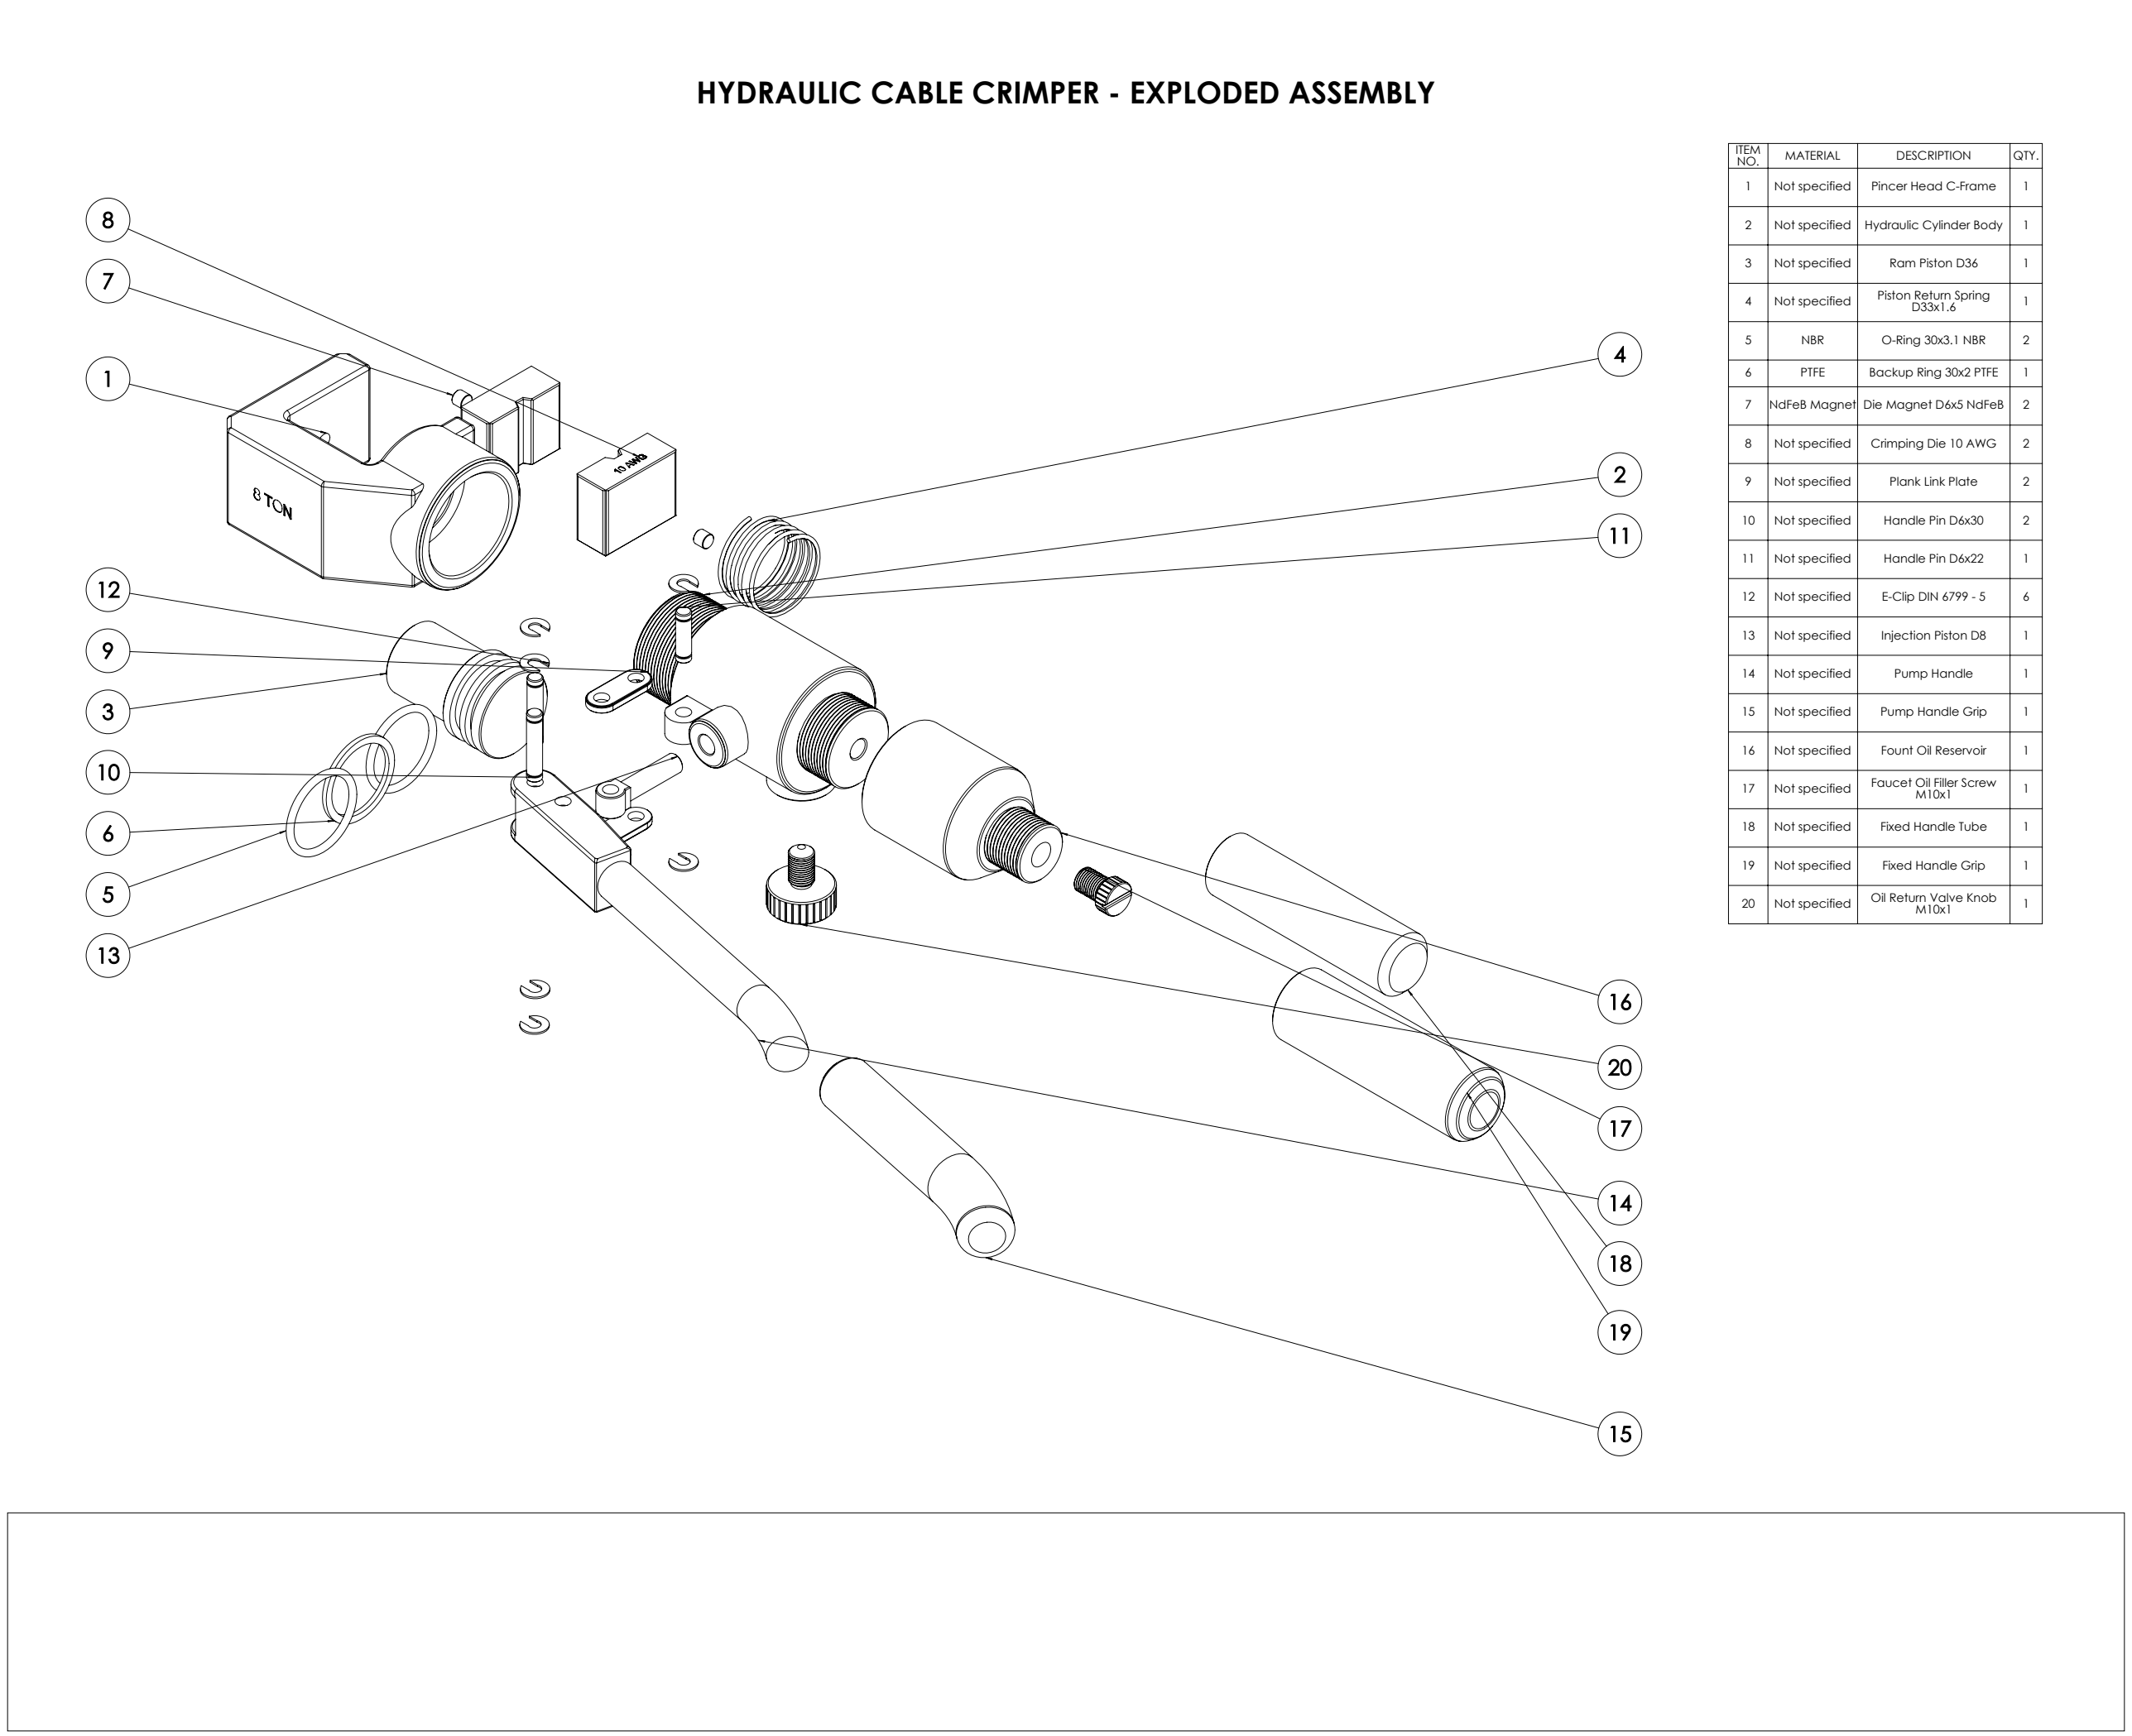
ISO-10303-21;
HEADER;
/* Generated by software containing ST-Developer
 * from STEP Tools, Inc. (www.steptools.com) 
 */

FILE_DESCRIPTION(
/* description */ (''),
/* implementation_level */ '2;1');

FILE_NAME(
/* name */ 'MAS-329',
/* time_stamp */ '2026-10-26T03:55:20-07:00',
/* author */ (''),
/* organization */ (''),
/* preprocessor_version */ 'ST-DEVELOPER v20.2',
/* originating_system */ 'Autodesk Translation Framework v15.15.0.0',
/* authorisation */ '');

FILE_SCHEMA (('AUTOMOTIVE_DESIGN { 1 0 10303 214 3 1 1 }'));
ENDSEC;

DATA;
#10=MECHANICAL_DESIGN_GEOMETRIC_PRESENTATION_REPRESENTATION('',(#175,#176,
#177,#178,#179,#180,#181,#182,#183,#184,#185,#186,#187,#188,#189,#190,#191,
#192,#193,#194),#45236);
#11=ITEM_DEFINED_TRANSFORMATION($,$,#16759,#18093);
#12=ITEM_DEFINED_TRANSFORMATION($,$,#16969,#18094);
#13=ITEM_DEFINED_TRANSFORMATION($,$,#17111,#18095);
#14=ITEM_DEFINED_TRANSFORMATION($,$,#17147,#18096);
#15=ITEM_DEFINED_TRANSFORMATION($,$,#17152,#18097);
#16=ITEM_DEFINED_TRANSFORMATION($,$,#17152,#18098);
#17=ITEM_DEFINED_TRANSFORMATION($,$,#17156,#18099);
#18=ITEM_DEFINED_TRANSFORMATION($,$,#17165,#18100);
#19=ITEM_DEFINED_TRANSFORMATION($,$,#17165,#18101);
#20=ITEM_DEFINED_TRANSFORMATION($,$,#17175,#18102);
#21=ITEM_DEFINED_TRANSFORMATION($,$,#17175,#18103);
#22=ITEM_DEFINED_TRANSFORMATION($,$,#17253,#18104);
#23=ITEM_DEFINED_TRANSFORMATION($,$,#18082,#18105);
#24=ITEM_DEFINED_TRANSFORMATION($,$,#18082,#18106);
#25=ITEM_DEFINED_TRANSFORMATION($,$,#17279,#18107);
#26=ITEM_DEFINED_TRANSFORMATION($,$,#17342,#18108);
#27=ITEM_DEFINED_TRANSFORMATION($,$,#17551,#18109);
#28=ITEM_DEFINED_TRANSFORMATION($,$,#17572,#18110);
#29=ITEM_DEFINED_TRANSFORMATION($,$,#17601,#18111);
#30=ITEM_DEFINED_TRANSFORMATION($,$,#17879,#18112);
#31=ITEM_DEFINED_TRANSFORMATION($,$,#17958,#18113);
#32=ITEM_DEFINED_TRANSFORMATION($,$,#17987,#18114);
#33=ITEM_DEFINED_TRANSFORMATION($,$,#17987,#18115);
#34=ITEM_DEFINED_TRANSFORMATION($,$,#18028,#18116);
#35=ITEM_DEFINED_TRANSFORMATION($,$,#18028,#18117);
#36=ITEM_DEFINED_TRANSFORMATION($,$,#18054,#18118);
#37=ITEM_DEFINED_TRANSFORMATION($,$,#18082,#18119);
#38=ITEM_DEFINED_TRANSFORMATION($,$,#18082,#18120);
#39=ITEM_DEFINED_TRANSFORMATION($,$,#18082,#18121);
#40=ITEM_DEFINED_TRANSFORMATION($,$,#18082,#18122);
#41=(
REPRESENTATION_RELATIONSHIP($,$,#45314,#45313)
REPRESENTATION_RELATIONSHIP_WITH_TRANSFORMATION(#11)
SHAPE_REPRESENTATION_RELATIONSHIP()
);
#42=(
REPRESENTATION_RELATIONSHIP($,$,#45315,#45313)
REPRESENTATION_RELATIONSHIP_WITH_TRANSFORMATION(#12)
SHAPE_REPRESENTATION_RELATIONSHIP()
);
#43=(
REPRESENTATION_RELATIONSHIP($,$,#45316,#45313)
REPRESENTATION_RELATIONSHIP_WITH_TRANSFORMATION(#13)
SHAPE_REPRESENTATION_RELATIONSHIP()
);
#44=(
REPRESENTATION_RELATIONSHIP($,$,#45317,#45313)
REPRESENTATION_RELATIONSHIP_WITH_TRANSFORMATION(#14)
SHAPE_REPRESENTATION_RELATIONSHIP()
);
#45=(
REPRESENTATION_RELATIONSHIP($,$,#45318,#45313)
REPRESENTATION_RELATIONSHIP_WITH_TRANSFORMATION(#15)
SHAPE_REPRESENTATION_RELATIONSHIP()
);
#46=(
REPRESENTATION_RELATIONSHIP($,$,#45318,#45313)
REPRESENTATION_RELATIONSHIP_WITH_TRANSFORMATION(#16)
SHAPE_REPRESENTATION_RELATIONSHIP()
);
#47=(
REPRESENTATION_RELATIONSHIP($,$,#45319,#45313)
REPRESENTATION_RELATIONSHIP_WITH_TRANSFORMATION(#17)
SHAPE_REPRESENTATION_RELATIONSHIP()
);
#48=(
REPRESENTATION_RELATIONSHIP($,$,#45320,#45313)
REPRESENTATION_RELATIONSHIP_WITH_TRANSFORMATION(#18)
SHAPE_REPRESENTATION_RELATIONSHIP()
);
#49=(
REPRESENTATION_RELATIONSHIP($,$,#45320,#45313)
REPRESENTATION_RELATIONSHIP_WITH_TRANSFORMATION(#19)
SHAPE_REPRESENTATION_RELATIONSHIP()
);
#50=(
REPRESENTATION_RELATIONSHIP($,$,#45321,#45313)
REPRESENTATION_RELATIONSHIP_WITH_TRANSFORMATION(#20)
SHAPE_REPRESENTATION_RELATIONSHIP()
);
#51=(
REPRESENTATION_RELATIONSHIP($,$,#45321,#45313)
REPRESENTATION_RELATIONSHIP_WITH_TRANSFORMATION(#21)
SHAPE_REPRESENTATION_RELATIONSHIP()
);
#52=(
REPRESENTATION_RELATIONSHIP($,$,#45322,#45313)
REPRESENTATION_RELATIONSHIP_WITH_TRANSFORMATION(#22)
SHAPE_REPRESENTATION_RELATIONSHIP()
);
#53=(
REPRESENTATION_RELATIONSHIP($,$,#45333,#45313)
REPRESENTATION_RELATIONSHIP_WITH_TRANSFORMATION(#23)
SHAPE_REPRESENTATION_RELATIONSHIP()
);
#54=(
REPRESENTATION_RELATIONSHIP($,$,#45333,#45313)
REPRESENTATION_RELATIONSHIP_WITH_TRANSFORMATION(#24)
SHAPE_REPRESENTATION_RELATIONSHIP()
);
#55=(
REPRESENTATION_RELATIONSHIP($,$,#45323,#45313)
REPRESENTATION_RELATIONSHIP_WITH_TRANSFORMATION(#25)
SHAPE_REPRESENTATION_RELATIONSHIP()
);
#56=(
REPRESENTATION_RELATIONSHIP($,$,#45324,#45313)
REPRESENTATION_RELATIONSHIP_WITH_TRANSFORMATION(#26)
SHAPE_REPRESENTATION_RELATIONSHIP()
);
#57=(
REPRESENTATION_RELATIONSHIP($,$,#45325,#45313)
REPRESENTATION_RELATIONSHIP_WITH_TRANSFORMATION(#27)
SHAPE_REPRESENTATION_RELATIONSHIP()
);
#58=(
REPRESENTATION_RELATIONSHIP($,$,#45326,#45313)
REPRESENTATION_RELATIONSHIP_WITH_TRANSFORMATION(#28)
SHAPE_REPRESENTATION_RELATIONSHIP()
);
#59=(
REPRESENTATION_RELATIONSHIP($,$,#45327,#45313)
REPRESENTATION_RELATIONSHIP_WITH_TRANSFORMATION(#29)
SHAPE_REPRESENTATION_RELATIONSHIP()
);
#60=(
REPRESENTATION_RELATIONSHIP($,$,#45328,#45313)
REPRESENTATION_RELATIONSHIP_WITH_TRANSFORMATION(#30)
SHAPE_REPRESENTATION_RELATIONSHIP()
);
#61=(
REPRESENTATION_RELATIONSHIP($,$,#45329,#45313)
REPRESENTATION_RELATIONSHIP_WITH_TRANSFORMATION(#31)
SHAPE_REPRESENTATION_RELATIONSHIP()
);
#62=(
REPRESENTATION_RELATIONSHIP($,$,#45330,#45313)
REPRESENTATION_RELATIONSHIP_WITH_TRANSFORMATION(#32)
SHAPE_REPRESENTATION_RELATIONSHIP()
);
#63=(
REPRESENTATION_RELATIONSHIP($,$,#45330,#45313)
REPRESENTATION_RELATIONSHIP_WITH_TRANSFORMATION(#33)
SHAPE_REPRESENTATION_RELATIONSHIP()
);
#64=(
REPRESENTATION_RELATIONSHIP($,$,#45331,#45313)
REPRESENTATION_RELATIONSHIP_WITH_TRANSFORMATION(#34)
SHAPE_REPRESENTATION_RELATIONSHIP()
);
#65=(
REPRESENTATION_RELATIONSHIP($,$,#45331,#45313)
REPRESENTATION_RELATIONSHIP_WITH_TRANSFORMATION(#35)
SHAPE_REPRESENTATION_RELATIONSHIP()
);
#66=(
REPRESENTATION_RELATIONSHIP($,$,#45332,#45313)
REPRESENTATION_RELATIONSHIP_WITH_TRANSFORMATION(#36)
SHAPE_REPRESENTATION_RELATIONSHIP()
);
#67=(
REPRESENTATION_RELATIONSHIP($,$,#45333,#45313)
REPRESENTATION_RELATIONSHIP_WITH_TRANSFORMATION(#37)
SHAPE_REPRESENTATION_RELATIONSHIP()
);
#68=(
REPRESENTATION_RELATIONSHIP($,$,#45333,#45313)
REPRESENTATION_RELATIONSHIP_WITH_TRANSFORMATION(#38)
SHAPE_REPRESENTATION_RELATIONSHIP()
);
#69=(
REPRESENTATION_RELATIONSHIP($,$,#45333,#45313)
REPRESENTATION_RELATIONSHIP_WITH_TRANSFORMATION(#39)
SHAPE_REPRESENTATION_RELATIONSHIP()
);
#70=(
REPRESENTATION_RELATIONSHIP($,$,#45333,#45313)
REPRESENTATION_RELATIONSHIP_WITH_TRANSFORMATION(#40)
SHAPE_REPRESENTATION_RELATIONSHIP()
);
#71=CONTEXT_DEPENDENT_SHAPE_REPRESENTATION(#41,#45283);
#72=CONTEXT_DEPENDENT_SHAPE_REPRESENTATION(#42,#45284);
#73=CONTEXT_DEPENDENT_SHAPE_REPRESENTATION(#43,#45285);
#74=CONTEXT_DEPENDENT_SHAPE_REPRESENTATION(#44,#45286);
#75=CONTEXT_DEPENDENT_SHAPE_REPRESENTATION(#45,#45287);
#76=CONTEXT_DEPENDENT_SHAPE_REPRESENTATION(#46,#45288);
#77=CONTEXT_DEPENDENT_SHAPE_REPRESENTATION(#47,#45289);
#78=CONTEXT_DEPENDENT_SHAPE_REPRESENTATION(#48,#45290);
#79=CONTEXT_DEPENDENT_SHAPE_REPRESENTATION(#49,#45291);
#80=CONTEXT_DEPENDENT_SHAPE_REPRESENTATION(#50,#45292);
#81=CONTEXT_DEPENDENT_SHAPE_REPRESENTATION(#51,#45293);
#82=CONTEXT_DEPENDENT_SHAPE_REPRESENTATION(#52,#45294);
#83=CONTEXT_DEPENDENT_SHAPE_REPRESENTATION(#53,#45295);
#84=CONTEXT_DEPENDENT_SHAPE_REPRESENTATION(#54,#45296);
#85=CONTEXT_DEPENDENT_SHAPE_REPRESENTATION(#55,#45297);
#86=CONTEXT_DEPENDENT_SHAPE_REPRESENTATION(#56,#45298);
#87=CONTEXT_DEPENDENT_SHAPE_REPRESENTATION(#57,#45299);
#88=CONTEXT_DEPENDENT_SHAPE_REPRESENTATION(#58,#45300);
#89=CONTEXT_DEPENDENT_SHAPE_REPRESENTATION(#59,#45301);
#90=CONTEXT_DEPENDENT_SHAPE_REPRESENTATION(#60,#45302);
#91=CONTEXT_DEPENDENT_SHAPE_REPRESENTATION(#61,#45303);
#92=CONTEXT_DEPENDENT_SHAPE_REPRESENTATION(#62,#45304);
#93=CONTEXT_DEPENDENT_SHAPE_REPRESENTATION(#63,#45305);
#94=CONTEXT_DEPENDENT_SHAPE_REPRESENTATION(#64,#45306);
#95=CONTEXT_DEPENDENT_SHAPE_REPRESENTATION(#65,#45307);
#96=CONTEXT_DEPENDENT_SHAPE_REPRESENTATION(#66,#45308);
#97=CONTEXT_DEPENDENT_SHAPE_REPRESENTATION(#67,#45309);
#98=CONTEXT_DEPENDENT_SHAPE_REPRESENTATION(#68,#45310);
#99=CONTEXT_DEPENDENT_SHAPE_REPRESENTATION(#69,#45311);
#100=CONTEXT_DEPENDENT_SHAPE_REPRESENTATION(#70,#45312);
#101=NEXT_ASSEMBLY_USAGE_OCCURRENCE('01_Pincer_Head_C-Frame:2',
'01_Pincer_Head_C-Frame:2','01_Pincer_Head_C-Frame:2',#45335,#45336,
'01_Pincer_Head_C-Frame:2');
#102=NEXT_ASSEMBLY_USAGE_OCCURRENCE('02_Hydraulic_Cylinder_Body:2',
'02_Hydraulic_Cylinder_Body:2','02_Hydraulic_Cylinder_Body:2',#45335,#45337,
'02_Hydraulic_Cylinder_Body:2');
#103=NEXT_ASSEMBLY_USAGE_OCCURRENCE('03_Ram_Piston_D36:2',
'03_Ram_Piston_D36:2','03_Ram_Piston_D36:2',#45335,#45338,
'03_Ram_Piston_D36:2');
#104=NEXT_ASSEMBLY_USAGE_OCCURRENCE('04_Piston_Return_Spring_D33x1.6:2',
'04_Piston_Return_Spring_D33x1.6:2','04_Piston_Return_Spring_D33x1.6:2',
#45335,#45339,'04_Piston_Return_Spring_D33x1.6:2');
#105=NEXT_ASSEMBLY_USAGE_OCCURRENCE('05_O-Ring_30x3.1_NBR:2',
'05_O-Ring_30x3.1_NBR:2','05_O-Ring_30x3.1_NBR:2',#45335,#45340,
'05_O-Ring_30x3.1_NBR:2');
#106=NEXT_ASSEMBLY_USAGE_OCCURRENCE('05_O-Ring_30x3.1_NBR:3',
'05_O-Ring_30x3.1_NBR:3','05_O-Ring_30x3.1_NBR:3',#45335,#45340,
'05_O-Ring_30x3.1_NBR:3');
#107=NEXT_ASSEMBLY_USAGE_OCCURRENCE('06_Backup_Ring_30x2_PTFE:2',
'06_Backup_Ring_30x2_PTFE:2','06_Backup_Ring_30x2_PTFE:2',#45335,#45341,
'06_Backup_Ring_30x2_PTFE:2');
#108=NEXT_ASSEMBLY_USAGE_OCCURRENCE('07_Die_Magnet_D6x5_NdFeB:2',
'07_Die_Magnet_D6x5_NdFeB:2','07_Die_Magnet_D6x5_NdFeB:2',#45335,#45342,
'07_Die_Magnet_D6x5_NdFeB:2');
#109=NEXT_ASSEMBLY_USAGE_OCCURRENCE('07_Die_Magnet_D6x5_NdFeB:3',
'07_Die_Magnet_D6x5_NdFeB:3','07_Die_Magnet_D6x5_NdFeB:3',#45335,#45342,
'07_Die_Magnet_D6x5_NdFeB:3');
#110=NEXT_ASSEMBLY_USAGE_OCCURRENCE('08_Crimping_Die_10_AWG:2',
'08_Crimping_Die_10_AWG:2','08_Crimping_Die_10_AWG:2',#45335,#45343,
'08_Crimping_Die_10_AWG:2');
#111=NEXT_ASSEMBLY_USAGE_OCCURRENCE('08_Crimping_Die_10_AWG:3',
'08_Crimping_Die_10_AWG:3','08_Crimping_Die_10_AWG:3',#45335,#45343,
'08_Crimping_Die_10_AWG:3');
#112=NEXT_ASSEMBLY_USAGE_OCCURRENCE('11_Handle_Pin_D6x22:2',
'11_Handle_Pin_D6x22:2','11_Handle_Pin_D6x22:2',#45335,#45344,
'11_Handle_Pin_D6x22:2');
#113=NEXT_ASSEMBLY_USAGE_OCCURRENCE('12_E-Clip_DIN_6799_-_5:2',
'12_E-Clip_DIN_6799_-_5:2','12_E-Clip_DIN_6799_-_5:2',#45335,#45355,
'12_E-Clip_DIN_6799_-_5:2');
#114=NEXT_ASSEMBLY_USAGE_OCCURRENCE('12_E-Clip_DIN_6799_-_5:3',
'12_E-Clip_DIN_6799_-_5:3','12_E-Clip_DIN_6799_-_5:3',#45335,#45355,
'12_E-Clip_DIN_6799_-_5:3');
#115=NEXT_ASSEMBLY_USAGE_OCCURRENCE('16_Fount_Oil_Reservoir:2',
'16_Fount_Oil_Reservoir:2','16_Fount_Oil_Reservoir:2',#45335,#45345,
'16_Fount_Oil_Reservoir:2');
#116=NEXT_ASSEMBLY_USAGE_OCCURRENCE(
'17_Faucet_Oil_Filler_Screw_M10x1:2',
'17_Faucet_Oil_Filler_Screw_M10x1:2',
'17_Faucet_Oil_Filler_Screw_M10x1:2',#45335,#45346,
'17_Faucet_Oil_Filler_Screw_M10x1:2');
#117=NEXT_ASSEMBLY_USAGE_OCCURRENCE('18_Fixed_Handle_Tube:2',
'18_Fixed_Handle_Tube:2','18_Fixed_Handle_Tube:2',#45335,#45347,
'18_Fixed_Handle_Tube:2');
#118=NEXT_ASSEMBLY_USAGE_OCCURRENCE('19_Fixed_Handle_Grip:2',
'19_Fixed_Handle_Grip:2','19_Fixed_Handle_Grip:2',#45335,#45348,
'19_Fixed_Handle_Grip:2');
#119=NEXT_ASSEMBLY_USAGE_OCCURRENCE('20_Oil_Return_Valve_Knob_M10x1:2',
'20_Oil_Return_Valve_Knob_M10x1:2','20_Oil_Return_Valve_Knob_M10x1:2',#45335,
#45349,'20_Oil_Return_Valve_Knob_M10x1:2');
#120=NEXT_ASSEMBLY_USAGE_OCCURRENCE('14_Pump_Handle:2',
'14_Pump_Handle:2','14_Pump_Handle:2',#45335,#45350,'14_Pump_Handle:2');
#121=NEXT_ASSEMBLY_USAGE_OCCURRENCE('15_Pump_Handle_Grip:2',
'15_Pump_Handle_Grip:2','15_Pump_Handle_Grip:2',#45335,#45351,
'15_Pump_Handle_Grip:2');
#122=NEXT_ASSEMBLY_USAGE_OCCURRENCE('09_Plank_Link_Plate:2',
'09_Plank_Link_Plate:2','09_Plank_Link_Plate:2',#45335,#45352,
'09_Plank_Link_Plate:2');
#123=NEXT_ASSEMBLY_USAGE_OCCURRENCE('09_Plank_Link_Plate:3',
'09_Plank_Link_Plate:3','09_Plank_Link_Plate:3',#45335,#45352,
'09_Plank_Link_Plate:3');
#124=NEXT_ASSEMBLY_USAGE_OCCURRENCE('10_Handle_Pin_D6x30:2',
'10_Handle_Pin_D6x30:2','10_Handle_Pin_D6x30:2',#45335,#45353,
'10_Handle_Pin_D6x30:2');
#125=NEXT_ASSEMBLY_USAGE_OCCURRENCE('10_Handle_Pin_D6x30:3',
'10_Handle_Pin_D6x30:3','10_Handle_Pin_D6x30:3',#45335,#45353,
'10_Handle_Pin_D6x30:3');
#126=NEXT_ASSEMBLY_USAGE_OCCURRENCE('13_Injection_Piston_D8:2',
'13_Injection_Piston_D8:2','13_Injection_Piston_D8:2',#45335,#45354,
'13_Injection_Piston_D8:2');
#127=NEXT_ASSEMBLY_USAGE_OCCURRENCE('12_E-Clip_DIN_6799_-_5:4',
'12_E-Clip_DIN_6799_-_5:4','12_E-Clip_DIN_6799_-_5:4',#45335,#45355,
'12_E-Clip_DIN_6799_-_5:4');
#128=NEXT_ASSEMBLY_USAGE_OCCURRENCE('12_E-Clip_DIN_6799_-_5:5',
'12_E-Clip_DIN_6799_-_5:5','12_E-Clip_DIN_6799_-_5:5',#45335,#45355,
'12_E-Clip_DIN_6799_-_5:5');
#129=NEXT_ASSEMBLY_USAGE_OCCURRENCE('12_E-Clip_DIN_6799_-_5:6',
'12_E-Clip_DIN_6799_-_5:6','12_E-Clip_DIN_6799_-_5:6',#45335,#45355,
'12_E-Clip_DIN_6799_-_5:6');
#130=NEXT_ASSEMBLY_USAGE_OCCURRENCE('12_E-Clip_DIN_6799_-_5:7',
'12_E-Clip_DIN_6799_-_5:7','12_E-Clip_DIN_6799_-_5:7',#45335,#45355,
'12_E-Clip_DIN_6799_-_5:7');
#131=(
BOUNDED_CURVE()
B_SPLINE_CURVE(2,(#38201,#38202,#38203),.UNSPECIFIED.,.F.,.F.)
B_SPLINE_CURVE_WITH_KNOTS((3,3),(0.,0.0727386053931439),.UNSPECIFIED.)
CURVE()
GEOMETRIC_REPRESENTATION_ITEM()
RATIONAL_B_SPLINE_CURVE((1.,1.,1.))
REPRESENTATION_ITEM('')
);
#132=(
BOUNDED_CURVE()
B_SPLINE_CURVE(2,(#38207,#38208,#38209),.UNSPECIFIED.,.F.,.F.)
B_SPLINE_CURVE_WITH_KNOTS((3,3),(0.,0.0727386053931439),.UNSPECIFIED.)
CURVE()
GEOMETRIC_REPRESENTATION_ITEM()
RATIONAL_B_SPLINE_CURVE((1.,1.,1.))
REPRESENTATION_ITEM('')
);
#133=(
BOUNDED_CURVE()
B_SPLINE_CURVE(2,(#38220,#38221,#38222),.UNSPECIFIED.,.F.,.F.)
B_SPLINE_CURVE_WITH_KNOTS((3,3),(0.,0.0727386053931439),.UNSPECIFIED.)
CURVE()
GEOMETRIC_REPRESENTATION_ITEM()
RATIONAL_B_SPLINE_CURVE((1.,1.,1.))
REPRESENTATION_ITEM('')
);
#134=(
BOUNDED_CURVE()
B_SPLINE_CURVE(2,(#38226,#38227,#38228),.UNSPECIFIED.,.F.,.F.)
B_SPLINE_CURVE_WITH_KNOTS((3,3),(0.,0.0727386053931439),.UNSPECIFIED.)
CURVE()
GEOMETRIC_REPRESENTATION_ITEM()
RATIONAL_B_SPLINE_CURVE((1.,1.,1.))
REPRESENTATION_ITEM('')
);
#135=SHAPE_REPRESENTATION_RELATIONSHIP('SRR','None',#45314,#155);
#136=SHAPE_REPRESENTATION_RELATIONSHIP('SRR','None',#45315,#156);
#137=SHAPE_REPRESENTATION_RELATIONSHIP('SRR','None',#45316,#157);
#138=SHAPE_REPRESENTATION_RELATIONSHIP('SRR','None',#45317,#158);
#139=SHAPE_REPRESENTATION_RELATIONSHIP('SRR','None',#45318,#159);
#140=SHAPE_REPRESENTATION_RELATIONSHIP('SRR','None',#45319,#160);
#141=SHAPE_REPRESENTATION_RELATIONSHIP('SRR','None',#45320,#161);
#142=SHAPE_REPRESENTATION_RELATIONSHIP('SRR','None',#45321,#162);
#143=SHAPE_REPRESENTATION_RELATIONSHIP('SRR','None',#45322,#163);
#144=SHAPE_REPRESENTATION_RELATIONSHIP('SRR','None',#45323,#164);
#145=SHAPE_REPRESENTATION_RELATIONSHIP('SRR','None',#45324,#165);
#146=SHAPE_REPRESENTATION_RELATIONSHIP('SRR','None',#45325,#166);
#147=SHAPE_REPRESENTATION_RELATIONSHIP('SRR','None',#45326,#167);
#148=SHAPE_REPRESENTATION_RELATIONSHIP('SRR','None',#45327,#168);
#149=SHAPE_REPRESENTATION_RELATIONSHIP('SRR','None',#45328,#169);
#150=SHAPE_REPRESENTATION_RELATIONSHIP('SRR','None',#45329,#170);
#151=SHAPE_REPRESENTATION_RELATIONSHIP('SRR','None',#45330,#171);
#152=SHAPE_REPRESENTATION_RELATIONSHIP('SRR','None',#45331,#172);
#153=SHAPE_REPRESENTATION_RELATIONSHIP('SRR','None',#45332,#173);
#154=SHAPE_REPRESENTATION_RELATIONSHIP('SRR','None',#45333,#174);
#155=ADVANCED_BREP_SHAPE_REPRESENTATION('',(#195),#45216);
#156=ADVANCED_BREP_SHAPE_REPRESENTATION('',(#196),#45217);
#157=ADVANCED_BREP_SHAPE_REPRESENTATION('',(#197),#45218);
#158=ADVANCED_BREP_SHAPE_REPRESENTATION('',(#198),#45219);
#159=ADVANCED_BREP_SHAPE_REPRESENTATION('',(#199),#45220);
#160=ADVANCED_BREP_SHAPE_REPRESENTATION('',(#200),#45221);
#161=ADVANCED_BREP_SHAPE_REPRESENTATION('',(#201),#45222);
#162=ADVANCED_BREP_SHAPE_REPRESENTATION('',(#202),#45223);
#163=ADVANCED_BREP_SHAPE_REPRESENTATION('',(#203),#45224);
#164=ADVANCED_BREP_SHAPE_REPRESENTATION('',(#204),#45225);
#165=ADVANCED_BREP_SHAPE_REPRESENTATION('',(#205),#45226);
#166=ADVANCED_BREP_SHAPE_REPRESENTATION('',(#206),#45227);
#167=ADVANCED_BREP_SHAPE_REPRESENTATION('',(#207),#45228);
#168=ADVANCED_BREP_SHAPE_REPRESENTATION('',(#208),#45229);
#169=ADVANCED_BREP_SHAPE_REPRESENTATION('',(#209),#45230);
#170=ADVANCED_BREP_SHAPE_REPRESENTATION('',(#210),#45231);
#171=ADVANCED_BREP_SHAPE_REPRESENTATION('',(#211),#45232);
#172=ADVANCED_BREP_SHAPE_REPRESENTATION('',(#212),#45233);
#173=ADVANCED_BREP_SHAPE_REPRESENTATION('',(#213),#45234);
#174=ADVANCED_BREP_SHAPE_REPRESENTATION('',(#214),#45235);
#175=STYLED_ITEM('',(#45463),#195);
#176=STYLED_ITEM('',(#45463),#196);
#177=STYLED_ITEM('',(#45498),#197);
#178=STYLED_ITEM('',(#45484),#198);
#179=STYLED_ITEM('',(#45491),#199);
#180=STYLED_ITEM('',(#45498),#200);
#181=STYLED_ITEM('',(#45470),#201);
#182=STYLED_ITEM('',(#45477),#202);
#183=STYLED_ITEM('',(#45484),#203);
#184=STYLED_ITEM('',(#45498),#204);
#185=STYLED_ITEM('',(#45491),#205);
#186=STYLED_ITEM('',(#45477),#206);
#187=STYLED_ITEM('',(#45491),#207);
#188=STYLED_ITEM('',(#45477),#208);
#189=STYLED_ITEM('',(#45498),#209);
#190=STYLED_ITEM('',(#45491),#210);
#191=STYLED_ITEM('',(#45498),#211);
#192=STYLED_ITEM('',(#45484),#212);
#193=STYLED_ITEM('',(#45477),#213);
#194=STYLED_ITEM('',(#45470),#214);
#195=MANIFOLD_SOLID_BREP('Body1',#16517);
#196=MANIFOLD_SOLID_BREP('Body1',#16518);
#197=MANIFOLD_SOLID_BREP('Body1',#16519);
#198=MANIFOLD_SOLID_BREP('Body1',#16520);
#199=MANIFOLD_SOLID_BREP('Body1',#16521);
#200=MANIFOLD_SOLID_BREP('Body1',#16522);
#201=MANIFOLD_SOLID_BREP('Body1',#16523);
#202=MANIFOLD_SOLID_BREP('Body1',#16524);
#203=MANIFOLD_SOLID_BREP('Body1',#16525);
#204=MANIFOLD_SOLID_BREP('Body1',#16526);
#205=MANIFOLD_SOLID_BREP('Body1',#16527);
#206=MANIFOLD_SOLID_BREP('Body1',#16528);
#207=MANIFOLD_SOLID_BREP('Body1',#16529);
#208=MANIFOLD_SOLID_BREP('Body1',#16530);
#209=MANIFOLD_SOLID_BREP('Body1',#16531);
#210=MANIFOLD_SOLID_BREP('Body1',#16532);
#211=MANIFOLD_SOLID_BREP('Body1',#16533);
#212=MANIFOLD_SOLID_BREP('Body1',#16534);
#213=MANIFOLD_SOLID_BREP('Body1',#16535);
#214=MANIFOLD_SOLID_BREP('Body1',#16536);
#215=TOROIDAL_SURFACE('',#16890,25.3786796564404,1.5);
#216=TOROIDAL_SURFACE('',#16900,25.5,1.5);
#217=TOROIDAL_SURFACE('',#16910,25.5,1.5);
#218=TOROIDAL_SURFACE('',#16914,4.5,1.5);
#219=TOROIDAL_SURFACE('',#16920,4.5,1.5);
#220=TOROIDAL_SURFACE('',#16924,4.5,1.5);
#221=TOROIDAL_SURFACE('',#16926,25.5,1.5);
#222=TOROIDAL_SURFACE('',#16927,4.5,1.5);
#223=TOROIDAL_SURFACE('',#16932,25.5,1.5);
#224=TOROIDAL_SURFACE('',#17153,16.52,1.465);
#225=TOROIDAL_SURFACE('',#17931,8.,1.);
#226=TOROIDAL_SURFACE('',#17938,8.,1.);
#227=TOROIDAL_SURFACE('',#17951,79.9999999999995,8.);
#228=TOROIDAL_SURFACE('',#17970,7.,4.);
#229=TOROIDAL_SURFACE('',#17981,79.9999999999995,8.);
#230=TOROIDAL_SURFACE('',#17985,79.9999999999995,11.);
#231=SPHERICAL_SURFACE('',#16793,1.5);
#232=SPHERICAL_SURFACE('',#16796,1.5);
#233=SPHERICAL_SURFACE('',#16802,1.5);
#234=SPHERICAL_SURFACE('',#16808,1.5);
#235=SPHERICAL_SURFACE('',#16812,1.5);
#236=SPHERICAL_SURFACE('',#16817,1.5);
#237=SPHERICAL_SURFACE('',#16821,1.5);
#238=SPHERICAL_SURFACE('',#16827,1.5);
#239=SPHERICAL_SURFACE('',#16830,1.5);
#240=SPHERICAL_SURFACE('',#16836,1.5);
#241=SPHERICAL_SURFACE('',#16842,1.5);
#242=SPHERICAL_SURFACE('',#16848,1.5);
#243=SPHERICAL_SURFACE('',#16853,1.5);
#244=SPHERICAL_SURFACE('',#16874,1.5);
#245=SPHERICAL_SURFACE('',#16880,1.5);
#246=ELLIPSE('',#16775,30.3654774451956,27.);
#247=ELLIPSE('',#16782,46.4525564420302,27.);
#248=ELLIPSE('',#17373,9.89949493661173,7.);
#249=ELLIPSE('',#17374,9.89949493661173,7.);
#250=ELLIPSE('',#17378,9.89949493661173,7.);
#251=ELLIPSE('',#17379,9.89949493661173,7.);
#252=ELLIPSE('',#17900,10.8879054120476,8.);
#253=ELLIPSE('',#17908,10.8879054120476,8.);
#254=ELLIPSE('',#17918,1.00079713248425,1.);
#255=ELLIPSE('',#17937,1.00079713248425,1.);
#256=B_SPLINE_CURVE_WITH_KNOTS('',3,(#22232,#22233,#22234,#22235,#22236,
#22237,#22238,#22239,#22240,#22241,#22242,#22243,#22244,#22245,#22246,#22247,
#22248,#22249,#22250,#22251,#22252,#22253,#22254,#22255,#22256,#22257,#22258,
#22259,#22260,#22261,#22262,#22263,#22264,#22265,#22266,#22267,#22268,#22269,
#22270,#22271,#22272,#22273,#22274,#22275,#22276,#22277,#22278,#22279,#22280,
#22281,#22282,#22283,#22284,#22285,#22286),.UNSPECIFIED.,.F.,.F.,(4,3,3,
3,3,3,3,3,3,3,3,3,3,3,3,3,3,3,4),(0.,0.045710607901934,0.0936977578945001,
0.144847111669027,0.20140314890997,0.272909847076527,0.34684212796304,0.403542711042019,
0.454759213428076,0.503663771096975,0.553082777660006,0.60625025134459,
0.667135318470237,0.750351488852678,0.812763616639508,0.865509180697515,
0.91510065731714,0.961342755203381,1.),.UNSPECIFIED.);
#257=B_SPLINE_CURVE_WITH_KNOTS('',3,(#22288,#22289,#22290,#22291),
 .UNSPECIFIED.,.F.,.F.,(4,4),(0.,1.),.UNSPECIFIED.);
#258=B_SPLINE_CURVE_WITH_KNOTS('',3,(#22293,#22294,#22295,#22296,#22297,
#22298,#22299,#22300,#22301,#22302,#22303,#22304,#22305,#22306,#22307,#22308,
#22309,#22310,#22311,#22312,#22313,#22314,#22315,#22316,#22317,#22318,#22319,
#22320,#22321,#22322,#22323,#22324,#22325,#22326,#22327,#22328,#22329,#22330,
#22331,#22332,#22333,#22334,#22335,#22336,#22337,#22338,#22339,#22340,#22341,
#22342,#22343,#22344,#22345,#22346,#22347),.UNSPECIFIED.,.F.,.F.,(4,3,3,
3,3,3,3,3,3,3,3,3,3,3,3,3,3,3,4),(0.,0.0457165824991635,0.0937104844515761,
0.144867913797289,0.201436011576242,0.27297908229306,0.346880659378771,
0.403581201094802,0.454799677982589,0.503723597905468,0.553141531246011,
0.606309913173532,0.667202763475632,0.750402072606724,0.812801554455043,
0.865537008236129,0.915120309500579,0.961355859688362,1.),.UNSPECIFIED.);
#259=B_SPLINE_CURVE_WITH_KNOTS('',3,(#22370,#22371,#22372,#22373,#22374),
 .UNSPECIFIED.,.F.,.F.,(4,1,4),(-1.66265780683826,-0.950090175336147,8.76618254786689E-34),
 .UNSPECIFIED.);
#260=B_SPLINE_CURVE_WITH_KNOTS('',3,(#22377,#22378,#22379,#22380,#22381),
 .UNSPECIFIED.,.F.,.F.,(4,1,4),(-8.76618254786689E-34,0.950090175336147,
1.66265780683826),.UNSPECIFIED.);
#261=B_SPLINE_CURVE_WITH_KNOTS('',3,(#22452,#22453,#22454,#22455,#22456,
#22457,#22458,#22459,#22460,#22461,#22462,#22463,#22464,#22465,#22466,#22467,
#22468,#22469,#22470,#22471,#22472,#22473,#22474,#22475,#22476,#22477,#22478,
#22479,#22480,#22481,#22482,#22483,#22484,#22485,#22486,#22487,#22488,#22489,
#22490,#22491,#22492,#22493,#22494,#22495,#22496,#22497,#22498,#22499,#22500,
#22501,#22502,#22503,#22504,#22505,#22506),.UNSPECIFIED.,.F.,.F.,(4,3,3,
3,3,3,3,3,3,3,3,3,3,3,3,3,3,3,4),(0.,0.0454739962515773,0.0931998981823239,
0.144047233375039,0.200179420009566,0.270609269371814,0.345305256937859,
0.401904934183246,0.452978957125852,0.503375918080837,0.552516920031195,
0.605334615481369,0.665679077650195,0.749259308237646,0.811944481178235,
0.864470546131162,0.91385478632005,0.959883517726927,1.),.UNSPECIFIED.);
#262=B_SPLINE_CURVE_WITH_KNOTS('',3,(#22508,#22509,#22510,#22511),
 .UNSPECIFIED.,.F.,.F.,(4,4),(-1.,0.),.UNSPECIFIED.);
#263=B_SPLINE_CURVE_WITH_KNOTS('',3,(#22513,#22514,#22515,#22516,#22517,
#22518,#22519,#22520,#22521,#22522,#22523,#22524,#22525,#22526,#22527,#22528,
#22529,#22530,#22531,#22532,#22533,#22534,#22535,#22536,#22537,#22538,#22539,
#22540,#22541,#22542,#22543,#22544,#22545,#22546,#22547,#22548,#22549,#22550,
#22551,#22552,#22553,#22554,#22555,#22556,#22557,#22558,#22559,#22560,#22561,
#22562,#22563,#22564,#22565,#22566,#22567),.UNSPECIFIED.,.F.,.F.,(4,3,3,
3,3,3,3,3,3,3,3,3,3,3,3,3,3,3,4),(0.,0.0454759500687694,0.0932040608878028,
0.144054037760376,0.200190152021456,0.270631477875933,0.345316813881959,
0.401916574351127,0.452991295574466,0.503400827180246,0.552541816304096,
0.605360167195349,0.665708324703348,0.749281243527511,0.811960932645634,
0.864483394812729,0.913864760430574,0.959891262991555,1.),.UNSPECIFIED.);
#264=B_SPLINE_CURVE_WITH_KNOTS('',3,(#22595,#22596,#22597,#22598,#22599,
#22600,#22601,#22602,#22603,#22604,#22605,#22606,#22607,#22608,#22609,#22610,
#22611,#22612,#22613,#22614,#22615,#22616,#22617,#22618,#22619,#22620,#22621,
#22622,#22623,#22624,#22625,#22626,#22627,#22628,#22629,#22630,#22631,#22632,
#22633,#22634,#22635,#22636,#22637,#22638,#22639,#22640,#22641,#22642,#22643,
#22644,#22645,#22646,#22647,#22648,#22649),.UNSPECIFIED.,.F.,.F.,(4,3,3,
3,3,3,3,3,3,3,3,3,3,3,3,3,3,3,4),(0.,0.0454739962517236,0.0931998981821424,
0.144047233377289,0.200179420014148,0.270609269376805,0.345305256939856,
0.401904934184723,0.452978957126951,0.503375918082738,0.552516920034218,
0.605334615484988,0.665679077654914,0.749259308241186,0.811944481180889,
0.864470546134333,0.913854786323009,0.959883517729389,1.),.UNSPECIFIED.);
#265=B_SPLINE_CURVE_WITH_KNOTS('',3,(#22651,#22652,#22653,#22654),
 .UNSPECIFIED.,.F.,.F.,(4,4),(0.,1.),.UNSPECIFIED.);
#266=B_SPLINE_CURVE_WITH_KNOTS('',3,(#22656,#22657,#22658,#22659,#22660,
#22661,#22662,#22663,#22664,#22665,#22666,#22667,#22668,#22669,#22670,#22671,
#22672,#22673,#22674,#22675,#22676,#22677,#22678,#22679,#22680,#22681,#22682,
#22683,#22684,#22685,#22686,#22687,#22688,#22689,#22690,#22691,#22692,#22693,
#22694,#22695,#22696,#22697,#22698,#22699,#22700,#22701,#22702,#22703,#22704,
#22705,#22706,#22707,#22708,#22709,#22710),.UNSPECIFIED.,.F.,.F.,(4,3,3,
3,3,3,3,3,3,3,3,3,3,3,3,3,3,3,4),(0.,0.0454759500669044,0.0932040608838389,
0.144054037755869,0.200190152008621,0.270631477848411,0.345316813870146,
0.401916574343999,0.4529912955674,0.503400827166756,0.552541816289859,0.605360167180691,
0.665708324686459,0.749281243514844,0.811960932636133,0.864483394804765,
0.913864760422638,0.959891262983851,1.),.UNSPECIFIED.);
#267=B_SPLINE_CURVE_WITH_KNOTS('',3,(#22729,#22730,#22731,#22732),
 .UNSPECIFIED.,.F.,.F.,(4,4),(1.38548660592135,2.14032342811115),
 .UNSPECIFIED.);
#268=B_SPLINE_CURVE_WITH_KNOTS('',3,(#22735,#22736,#22737,#22738),
 .UNSPECIFIED.,.F.,.F.,(4,4),(-2.14032342811115,-1.38548660592135),
 .UNSPECIFIED.);
#269=B_SPLINE_CURVE_WITH_KNOTS('',3,(#22759,#22760,#22761,#22762),
 .UNSPECIFIED.,.F.,.F.,(4,4),(-1.33701776267244,-0.785398163397445),
 .UNSPECIFIED.);
#270=B_SPLINE_CURVE_WITH_KNOTS('',3,(#22765,#22766,#22767,#22768),
 .UNSPECIFIED.,.F.,.F.,(4,4),(0.785398163397445,1.33701776267244),
 .UNSPECIFIED.);
#271=B_SPLINE_CURVE_WITH_KNOTS('',3,(#22785,#22786,#22787,#22788),
 .UNSPECIFIED.,.F.,.F.,(4,4),(-2.35619449019235,-2.14032342811107),
 .UNSPECIFIED.);
#272=B_SPLINE_CURVE_WITH_KNOTS('',3,(#22789,#22790,#22791,#22792),
 .UNSPECIFIED.,.F.,.F.,(4,4),(2.14032342811107,2.35619449019235),
 .UNSPECIFIED.);
#273=B_SPLINE_CURVE_WITH_KNOTS('',3,(#22818,#22819,#22820,#22821),
 .UNSPECIFIED.,.F.,.F.,(4,4),(-1.5707963267949,-1.33701776267243),
 .UNSPECIFIED.);
#274=B_SPLINE_CURVE_WITH_KNOTS('',3,(#22822,#22823,#22824,#22825),
 .UNSPECIFIED.,.F.,.F.,(4,4),(1.33701776267243,1.5707963267949),
 .UNSPECIFIED.);
#275=B_SPLINE_CURVE_WITH_KNOTS('',3,(#22846,#22847,#22848,#22849),
 .UNSPECIFIED.,.F.,.F.,(4,4),(-1.33701776267244,-0.785398163397449),
 .UNSPECIFIED.);
#276=B_SPLINE_CURVE_WITH_KNOTS('',3,(#22852,#22853,#22854,#22855),
 .UNSPECIFIED.,.F.,.F.,(4,4),(0.785398163397449,1.33701776267244),
 .UNSPECIFIED.);
#277=B_SPLINE_CURVE_WITH_KNOTS('',3,(#22872,#22873,#22874,#22875),
 .UNSPECIFIED.,.F.,.F.,(4,4),(1.33701776267244,1.5707963267949),
 .UNSPECIFIED.);
#278=B_SPLINE_CURVE_WITH_KNOTS('',3,(#22876,#22877,#22878,#22879),
 .UNSPECIFIED.,.F.,.F.,(4,4),(-1.5707963267949,-1.33701776267244),
 .UNSPECIFIED.);
#279=B_SPLINE_CURVE_WITH_KNOTS('',3,(#22897,#22898,#22899,#22900),
 .UNSPECIFIED.,.F.,.F.,(4,4),(1.38548660592135,2.14032342811115),
 .UNSPECIFIED.);
#280=B_SPLINE_CURVE_WITH_KNOTS('',3,(#22903,#22904,#22905,#22906),
 .UNSPECIFIED.,.F.,.F.,(4,4),(-2.14032342811115,-1.38548660592135),
 .UNSPECIFIED.);
#281=B_SPLINE_CURVE_WITH_KNOTS('',3,(#22923,#22924,#22925,#22926),
 .UNSPECIFIED.,.F.,.F.,(4,4),(2.14032342811108,2.35619449019234),
 .UNSPECIFIED.);
#282=B_SPLINE_CURVE_WITH_KNOTS('',3,(#22927,#22928,#22929,#22930),
 .UNSPECIFIED.,.F.,.F.,(4,4),(-2.35619449019234,-2.14032342811108),
 .UNSPECIFIED.);
#283=B_SPLINE_CURVE_WITH_KNOTS('',3,(#22971,#22972,#22973,#22974,#22975,
#22976,#22977,#22978,#22979,#22980,#22981,#22982),.UNSPECIFIED.,.F.,.F.,
(4,2,2,2,2,4),(0.,0.0283853554165653,0.0567707108331306,0.113541421666261,
0.206773466476135,0.300005511286008),.UNSPECIFIED.);
#284=B_SPLINE_CURVE_WITH_KNOTS('',3,(#22988,#22989,#22990,#22991,#22992,
#22993,#22994,#22995,#22996,#22997),.UNSPECIFIED.,.F.,.F.,(4,2,2,2,4),(0.328734721229726,
0.593926356430402,0.667111024695369,0.687829707063932,0.708548389432494),
 .UNSPECIFIED.);
#285=B_SPLINE_CURVE_WITH_KNOTS('',3,(#23011,#23012,#23013,#23014,#23015,
#23016,#23017,#23018),.UNSPECIFIED.,.F.,.F.,(4,2,2,4),(0.894852523096926,
0.994118550241906,1.09338457738688,1.10550146254272),.UNSPECIFIED.);
#286=B_SPLINE_CURVE_WITH_KNOTS('',3,(#23023,#23024,#23025,#23026,#23027,
#23028,#23029,#23030,#23031,#23032,#23033,#23034),.UNSPECIFIED.,.F.,.F.,
(4,2,2,2,2,4),(0.,0.0283853554165652,0.0567707108331305,0.113541421666261,
0.206773466476134,0.300005511286007),.UNSPECIFIED.);
#287=B_SPLINE_CURVE_WITH_KNOTS('',2,(#23117,#23118,#23119),
 .UNSPECIFIED.,.F.,.F.,(3,3),(0.,1.),.UNSPECIFIED.);
#288=B_SPLINE_CURVE_WITH_KNOTS('',2,(#23121,#23122,#23123),
 .UNSPECIFIED.,.F.,.F.,(3,3),(0.,1.),.UNSPECIFIED.);
#289=B_SPLINE_CURVE_WITH_KNOTS('',2,(#23125,#23126,#23127),
 .UNSPECIFIED.,.F.,.F.,(3,3),(0.,1.),.UNSPECIFIED.);
#290=B_SPLINE_CURVE_WITH_KNOTS('',2,(#23129,#23130,#23131),
 .UNSPECIFIED.,.F.,.F.,(3,3),(0.,1.),.UNSPECIFIED.);
#291=B_SPLINE_CURVE_WITH_KNOTS('',2,(#23133,#23134,#23135),
 .UNSPECIFIED.,.F.,.F.,(3,3),(0.,1.),.UNSPECIFIED.);
#292=B_SPLINE_CURVE_WITH_KNOTS('',2,(#23137,#23138,#23139),
 .UNSPECIFIED.,.F.,.F.,(3,3),(0.,1.),.UNSPECIFIED.);
#293=B_SPLINE_CURVE_WITH_KNOTS('',2,(#23141,#23142,#23143),
 .UNSPECIFIED.,.F.,.F.,(3,3),(0.,1.),.UNSPECIFIED.);
#294=B_SPLINE_CURVE_WITH_KNOTS('',2,(#23145,#23146,#23147),
 .UNSPECIFIED.,.F.,.F.,(3,3),(0.,1.),.UNSPECIFIED.);
#295=B_SPLINE_CURVE_WITH_KNOTS('',2,(#23149,#23150,#23151),
 .UNSPECIFIED.,.F.,.F.,(3,3),(0.,1.),.UNSPECIFIED.);
#296=B_SPLINE_CURVE_WITH_KNOTS('',2,(#23153,#23154,#23155),
 .UNSPECIFIED.,.F.,.F.,(3,3),(0.,1.),.UNSPECIFIED.);
#297=B_SPLINE_CURVE_WITH_KNOTS('',2,(#23156,#23157,#23158),
 .UNSPECIFIED.,.F.,.F.,(3,3),(0.,1.),.UNSPECIFIED.);
#298=B_SPLINE_CURVE_WITH_KNOTS('',2,(#23177,#23178,#23179),
 .UNSPECIFIED.,.F.,.F.,(3,3),(0.,1.),.UNSPECIFIED.);
#299=B_SPLINE_CURVE_WITH_KNOTS('',2,(#23181,#23182,#23183),
 .UNSPECIFIED.,.F.,.F.,(3,3),(0.,1.),.UNSPECIFIED.);
#300=B_SPLINE_CURVE_WITH_KNOTS('',2,(#23185,#23186,#23187),
 .UNSPECIFIED.,.F.,.F.,(3,3),(0.,1.),.UNSPECIFIED.);
#301=B_SPLINE_CURVE_WITH_KNOTS('',2,(#23189,#23190,#23191),
 .UNSPECIFIED.,.F.,.F.,(3,3),(0.,1.),.UNSPECIFIED.);
#302=B_SPLINE_CURVE_WITH_KNOTS('',2,(#23193,#23194,#23195),
 .UNSPECIFIED.,.F.,.F.,(3,3),(0.,1.),.UNSPECIFIED.);
#303=B_SPLINE_CURVE_WITH_KNOTS('',2,(#23197,#23198,#23199),
 .UNSPECIFIED.,.F.,.F.,(3,3),(0.,1.),.UNSPECIFIED.);
#304=B_SPLINE_CURVE_WITH_KNOTS('',2,(#23201,#23202,#23203),
 .UNSPECIFIED.,.F.,.F.,(3,3),(0.,1.),.UNSPECIFIED.);
#305=B_SPLINE_CURVE_WITH_KNOTS('',2,(#23205,#23206,#23207),
 .UNSPECIFIED.,.F.,.F.,(3,3),(0.,1.),.UNSPECIFIED.);
#306=B_SPLINE_CURVE_WITH_KNOTS('',2,(#23209,#23210,#23211),
 .UNSPECIFIED.,.F.,.F.,(3,3),(0.,1.),.UNSPECIFIED.);
#307=B_SPLINE_CURVE_WITH_KNOTS('',2,(#23213,#23214,#23215),
 .UNSPECIFIED.,.F.,.F.,(3,3),(0.,1.),.UNSPECIFIED.);
#308=B_SPLINE_CURVE_WITH_KNOTS('',2,(#23217,#23218,#23219),
 .UNSPECIFIED.,.F.,.F.,(3,3),(0.,1.),.UNSPECIFIED.);
#309=B_SPLINE_CURVE_WITH_KNOTS('',2,(#23221,#23222,#23223),
 .UNSPECIFIED.,.F.,.F.,(3,3),(0.,1.),.UNSPECIFIED.);
#310=B_SPLINE_CURVE_WITH_KNOTS('',2,(#23225,#23226,#23227),
 .UNSPECIFIED.,.F.,.F.,(3,3),(0.,1.),.UNSPECIFIED.);
#311=B_SPLINE_CURVE_WITH_KNOTS('',2,(#23229,#23230,#23231),
 .UNSPECIFIED.,.F.,.F.,(3,3),(0.,1.),.UNSPECIFIED.);
#312=B_SPLINE_CURVE_WITH_KNOTS('',2,(#23233,#23234,#23235),
 .UNSPECIFIED.,.F.,.F.,(3,3),(0.,1.),.UNSPECIFIED.);
#313=B_SPLINE_CURVE_WITH_KNOTS('',2,(#23236,#23237,#23238),
 .UNSPECIFIED.,.F.,.F.,(3,3),(0.,1.),.UNSPECIFIED.);
#314=B_SPLINE_CURVE_WITH_KNOTS('',3,(#23280,#23281,#23282,#23283,#23284,
#23285,#23286,#23287,#23288,#23289,#23290,#23291),.UNSPECIFIED.,.F.,.F.,
(4,2,2,2,2,4),(-0.300005511286007,-0.206773466476134,-0.113541421666261,
-0.0567707108331306,-0.0283853554165654,0.),.UNSPECIFIED.);
#315=B_SPLINE_CURVE_WITH_KNOTS('',3,(#23300,#23301,#23302,#23303,#23304,
#23305,#23306,#23307,#23308,#23309,#23310,#23311,#23312,#23313),
 .UNSPECIFIED.,.F.,.F.,(4,2,2,2,2,2,4),(-0.242126305586689,-0.241475938992465,
-0.207325141862153,-0.17328250313445,-0.113202201999937,-0.0559588482258517,
0.),.UNSPECIFIED.);
#316=B_SPLINE_CURVE_WITH_KNOTS('',3,(#23315,#23316,#23317,#23318,#23319,
#23320,#23321,#23322,#23323,#23324,#23325,#23326,#23327,#23328),
 .UNSPECIFIED.,.F.,.F.,(4,2,2,2,2,2,4),(-0.237971793841113,-0.180365854109777,
-0.122215701674832,-0.0629296381239613,-0.0314884565302302,0.,0.000668991455295416),
 .UNSPECIFIED.);
#317=B_SPLINE_CURVE_WITH_KNOTS('',3,(#23339,#23340,#23341,#23342,#23343,
#23344,#23345,#23346,#23347,#23348,#23349,#23350,#23351,#23352),
 .UNSPECIFIED.,.F.,.F.,(4,2,2,2,2,2,4),(-0.23846990825455,-0.237798685175548,
-0.20633335283318,-0.174914932942728,-0.115672316276476,-0.0575645322663487,
0.),.UNSPECIFIED.);
#318=B_SPLINE_CURVE_WITH_KNOTS('',3,(#23356,#23357,#23358,#23359,#23360,
#23361,#23362,#23363,#23364,#23365,#23366,#23367,#23368,#23369),
 .UNSPECIFIED.,.F.,.F.,(4,2,2,2,2,2,4),(-0.241896356494029,-0.185842740394847,
-0.128518974500819,-0.0683631385924297,-0.0342301099048936,0.,0.000659700792702867),
 .UNSPECIFIED.);
#319=B_SPLINE_CURVE_WITH_KNOTS('',3,(#23388,#23389,#23390,#23391,#23392,
#23393,#23394,#23395,#23396,#23397),.UNSPECIFIED.,.F.,.F.,(4,2,2,2,4),(0.712943458944601,
0.733662141313163,0.754380823681726,0.827565491946693,1.09275712714737),
 .UNSPECIFIED.);
#320=B_SPLINE_CURVE_WITH_KNOTS('',3,(#23402,#23403,#23404,#23405,#23406,
#23407,#23408,#23409,#23410,#23411,#23412,#23413),.UNSPECIFIED.,.F.,.F.,
(4,2,2,2,2,4),(-0.300005511286008,-0.206773466476135,-0.113541421666261,
-0.0567707108331308,-0.0283853554165654,0.),.UNSPECIFIED.);
#321=B_SPLINE_CURVE_WITH_KNOTS('',3,(#23474,#23475,#23476,#23477,#23478,
#23479,#23480,#23481,#23482,#23483,#23484,#23485,#23486,#23487),
 .UNSPECIFIED.,.F.,.F.,(4,2,2,2,2,2,4),(-0.000578412997427686,0.,0.0341328715078763,
0.0680999028359124,0.128446519154858,0.185899361060066,0.241981137339067),
 .UNSPECIFIED.);
#322=B_SPLINE_CURVE_WITH_KNOTS('',3,(#23498,#23499,#23500,#23501,#23502,
#23503,#23504,#23505,#23506,#23507,#23508,#23509,#23510,#23511),
 .UNSPECIFIED.,.F.,.F.,(4,2,2,2,2,2,4),(0.,0.0559818727072018,0.113332368636633,
0.173571484036089,0.207478006800184,0.241550074317809,0.242127456935271),
 .UNSPECIFIED.);
#323=B_SPLINE_CURVE_WITH_KNOTS('',2,(#23531,#23532,#23533),
 .UNSPECIFIED.,.F.,.F.,(3,3),(0.,1.),.UNSPECIFIED.);
#324=B_SPLINE_CURVE_WITH_KNOTS('',2,(#23543,#23544,#23545),
 .UNSPECIFIED.,.F.,.F.,(3,3),(0.,1.),.UNSPECIFIED.);
#325=B_SPLINE_CURVE_WITH_KNOTS('',2,(#23554,#23555,#23556),
 .UNSPECIFIED.,.F.,.F.,(3,3),(0.,1.),.UNSPECIFIED.);
#326=B_SPLINE_CURVE_WITH_KNOTS('',2,(#23565,#23566,#23567),
 .UNSPECIFIED.,.F.,.F.,(3,3),(0.,1.),.UNSPECIFIED.);
#327=B_SPLINE_CURVE_WITH_KNOTS('',2,(#23576,#23577,#23578),
 .UNSPECIFIED.,.F.,.F.,(3,3),(0.,1.),.UNSPECIFIED.);
#328=B_SPLINE_CURVE_WITH_KNOTS('',2,(#23587,#23588,#23589),
 .UNSPECIFIED.,.F.,.F.,(3,3),(0.,1.),.UNSPECIFIED.);
#329=B_SPLINE_CURVE_WITH_KNOTS('',2,(#23598,#23599,#23600),
 .UNSPECIFIED.,.F.,.F.,(3,3),(0.,1.),.UNSPECIFIED.);
#330=B_SPLINE_CURVE_WITH_KNOTS('',2,(#23609,#23610,#23611),
 .UNSPECIFIED.,.F.,.F.,(3,3),(0.,1.),.UNSPECIFIED.);
#331=B_SPLINE_CURVE_WITH_KNOTS('',2,(#23620,#23621,#23622),
 .UNSPECIFIED.,.F.,.F.,(3,3),(0.,1.),.UNSPECIFIED.);
#332=B_SPLINE_CURVE_WITH_KNOTS('',2,(#23631,#23632,#23633),
 .UNSPECIFIED.,.F.,.F.,(3,3),(0.,1.),.UNSPECIFIED.);
#333=B_SPLINE_CURVE_WITH_KNOTS('',2,(#23640,#23641,#23642),
 .UNSPECIFIED.,.F.,.F.,(3,3),(0.,1.),.UNSPECIFIED.);
#334=B_SPLINE_CURVE_WITH_KNOTS('',2,(#23686,#23687,#23688),
 .UNSPECIFIED.,.F.,.F.,(3,3),(0.,1.),.UNSPECIFIED.);
#335=B_SPLINE_CURVE_WITH_KNOTS('',2,(#23698,#23699,#23700),
 .UNSPECIFIED.,.F.,.F.,(3,3),(0.,1.),.UNSPECIFIED.);
#336=B_SPLINE_CURVE_WITH_KNOTS('',2,(#23709,#23710,#23711),
 .UNSPECIFIED.,.F.,.F.,(3,3),(0.,1.),.UNSPECIFIED.);
#337=B_SPLINE_CURVE_WITH_KNOTS('',2,(#23720,#23721,#23722),
 .UNSPECIFIED.,.F.,.F.,(3,3),(0.,1.),.UNSPECIFIED.);
#338=B_SPLINE_CURVE_WITH_KNOTS('',2,(#23731,#23732,#23733),
 .UNSPECIFIED.,.F.,.F.,(3,3),(0.,1.),.UNSPECIFIED.);
#339=B_SPLINE_CURVE_WITH_KNOTS('',2,(#23742,#23743,#23744),
 .UNSPECIFIED.,.F.,.F.,(3,3),(0.,1.),.UNSPECIFIED.);
#340=B_SPLINE_CURVE_WITH_KNOTS('',2,(#23753,#23754,#23755),
 .UNSPECIFIED.,.F.,.F.,(3,3),(0.,1.),.UNSPECIFIED.);
#341=B_SPLINE_CURVE_WITH_KNOTS('',2,(#23764,#23765,#23766),
 .UNSPECIFIED.,.F.,.F.,(3,3),(0.,1.),.UNSPECIFIED.);
#342=B_SPLINE_CURVE_WITH_KNOTS('',2,(#23775,#23776,#23777),
 .UNSPECIFIED.,.F.,.F.,(3,3),(0.,1.),.UNSPECIFIED.);
#343=B_SPLINE_CURVE_WITH_KNOTS('',2,(#23786,#23787,#23788),
 .UNSPECIFIED.,.F.,.F.,(3,3),(0.,1.),.UNSPECIFIED.);
#344=B_SPLINE_CURVE_WITH_KNOTS('',2,(#23797,#23798,#23799),
 .UNSPECIFIED.,.F.,.F.,(3,3),(0.,1.),.UNSPECIFIED.);
#345=B_SPLINE_CURVE_WITH_KNOTS('',2,(#23808,#23809,#23810),
 .UNSPECIFIED.,.F.,.F.,(3,3),(0.,1.),.UNSPECIFIED.);
#346=B_SPLINE_CURVE_WITH_KNOTS('',2,(#23819,#23820,#23821),
 .UNSPECIFIED.,.F.,.F.,(3,3),(0.,1.),.UNSPECIFIED.);
#347=B_SPLINE_CURVE_WITH_KNOTS('',2,(#23830,#23831,#23832),
 .UNSPECIFIED.,.F.,.F.,(3,3),(0.,1.),.UNSPECIFIED.);
#348=B_SPLINE_CURVE_WITH_KNOTS('',2,(#23841,#23842,#23843),
 .UNSPECIFIED.,.F.,.F.,(3,3),(0.,1.),.UNSPECIFIED.);
#349=B_SPLINE_CURVE_WITH_KNOTS('',2,(#23850,#23851,#23852),
 .UNSPECIFIED.,.F.,.F.,(3,3),(0.,1.),.UNSPECIFIED.);
#350=B_SPLINE_CURVE_WITH_KNOTS('',3,(#23915,#23916,#23917,#23918,#23919,
#23920,#23921,#23922,#23923,#23924,#23925,#23926,#23927,#23928,#23929,#23930),
 .UNSPECIFIED.,.F.,.F.,(4,3,3,3,3,4),(-4.09299088010945,-3.98286471232789,
-3.4850066232869,-2.98714853424591,-2.48929044520493,-2.07752579179387),
 .UNSPECIFIED.);
#351=B_SPLINE_CURVE_WITH_KNOTS('',3,(#23933,#23934,#23935,#23936,#23937,
#23938,#23939,#23940,#23941,#23942),.UNSPECIFIED.,.F.,.F.,(4,3,3,4),(0.,
0.497858089040978,0.99571617808196,1.12612756527411),.UNSPECIFIED.);
#352=B_SPLINE_CURVE_WITH_KNOTS('',3,(#23947,#23948,#23949,#23950,#23951,
#23952,#23953,#23954,#23955,#23956,#23957,#23958,#23959,#23960,#23961,#23962,
#23963,#23964,#23965,#23966,#23967,#23968,#23969,#23970,#23971,#23972,#23973,
#23974,#23975,#23976,#23977,#23978,#23979,#23980,#23981,#23982,#23983,#23984,
#23985,#23986),.UNSPECIFIED.,.F.,.F.,(4,3,3,3,3,3,3,3,3,3,3,3,3,4),(-10.376176187289,
-9.95716178081971,-9.45930369177872,-8.96144560273774,-8.46358751369675,
-7.96572942465577,-7.46787133561478,-6.9700132465738,-6.47215515753281,
-5.97429706849183,-5.47643897945084,-4.97858089040986,-4.48072280136887,
-4.09299088010945),.UNSPECIFIED.);
#353=B_SPLINE_CURVE_WITH_KNOTS('',3,(#23987,#23988,#23989,#23990,#23991,
#23992,#23993,#23994,#23995,#23996,#23997,#23998,#23999,#24000,#24001,#24002,
#24003,#24004,#24005,#24006,#24007,#24008,#24009,#24010,#24011,#24012,#24013,
#24014,#24015,#24016,#24017,#24018,#24019,#24020,#24021,#24022,#24023,#24024,
#24025,#24026),.UNSPECIFIED.,.F.,.F.,(4,3,3,3,3,3,3,3,3,3,3,3,3,4),(1.12612756527411,
1.49357426712295,1.99143235616393,2.48929044520492,2.98714853424591,3.48500662328689,
3.98286471232788,4.48072280136887,4.97858089040986,5.47643897945084,5.97429706849183,
6.47215515753282,6.9700132465738,7.40931287245371),.UNSPECIFIED.);
#354=B_SPLINE_CURVE_WITH_KNOTS('',3,(#24031,#24032,#24033,#24034,#24035,
#24036,#24037,#24038,#24039,#24040,#24041,#24042,#24043,#24044,#24045,#24046,
#24047,#24048,#24049,#24050,#24051,#24052,#24053,#24054,#24055,#24056,#24057,
#24058,#24059,#24060,#24061,#24062,#24063,#24064,#24065,#24066,#24067,#24068,
#24069,#24070,#24071,#24072,#24073),.UNSPECIFIED.,.F.,.F.,(4,3,3,3,3,3,
3,3,3,3,3,3,3,3,4),(-16.6593614944686,-16.4293169383525,-15.9314588493115,
-15.4336007602705,-14.9357426712296,-14.4378845821886,-13.9400264931476,
-13.4421684041066,-12.9443103150656,-12.4464522260246,-11.9485941369836,
-11.4507360479427,-10.9528779589017,-10.4550198698607,-10.376176187289),
 .UNSPECIFIED.);
#355=B_SPLINE_CURVE_WITH_KNOTS('',3,(#24074,#24075,#24076,#24077,#24078,
#24079,#24080,#24081,#24082,#24083,#24084,#24085,#24086,#24087,#24088,#24089,
#24090,#24091,#24092,#24093,#24094,#24095,#24096,#24097,#24098,#24099,#24100,
#24101,#24102,#24103,#24104,#24105,#24106,#24107,#24108,#24109,#24110,#24111,
#24112,#24113,#24114,#24115,#24116),.UNSPECIFIED.,.F.,.F.,(4,3,3,3,3,3,
3,3,3,3,3,3,3,3,4),(7.40931287245371,7.46787133561479,7.96572942465578,
8.46358751369676,8.96144560273774,9.45930369177873,9.95716178081971,10.4550198698607,
10.9528779589017,11.4507360479427,11.9485941369836,12.4464522260246,12.9443103150656,
13.4421684041066,13.6924981796333),.UNSPECIFIED.);
#356=B_SPLINE_CURVE_WITH_KNOTS('',3,(#24121,#24122,#24123,#24124,#24125,
#24126,#24127,#24128,#24129,#24130,#24131,#24132,#24133,#24134,#24135,#24136,
#24137,#24138,#24139,#24140,#24141,#24142,#24143,#24144,#24145,#24146,#24147,
#24148,#24149,#24150,#24151,#24152,#24153,#24154,#24155,#24156,#24157,#24158,
#24159,#24160,#24161,#24162,#24163),.UNSPECIFIED.,.F.,.F.,(4,3,3,3,3,3,
3,3,3,3,3,3,3,3,4),(-22.9425468016482,-22.9014720958853,-22.4036140068443,
-21.9057559178034,-21.4078978287624,-20.9100397397214,-20.4121816506804,
-19.9143235616394,-19.4164654725984,-18.9186073835574,-18.4207492945165,
-17.9228912054755,-17.4250331164345,-16.9271750273935,-16.6593614944686),
 .UNSPECIFIED.);
#357=B_SPLINE_CURVE_WITH_KNOTS('',3,(#24164,#24165,#24166,#24167,#24168,
#24169,#24170,#24171,#24172,#24173,#24174,#24175,#24176,#24177,#24178,#24179,
#24180,#24181,#24182,#24183,#24184,#24185,#24186,#24187,#24188,#24189,#24190,
#24191,#24192,#24193,#24194,#24195,#24196,#24197,#24198,#24199,#24200,#24201,
#24202,#24203,#24204,#24205,#24206),.UNSPECIFIED.,.F.,.F.,(4,3,3,3,3,3,
3,3,3,3,3,3,3,3,4),(13.6924981796333,13.9400264931476,14.4378845821886,
14.9357426712296,15.4336007602705,15.9314588493115,16.4293169383525,16.9271750273935,
17.4250331164345,17.9228912054755,18.4207492945165,18.9186073835575,19.4164654725984,
19.9143235616394,19.9756834868129),.UNSPECIFIED.);
#358=B_SPLINE_CURVE_WITH_KNOTS('',3,(#24211,#24212,#24213,#24214,#24215,
#24216,#24217,#24218,#24219,#24220,#24221,#24222,#24223,#24224,#24225,#24226,
#24227,#24228,#24229,#24230,#24231,#24232,#24233,#24234,#24235,#24236,#24237,
#24238,#24239,#24240,#24241,#24242,#24243,#24244,#24245,#24246,#24247,#24248,
#24249,#24250),.UNSPECIFIED.,.F.,.F.,(4,3,3,3,3,3,3,3,3,3,3,3,3,4),(-29.2257321088278,
-28.8757691643771,-28.3779110753362,-27.8800529862952,-27.3821948972542,
-26.8843368082132,-26.3864787191722,-25.8886206301312,-25.3907625410903,
-24.8929044520493,-24.3950463630083,-23.8971882739673,-23.3993301849263,
-22.9425468016482),.UNSPECIFIED.);
#359=B_SPLINE_CURVE_WITH_KNOTS('',3,(#24251,#24252,#24253,#24254,#24255,
#24256,#24257,#24258,#24259,#24260,#24261,#24262,#24263,#24264,#24265,#24266,
#24267,#24268,#24269,#24270,#24271,#24272,#24273,#24274,#24275,#24276,#24277,
#24278,#24279,#24280,#24281,#24282,#24283,#24284,#24285,#24286,#24287,#24288,
#24289,#24290),.UNSPECIFIED.,.F.,.F.,(4,3,3,3,3,3,3,3,3,3,3,3,3,4),(19.9756834868129,
20.4121816506804,20.9100397397214,21.4078978287624,21.9057559178034,22.4036140068443,
22.9014720958853,23.3993301849263,23.8971882739673,24.3950463630083,24.8929044520493,
25.3907625410903,25.8886206301312,26.2588687939925),.UNSPECIFIED.);
#360=B_SPLINE_CURVE_WITH_KNOTS('',3,(#24295,#24296,#24297,#24298,#24299,
#24300,#24301,#24302,#24303,#24304,#24305,#24306,#24307,#24308,#24309,#24310,
#24311,#24312,#24313,#24314,#24315,#24316,#24317,#24318,#24319,#24320,#24321,
#24322,#24323,#24324,#24325,#24326,#24327,#24328,#24329,#24330,#24331,#24332,
#24333,#24334,#24335,#24336,#24337),.UNSPECIFIED.,.F.,.F.,(4,3,3,3,3,3,
3,3,3,3,3,3,3,3,4),(-35.5089174160074,-35.34792432191,-34.850066232869,
-34.352208143828,-33.854350054787,-33.356491965746,-32.858633876705,-32.3607757876641,
-31.8629176986231,-31.3650596095821,-30.8672015205411,-30.3693434315001,
-29.8714853424591,-29.3736272534181,-29.2257321088278),.UNSPECIFIED.);
#361=B_SPLINE_CURVE_WITH_KNOTS('',3,(#24338,#24339,#24340,#24341,#24342,
#24343,#24344,#24345,#24346,#24347,#24348,#24349,#24350,#24351,#24352,#24353,
#24354,#24355,#24356,#24357,#24358,#24359,#24360,#24361,#24362,#24363,#24364,
#24365,#24366,#24367,#24368,#24369,#24370,#24371,#24372,#24373,#24374,#24375,
#24376,#24377,#24378,#24379,#24380),.UNSPECIFIED.,.F.,.F.,(4,3,3,3,3,3,
3,3,3,3,3,3,3,3,4),(26.2588687939925,26.3864787191722,26.8843368082132,
27.3821948972542,27.8800529862952,28.3779110753362,28.8757691643771,29.3736272534181,
29.8714853424591,30.3693434315001,30.8672015205411,31.3650596095821,31.8629176986231,
32.3607757876641,32.542054101172),.UNSPECIFIED.);
#362=B_SPLINE_CURVE_WITH_KNOTS('',3,(#24385,#24386,#24387,#24388,#24389,
#24390,#24391,#24392,#24393,#24394,#24395,#24396,#24397,#24398,#24399,#24400,
#24401,#24402,#24403,#24404,#24405,#24406,#24407,#24408,#24409,#24410,#24411,
#24412,#24413,#24414,#24415,#24416,#24417,#24418,#24419,#24420,#24421,#24422,
#24423,#24424),.UNSPECIFIED.,.F.,.F.,(4,3,3,3,3,3,3,3,3,3,3,3,3,4),(-41.792102723187,
-41.3222213904018,-40.8243633013608,-40.3265052123198,-39.8286471232788,
-39.3307890342378,-38.8329309451969,-38.3350728561559,-37.8372147671149,
-37.3393566780739,-36.8414985890329,-36.3436404999919,-35.8457824109509,
-35.5089174160074),.UNSPECIFIED.);
#363=B_SPLINE_CURVE_WITH_KNOTS('',3,(#24425,#24426,#24427,#24428,#24429,
#24430,#24431,#24432,#24433,#24434,#24435,#24436,#24437,#24438,#24439,#24440,
#24441,#24442,#24443,#24444,#24445,#24446,#24447,#24448,#24449,#24450,#24451,
#24452,#24453,#24454,#24455,#24456,#24457,#24458,#24459,#24460,#24461,#24462,
#24463,#24464),.UNSPECIFIED.,.F.,.F.,(4,3,3,3,3,3,3,3,3,3,3,3,3,4),(32.542054101172,
32.858633876705,33.356491965746,33.854350054787,34.352208143828,34.850066232869,
35.34792432191,35.845782410951,36.3436404999919,36.8414985890329,37.3393566780739,
37.8372147671149,38.3350728561559,38.8252394083516),.UNSPECIFIED.);
#364=B_SPLINE_CURVE_WITH_KNOTS('',3,(#24469,#24470,#24471,#24472,#24473,
#24474,#24475,#24476,#24477,#24478,#24479,#24480,#24481,#24482,#24483,#24484,
#24485,#24486,#24487,#24488,#24489,#24490,#24491,#24492,#24493,#24494,#24495,
#24496,#24497,#24498,#24499,#24500,#24501,#24502,#24503,#24504,#24505,#24506,
#24507,#24508,#24509,#24510,#24511),.UNSPECIFIED.,.F.,.F.,(4,3,3,3,3,3,
3,3,3,3,3,3,3,3,4),(-48.0752880303665,-47.7943765479346,-47.2965184588936,
-46.7986603698526,-46.3008022808116,-45.8029441917706,-45.3050861027297,
-44.8072280136887,-44.3093699246477,-43.8115118356067,-43.3136537465657,
-42.8157956575247,-42.3179375684838,-41.8200794794428,-41.792102723187),
 .UNSPECIFIED.);
#365=B_SPLINE_CURVE_WITH_KNOTS('',3,(#24512,#24513,#24514,#24515,#24516,
#24517,#24518,#24519,#24520,#24521,#24522,#24523,#24524,#24525,#24526,#24527,
#24528,#24529,#24530,#24531,#24532,#24533,#24534,#24535,#24536,#24537,#24538,
#24539,#24540,#24541,#24542,#24543,#24544,#24545,#24546,#24547,#24548,#24549,
#24550,#24551,#24552,#24553,#24554),.UNSPECIFIED.,.F.,.F.,(4,3,3,3,3,3,
3,3,3,3,3,3,3,3,4),(38.8252394083516,38.8329309451969,39.3307890342379,
39.8286471232788,40.3265052123198,40.8243633013608,41.3222213904018,41.8200794794428,
42.3179375684838,42.8157956575247,43.3136537465657,43.8115118356067,44.3093699246477,
44.8072280136887,45.1084247155312),.UNSPECIFIED.);
#366=B_SPLINE_CURVE_WITH_KNOTS('',3,(#24559,#24560,#24561,#24562,#24563,
#24564,#24565,#24566,#24567,#24568,#24569,#24570,#24571,#24572,#24573,#24574,
#24575,#24576,#24577,#24578,#24579,#24580,#24581,#24582,#24583,#24584,#24585,
#24586,#24587,#24588,#24589,#24590,#24591,#24592,#24593,#24594,#24595,#24596,
#24597,#24598,#24599,#24600,#24601),.UNSPECIFIED.,.F.,.F.,(4,3,3,3,3,3,
3,3,3,3,3,3,3,3,4),(-54.3584733375462,-54.2665317054674,-53.7686736164264,
-53.2708155273854,-52.7729574383444,-52.2750993493035,-51.7772412602625,
-51.2793831712215,-50.7815250821805,-50.2836669931395,-49.7858089040985,
-49.2879508150576,-48.7900927260166,-48.2922346369756,-48.0752880303665),
 .UNSPECIFIED.);
#367=B_SPLINE_CURVE_WITH_KNOTS('',3,(#24602,#24603,#24604,#24605,#24606,
#24607,#24608,#24609,#24610,#24611,#24612,#24613,#24614,#24615,#24616,#24617,
#24618,#24619,#24620,#24621,#24622,#24623,#24624,#24625,#24626,#24627,#24628,
#24629,#24630,#24631,#24632,#24633,#24634,#24635,#24636,#24637,#24638,#24639,
#24640,#24641,#24642,#24643,#24644),.UNSPECIFIED.,.F.,.F.,(4,3,3,3,3,3,
3,3,3,3,3,3,3,3,4),(45.1084247155312,45.3050861027297,45.8029441917707,
46.3008022808116,46.7986603698526,47.2965184588936,47.7943765479346,48.2922346369756,
48.7900927260166,49.2879508150575,49.7858089040985,50.2836669931395,50.7815250821805,
51.2793831712215,51.3916100227108),.UNSPECIFIED.);
#368=B_SPLINE_CURVE_WITH_KNOTS('',3,(#24649,#24650,#24651,#24652,#24653,
#24654,#24655,#24656,#24657,#24658,#24659,#24660,#24661,#24662,#24663,#24664,
#24665,#24666,#24667,#24668,#24669,#24670,#24671,#24672,#24673,#24674,#24675,
#24676,#24677,#24678,#24679,#24680,#24681,#24682,#24683,#24684,#24685,#24686,
#24687,#24688),.UNSPECIFIED.,.F.,.F.,(4,3,3,3,3,3,3,3,3,3,3,3,3,4),(-60.6416586447257,
-60.2408287739593,-59.7429706849182,-59.2451125958773,-58.7472545068363,
-58.2493964177953,-57.7515383287543,-57.2536802397133,-56.7558221506723,
-56.2579640616314,-55.7601059725904,-55.2622478835494,-54.7643897945084,
-54.3584733375462),.UNSPECIFIED.);
#369=B_SPLINE_CURVE_WITH_KNOTS('',3,(#24689,#24690,#24691,#24692,#24693,
#24694,#24695,#24696,#24697,#24698,#24699,#24700,#24701,#24702,#24703,#24704,
#24705,#24706,#24707,#24708,#24709,#24710,#24711,#24712,#24713,#24714,#24715,
#24716,#24717,#24718,#24719,#24720,#24721,#24722,#24723,#24724,#24725,#24726,
#24727,#24728),.UNSPECIFIED.,.F.,.F.,(4,3,3,3,3,3,3,3,3,3,3,3,3,4),(51.3916100227108,
51.7772412602625,52.2750993493035,52.7729574383445,53.2708155273854,53.7686736164264,
54.2665317054674,54.7643897945084,55.2622478835494,55.7601059725904,56.2579640616314,
56.7558221506723,57.2536802397133,57.6747953298904),.UNSPECIFIED.);
#370=B_SPLINE_CURVE_WITH_KNOTS('',3,(#24733,#24734,#24735,#24736,#24737,
#24738,#24739,#24740,#24741,#24742,#24743,#24744,#24745,#24746,#24747,#24748,
#24749,#24750,#24751,#24752,#24753,#24754,#24755,#24756,#24757,#24758,#24759,
#24760,#24761,#24762,#24763,#24764,#24765,#24766,#24767,#24768,#24769,#24770,
#24771,#24772,#24773,#24774,#24775),.UNSPECIFIED.,.F.,.F.,(4,3,3,3,3,3,
3,3,3,3,3,3,3,3,4),(-66.9248439519053,-66.712983931492,-66.215125842451,
-65.7172677534101,-65.2194096643691,-64.7215515753281,-64.2236934862871,
-63.7258353972461,-63.2279773082051,-62.7301192191642,-62.2322611301232,
-61.7344030410822,-61.2365449520412,-60.7386868630002,-60.6416586447257),
 .UNSPECIFIED.);
#371=B_SPLINE_CURVE_WITH_KNOTS('',3,(#24776,#24777,#24778,#24779,#24780,
#24781,#24782,#24783,#24784,#24785,#24786,#24787,#24788,#24789,#24790,#24791,
#24792,#24793,#24794,#24795,#24796,#24797,#24798,#24799,#24800,#24801,#24802,
#24803,#24804,#24805,#24806,#24807,#24808,#24809,#24810,#24811,#24812,#24813,
#24814,#24815,#24816,#24817,#24818),.UNSPECIFIED.,.F.,.F.,(4,3,3,3,3,3,
3,3,3,3,3,3,3,3,4),(57.6747953298904,57.7515383287543,58.2493964177953,
58.7472545068363,59.2451125958773,59.7429706849182,60.2408287739592,60.7386868630002,
61.2365449520412,61.7344030410822,62.2322611301232,62.7301192191642,63.2279773082051,
63.7258353972461,63.95798063707),.UNSPECIFIED.);
#372=B_SPLINE_CURVE_WITH_KNOTS('',3,(#24823,#24824,#24825,#24826,#24827,
#24828,#24829,#24830,#24831,#24832,#24833,#24834,#24835,#24836,#24837,#24838,
#24839,#24840,#24841,#24842,#24843,#24844,#24845,#24846,#24847,#24848,#24849,
#24850,#24851,#24852,#24853,#24854,#24855,#24856,#24857,#24858,#24859,#24860,
#24861,#24862,#24863,#24864,#24865),.UNSPECIFIED.,.F.,.F.,(4,3,3,3,3,3,
3,3,3,3,3,3,3,3,4),(-73.2080292590849,-73.1851390890248,-72.6872809999838,
-72.1894229109429,-71.6915648219019,-71.1937067328609,-70.6958486438199,
-70.1979905547789,-69.7001324657379,-69.202274376697,-68.704416287656,-68.206558198615,
-67.708700109574,-67.210842020533,-66.9248439519053),.UNSPECIFIED.);
#373=B_SPLINE_CURVE_WITH_KNOTS('',3,(#24866,#24867,#24868,#24869,#24870,
#24871,#24872,#24873,#24874,#24875,#24876,#24877,#24878,#24879,#24880,#24881,
#24882,#24883,#24884,#24885,#24886,#24887,#24888,#24889,#24890,#24891,#24892,
#24893,#24894,#24895,#24896,#24897,#24898,#24899,#24900,#24901,#24902,#24903,
#24904,#24905,#24906,#24907,#24908),.UNSPECIFIED.,.F.,.F.,(4,3,3,3,3,3,
3,3,3,3,3,3,3,3,4),(63.95798063707,64.2236934862871,64.7215515753281,65.2194096643691,
65.7172677534101,66.2151258424511,66.712983931492,67.210842020533,67.708700109574,
68.206558198615,68.704416287656,69.202274376697,69.700132465738,70.1979905547789,
70.2411659442496),.UNSPECIFIED.);
#374=B_SPLINE_CURVE_WITH_KNOTS('',3,(#24913,#24914,#24915,#24916,#24917,
#24918,#24919,#24920,#24921,#24922,#24923,#24924,#24925,#24926,#24927,#24928,
#24929,#24930,#24931,#24932,#24933,#24934,#24935,#24936,#24937,#24938,#24939,
#24940,#24941,#24942,#24943,#24944,#24945,#24946,#24947,#24948,#24949,#24950,
#24951,#24952),.UNSPECIFIED.,.F.,.F.,(4,3,3,3,3,3,3,3,3,3,3,3,3,4),(-79.4912145662645,
-79.1594361575167,-78.6615780684757,-78.1637199794347,-77.6658618903937,
-77.1680038013527,-76.6701457123117,-76.1722876232708,-75.6744295342298,
-75.1765714451888,-74.6787133561478,-74.1808552671068,-73.6829971780658,
-73.2080292590849),.UNSPECIFIED.);
#375=B_SPLINE_CURVE_WITH_KNOTS('',3,(#24953,#24954,#24955,#24956,#24957,
#24958,#24959,#24960,#24961,#24962,#24963,#24964,#24965,#24966,#24967,#24968,
#24969,#24970,#24971,#24972,#24973,#24974,#24975,#24976,#24977,#24978,#24979,
#24980,#24981,#24982,#24983,#24984,#24985,#24986,#24987,#24988,#24989,#24990,
#24991,#24992),.UNSPECIFIED.,.F.,.F.,(4,3,3,3,3,3,3,3,3,3,3,3,3,4),(70.2411659442496,
70.6958486438199,71.1937067328609,71.6915648219019,72.1894229109429,72.6872809999839,
73.1851390890248,73.6829971780658,74.1808552671068,74.6787133561478,75.1765714451888,
75.6744295342298,76.1722876232707,76.5243512514292),.UNSPECIFIED.);
#376=B_SPLINE_CURVE_WITH_KNOTS('',3,(#24997,#24998,#24999,#25000,#25001,
#25002,#25003,#25004,#25005,#25006,#25007,#25008,#25009,#25010,#25011,#25012,
#25013,#25014,#25015,#25016,#25017,#25018,#25019,#25020,#25021,#25022,#25023,
#25024,#25025,#25026,#25027,#25028,#25029,#25030,#25031,#25032,#25033,#25034,
#25035,#25036,#25037,#25038,#25039),.UNSPECIFIED.,.F.,.F.,(4,3,3,3,3,3,
3,3,3,3,3,3,3,3,4),(-85.7743998734441,-85.6315913150495,-85.1337332260085,
-84.6358751369675,-84.1380170479265,-83.6401589588856,-83.1423008698446,
-82.6444427808036,-82.1465846917626,-81.6487266027216,-81.1508685136806,
-80.6530104246396,-80.1551523355986,-79.6572942465577,-79.4912145662645),
 .UNSPECIFIED.);
#377=B_SPLINE_CURVE_WITH_KNOTS('',3,(#25040,#25041,#25042,#25043,#25044,
#25045,#25046,#25047,#25048,#25049,#25050,#25051,#25052,#25053,#25054,#25055,
#25056,#25057,#25058,#25059,#25060,#25061,#25062,#25063,#25064,#25065,#25066,
#25067,#25068,#25069,#25070,#25071,#25072,#25073,#25074,#25075,#25076,#25077,
#25078,#25079,#25080,#25081,#25082),.UNSPECIFIED.,.F.,.F.,(4,3,3,3,3,3,
3,3,3,3,3,3,3,3,4),(76.5243512514292,76.6701457123117,77.1680038013527,
77.6658618903937,78.1637199794347,78.6615780684757,79.1594361575167,79.6572942465577,
80.1551523355986,80.6530104246396,81.1508685136806,81.6487266027216,82.1465846917626,
82.6444427808036,82.8075365586088),.UNSPECIFIED.);
#378=B_SPLINE_CURVE_WITH_KNOTS('',3,(#25087,#25088,#25089,#25090,#25091,
#25092,#25093,#25094,#25095,#25096,#25097,#25098,#25099,#25100,#25101,#25102,
#25103,#25104,#25105,#25106,#25107,#25108,#25109,#25110,#25111,#25112,#25113,
#25114,#25115,#25116,#25117,#25118,#25119,#25120,#25121,#25122,#25123,#25124,
#25125,#25126),.UNSPECIFIED.,.F.,.F.,(4,3,3,3,3,3,3,3,3,3,3,3,3,4),(-92.0575851806237,
-91.6058883835413,-91.1080302945003,-90.6101722054593,-90.1123141164184,
-89.6144560273774,-89.1165979383364,-88.6187398492954,-88.1208817602544,
-87.6230236712134,-87.1251655821724,-86.6273074931315,-86.1294494040905,
-85.7743998734441),.UNSPECIFIED.);
#379=B_SPLINE_CURVE_WITH_KNOTS('',3,(#25127,#25128,#25129,#25130,#25131,
#25132,#25133,#25134,#25135,#25136,#25137,#25138,#25139,#25140,#25141,#25142,
#25143,#25144,#25145,#25146,#25147,#25148,#25149,#25150,#25151,#25152,#25153,
#25154,#25155,#25156,#25157,#25158,#25159,#25160,#25161,#25162,#25163,#25164,
#25165,#25166),.UNSPECIFIED.,.F.,.F.,(4,3,3,3,3,3,3,3,3,3,3,3,3,4),(82.8075365586088,
83.1423008698446,83.6401589588855,84.1380170479265,84.6358751369675,85.1337332260085,
85.6315913150495,86.1294494040905,86.6273074931315,87.1251655821725,87.6230236712134,
88.1208817602544,88.6187398492954,89.0907218657884),.UNSPECIFIED.);
#380=B_SPLINE_CURVE_WITH_KNOTS('',3,(#25171,#25172,#25173,#25174,#25175,
#25176,#25177,#25178,#25179,#25180,#25181,#25182,#25183,#25184,#25185,#25186,
#25187,#25188,#25189,#25190,#25191,#25192,#25193,#25194,#25195,#25196,#25197,
#25198,#25199,#25200,#25201,#25202,#25203,#25204,#25205,#25206,#25207,#25208,
#25209,#25210,#25211,#25212,#25213),.UNSPECIFIED.,.F.,.F.,(4,3,3,3,3,3,
3,3,3,3,3,3,3,3,4),(-98.3407704878033,-98.0780435410741,-97.5801854520331,
-97.0823273629921,-96.5844692739512,-96.0866111849102,-95.5887530958692,
-95.0908950068282,-94.5930369177872,-94.0951788287462,-93.5973207397052,
-93.0994626506643,-92.6016045616233,-92.1037464725823,-92.0575851806237),
 .UNSPECIFIED.);
#381=B_SPLINE_CURVE_WITH_KNOTS('',3,(#25214,#25215,#25216,#25217,#25218,
#25219,#25220,#25221,#25222,#25223,#25224,#25225,#25226,#25227,#25228,#25229,
#25230,#25231,#25232,#25233,#25234,#25235,#25236,#25237,#25238,#25239,#25240,
#25241,#25242,#25243,#25244,#25245,#25246,#25247,#25248,#25249,#25250,#25251,
#25252,#25253,#25254,#25255,#25256),.UNSPECIFIED.,.F.,.F.,(4,3,3,3,3,3,
3,3,3,3,3,3,3,3,4),(89.0907218657884,89.1165979383364,89.6144560273774,
90.1123141164184,90.6101722054593,91.1080302945003,91.6058883835413,92.1037464725823,
92.6016045616233,93.0994626506643,93.5973207397052,94.0951788287462,94.5930369177872,
95.0908950068282,95.373907172968),.UNSPECIFIED.);
#382=B_SPLINE_CURVE_WITH_KNOTS('',3,(#25262,#25263,#25264,#25265,#25266,
#25267,#25268,#25269,#25270,#25271,#25272,#25273,#25274,#25275,#25276),
 .UNSPECIFIED.,.F.,.F.,(4,1,1,1,1,1,1,1,1,1,1,1,4),(103.672557568463,103.718718860422,
104.216576949463,104.714435038504,105.212293127545,105.710151216586,106.208009305627,
106.705867394668,107.203725483709,107.70158357275,108.199441661791,108.697299750832,
109.109064404243),.UNSPECIFIED.);
#383=B_SPLINE_CURVE_WITH_KNOTS('',3,(#25279,#25280,#25281,#25282,#25283,
#25284,#25285,#25286,#25287,#25288,#25289,#25290),.UNSPECIFIED.,.F.,.F.,
(4,1,1,1,1,1,1,1,1,4),(103.672557568463,103.887403491364,104.385261580405,
104.883119669446,105.380977758487,105.878835847528,106.376693936569,106.87455202561,
107.372410114651,107.870268203692),.UNSPECIFIED.);
#384=B_SPLINE_CURVE_WITH_KNOTS('',3,(#25295,#25296,#25297,#25298,#25299,
#25300,#25301,#25302,#25303,#25304,#25305,#25306,#25307,#25308,#25309,#25310),
 .UNSPECIFIED.,.F.,.F.,(4,1,1,1,1,1,1,1,1,1,1,1,1,4),(97.3893722612836,
97.7444217919299,98.2422798809709,98.7401379700119,99.2379960590529,99.7358541480939,
100.233712237135,100.731570326176,101.229428415217,101.727286504258,102.225144593299,
102.72300268234,103.220860771381,103.672557568463),.UNSPECIFIED.);
#385=B_SPLINE_CURVE_WITH_KNOTS('',3,(#25311,#25312,#25313,#25314,#25315,
#25316,#25317,#25318,#25319,#25320,#25321,#25322,#25323,#25324,#25325,#25326,
#25327),.UNSPECIFIED.,.F.,.F.,(4,1,1,1,1,1,1,1,1,1,1,1,1,1,4),(97.3893722612836,
97.4152483338315,97.9131064228725,98.4109645119134,98.9088226009544,99.4066806899954,
99.9045387790364,100.402396868077,100.900254957118,101.398113046159,101.8959711352,
102.393829224241,102.891687313282,103.389545402323,103.672557568463),
 .UNSPECIFIED.);
#386=B_SPLINE_CURVE_WITH_KNOTS('',3,(#25332,#25333,#25334,#25335,#25336,
#25337,#25338,#25339,#25340,#25341,#25342,#25343,#25344,#25345,#25346,#25347,
#25348),.UNSPECIFIED.,.F.,.F.,(4,1,1,1,1,1,1,1,1,1,1,1,1,1,4),(91.106186954104,
91.2722666343971,91.7701247234381,92.2679828124791,92.7658409015201,93.2636989905611,
93.761557079602,94.259415168643,94.757273257684,95.255131346725,95.752989435766,
96.250847524807,96.7487056138479,97.2465637028889,97.3893722612836),
 .UNSPECIFIED.);
#387=B_SPLINE_CURVE_WITH_KNOTS('',3,(#25349,#25350,#25351,#25352,#25353,
#25354,#25355,#25356,#25357,#25358,#25359,#25360,#25361,#25362,#25363,#25364),
 .UNSPECIFIED.,.F.,.F.,(4,1,1,1,1,1,1,1,1,1,1,1,1,4),(91.106186954104,91.4409512653396,
91.9388093543806,92.4366674434216,92.9345255324626,93.4323836215036,93.9302417105446,
94.4280997995856,94.9259578886266,95.4238159776675,95.9216740667085,96.4195321557495,
96.9173902447905,97.3893722612836),.UNSPECIFIED.);
#388=B_SPLINE_CURVE_WITH_KNOTS('',3,(#25369,#25370,#25371,#25372,#25373,
#25374,#25375,#25376,#25377,#25378,#25379,#25380,#25381,#25382,#25383,#25384),
 .UNSPECIFIED.,.F.,.F.,(4,1,1,1,1,1,1,1,1,1,1,1,1,4),(84.8230016469244,
85.2979695659053,85.7958276549463,86.2936857439873,86.7915438330282,87.2894019220692,
87.7872600111102,88.2851181001512,88.7829761891922,89.2808342782332,89.7786923672741,
90.2765504563151,90.7744085453561,91.106186954104),.UNSPECIFIED.);
#389=B_SPLINE_CURVE_WITH_KNOTS('',3,(#25385,#25386,#25387,#25388,#25389,
#25390,#25391,#25392,#25393,#25394,#25395,#25396,#25397,#25398,#25399,#25400,
#25401),.UNSPECIFIED.,.F.,.F.,(4,1,1,1,1,1,1,1,1,1,1,1,1,1,4),(84.8230016469244,
84.9687961078068,85.4666541968478,85.9645122858888,86.4623703749298,86.9602284639708,
87.4580865530118,87.9559446420528,88.4538027310937,88.9516608201347,89.4495189091757,
89.9473769982167,90.4452350872577,90.9430931762987,91.106186954104),
 .UNSPECIFIED.);
#390=B_SPLINE_CURVE_WITH_KNOTS('',3,(#25406,#25407,#25408,#25409,#25410,
#25411,#25412,#25413,#25414,#25415,#25416,#25417,#25418,#25419,#25420,#25421,
#25422),.UNSPECIFIED.,.F.,.F.,(4,1,1,1,1,1,1,1,1,1,1,1,1,1,4),(78.5398163397448,
78.8258144083725,79.3236724974135,79.8215305864545,80.3193886754954,80.8172467645364,
81.3151048535774,81.8129629426184,82.3108210316594,82.8086791207004,83.3065372097414,
83.8043952987823,84.3022533878233,84.8001114768643,84.8230016469244),
 .UNSPECIFIED.);
#391=B_SPLINE_CURVE_WITH_KNOTS('',3,(#25423,#25424,#25425,#25426,#25427,
#25428,#25429,#25430,#25431,#25432,#25433,#25434,#25435,#25436,#25437,#25438),
 .UNSPECIFIED.,.F.,.F.,(4,1,1,1,1,1,1,1,1,1,1,1,1,4),(78.5398163397448,
78.994499039315,79.492357128356,79.990215217397,80.488073306438,80.985931395479,
81.4837894845199,81.9816475735609,82.4795056626019,82.9773637516429,83.4752218406839,
83.9730799297249,84.4709380187658,84.8230016469244),.UNSPECIFIED.);
#392=B_SPLINE_CURVE_WITH_KNOTS('',3,(#25443,#25444,#25445,#25446,#25447,
#25448,#25449,#25450,#25451,#25452,#25453,#25454,#25455,#25456,#25457,#25458,
#25459),.UNSPECIFIED.,.F.,.F.,(4,1,1,1,1,1,1,1,1,1,1,1,1,1,4),(72.2566310325652,
72.3536592508397,72.8515173398807,73.3493754289216,73.8472335179626,74.3450916070036,
74.8429496960446,75.3408077850856,75.8386658741266,76.3365239631676,76.8343820522085,
77.3322401412495,77.8300982302905,78.3279563193315,78.5398163397448),
 .UNSPECIFIED.);
#393=B_SPLINE_CURVE_WITH_KNOTS('',3,(#25460,#25461,#25462,#25463,#25464,
#25465,#25466,#25467,#25468,#25469,#25470,#25471,#25472,#25473,#25474,#25475,
#25476),.UNSPECIFIED.,.F.,.F.,(4,1,1,1,1,1,1,1,1,1,1,1,1,1,4),(72.2566310325652,
72.5223438817822,73.0202019708232,73.5180600598642,74.0159181489052,74.5137762379462,
75.0116343269871,75.5094924160281,76.0073505050691,76.5052085941101,77.0030666831511,
77.5009247721921,77.9987828612331,78.496640950274,78.5398163397448),
 .UNSPECIFIED.);
#394=B_SPLINE_CURVE_WITH_KNOTS('',3,(#25481,#25482,#25483,#25484,#25485,
#25486,#25487,#25488,#25489,#25490,#25491,#25492,#25493,#25494,#25495,#25496),
 .UNSPECIFIED.,.F.,.F.,(4,1,1,1,1,1,1,1,1,1,1,1,1,4),(65.9734457253856,
66.3793621823478,66.8772202713888,67.3750783604298,67.8729364494708,68.3707945385118,
68.8686526275528,69.3665107165938,69.8643688056347,70.3622268946757,70.8600849837167,
71.3579430727577,71.8558011617987,72.2566310325652),.UNSPECIFIED.);
#395=B_SPLINE_CURVE_WITH_KNOTS('',3,(#25497,#25498,#25499,#25500,#25501,
#25502,#25503,#25504,#25505,#25506,#25507,#25508,#25509,#25510,#25511,#25512,
#25513),.UNSPECIFIED.,.F.,.F.,(4,1,1,1,1,1,1,1,1,1,1,1,1,1,4),(65.9734457253856,
66.0501887242494,66.5480468132904,67.0459049023314,67.5437629913723,68.0416210804133,
68.5394791694543,69.0373372584953,69.5351953475363,70.0330534365773,70.5309115256183,
71.0287696146593,71.5266277037002,72.0244857927412,72.2566310325652),
 .UNSPECIFIED.);
#396=B_SPLINE_CURVE_WITH_KNOTS('',3,(#25518,#25519,#25520,#25521,#25522,
#25523,#25524,#25525,#25526,#25527,#25528,#25529,#25530,#25531,#25532,#25533,
#25534),.UNSPECIFIED.,.F.,.F.,(4,1,1,1,1,1,1,1,1,1,1,1,1,1,4),(59.6902604182061,
59.907207024815,60.405065113856,60.902923202897,61.400781291938,61.898639380979,
62.39649747002,62.8943555590609,63.3922136481019,63.8900717371429,64.3879298261839,
64.8857879152249,65.3836460042659,65.8815040933069,65.9734457253856),
 .UNSPECIFIED.);
#397=B_SPLINE_CURVE_WITH_KNOTS('',3,(#25535,#25536,#25537,#25538,#25539,
#25540,#25541,#25542,#25543,#25544,#25545,#25546,#25547,#25548,#25549,#25550),
 .UNSPECIFIED.,.F.,.F.,(4,1,1,1,1,1,1,1,1,1,1,1,1,4),(59.690260418206,60.0758916557576,
60.5737497447986,61.0716078338395,61.5694659228805,62.0673240119215,62.5651821009625,
63.0630401900035,63.5608982790445,64.0587563680855,64.5566144571264,65.0544725461674,
65.5523306352084,65.9734457253856),.UNSPECIFIED.);
#398=B_SPLINE_CURVE_WITH_KNOTS('',3,(#25555,#25556,#25557,#25558,#25559,
#25560,#25561,#25562,#25563,#25564,#25565,#25566,#25567,#25568,#25569,#25570,
#25571),.UNSPECIFIED.,.F.,.F.,(4,1,1,1,1,1,1,1,1,1,1,1,1,1,4),(53.4070751110264,
53.4350518672822,53.9329099563232,54.4307680453642,54.9286261344052,55.4264842234462,
55.9243423124872,56.4222004015281,56.9200584905691,57.4179165796101,57.9157746686511,
58.4136327576921,58.9114908467331,59.409348935774,59.6902604182061),
 .UNSPECIFIED.);
#399=B_SPLINE_CURVE_WITH_KNOTS('',3,(#25572,#25573,#25574,#25575,#25576,
#25577,#25578,#25579,#25580,#25581,#25582,#25583,#25584,#25585,#25586,#25587,
#25588),.UNSPECIFIED.,.F.,.F.,(4,1,1,1,1,1,1,1,1,1,1,1,1,1,4),(53.4070751110264,
53.6037364982248,54.1015945872658,54.5994526763067,55.0973107653477,55.5951688543887,
56.0930269434297,56.5908850324707,57.0887431215117,57.5866012105526,58.0844592995936,
58.5823173886346,59.0801754776756,59.5780335667166,59.690260418206),
 .UNSPECIFIED.);
#400=B_SPLINE_CURVE_WITH_KNOTS('',3,(#25593,#25594,#25595,#25596,#25597,
#25598,#25599,#25600,#25601,#25602,#25603,#25604,#25605,#25606,#25607,#25608),
 .UNSPECIFIED.,.F.,.F.,(4,1,1,1,1,1,1,1,1,1,1,1,1,4),(47.1238898038469,
47.4607547987904,47.9586128878314,48.4564709768724,48.9543290659134,49.4521871549543,
49.9500452439953,50.4479033330363,50.9457614220773,51.4436195111183,51.9414776001593,
52.4393356892003,52.9371937782412,53.4070751110264),.UNSPECIFIED.);
#401=B_SPLINE_CURVE_WITH_KNOTS('',3,(#25609,#25610,#25611,#25612,#25613,
#25614,#25615,#25616,#25617,#25618,#25619,#25620,#25621,#25622,#25623,#25624,
#25625),.UNSPECIFIED.,.F.,.F.,(4,1,1,1,1,1,1,1,1,1,1,1,1,1,4),(47.1238898038469,
47.131581340692,47.6294394297329,48.1272975187739,48.6251556078149,49.1230136968559,
49.6208717858969,50.1187298749379,50.6165879639789,51.1144460530198,51.6123041420608,
52.1101622311018,52.6080203201428,53.1058784091838,53.4070751110264),
 .UNSPECIFIED.);
#402=B_SPLINE_CURVE_WITH_KNOTS('',3,(#25630,#25631,#25632,#25633,#25634,
#25635,#25636,#25637,#25638,#25639,#25640,#25641,#25642,#25643,#25644,#25645,
#25646),.UNSPECIFIED.,.F.,.F.,(4,1,1,1,1,1,1,1,1,1,1,1,1,1,4),(40.8407044966673,
40.9885996412576,41.4864577302986,41.9843158193396,42.4821739083806,42.9800319974215,
43.4778900864625,43.9757481755035,44.4736062645445,44.9714643535855,45.4693224426265,
45.9671805316675,46.4650386207084,46.9628967097494,47.1238898038469),
 .UNSPECIFIED.);
#403=B_SPLINE_CURVE_WITH_KNOTS('',3,(#25647,#25648,#25649,#25650,#25651,
#25652,#25653,#25654,#25655,#25656,#25657,#25658,#25659,#25660,#25661,#25662),
 .UNSPECIFIED.,.F.,.F.,(4,1,1,1,1,1,1,1,1,1,1,1,1,4),(40.8407044966673,
41.1572842722001,41.6551423612411,42.1530004502821,42.6508585393231,43.1487166283641,
43.6465747174051,44.144432806446,44.642290895487,45.140148984528,45.638007073569,
46.13586516261,46.633723251651,47.1238898038469),.UNSPECIFIED.);
#404=B_SPLINE_CURVE_WITH_KNOTS('',3,(#25667,#25668,#25669,#25670,#25671,
#25672,#25673,#25674,#25675,#25676,#25677,#25678,#25679,#25680,#25681,#25682),
 .UNSPECIFIED.,.F.,.F.,(4,1,1,1,1,1,1,1,1,1,1,1,1,4),(34.5575191894876,
35.0143025727658,35.5121606618068,36.0100187508477,36.5078768398887,37.0057349289297,
37.5035930179707,38.0014511070117,38.4993091960527,38.9971672850937,39.4950253741346,
39.9928834631756,40.4907415522166,40.8407044966673),.UNSPECIFIED.);
#405=B_SPLINE_CURVE_WITH_KNOTS('',3,(#25683,#25684,#25685,#25686,#25687,
#25688,#25689,#25690,#25691,#25692,#25693,#25694,#25695,#25696,#25697,#25698,
#25699),.UNSPECIFIED.,.F.,.F.,(4,1,1,1,1,1,1,1,1,1,1,1,1,1,4),(34.5575191894876,
34.6851291146673,35.1829872037083,35.6808452927493,36.1787033817903,36.6765614708313,
37.1744195598722,37.6722776489132,38.1701357379542,38.6679938269952,39.1658519160362,
39.6637100050772,40.1615680941182,40.6594261831592,40.8407044966673),
 .UNSPECIFIED.);
#406=B_SPLINE_CURVE_WITH_KNOTS('',3,(#25704,#25705,#25706,#25707,#25708,
#25709,#25710,#25711,#25712,#25713,#25714,#25715,#25716,#25717,#25718,#25719,
#25720),.UNSPECIFIED.,.F.,.F.,(4,1,1,1,1,1,1,1,1,1,1,1,1,1,4),(28.274333882308,
28.542147415233,29.0400055042739,29.5378635933149,30.0357216823559,30.5335797713969,
31.0314378604379,31.5292959494789,32.0271540385199,32.5250121275608,33.0228702166018,
33.5207283056428,34.0185863946838,34.5164444837248,34.5575191894876),
 .UNSPECIFIED.);
#407=B_SPLINE_CURVE_WITH_KNOTS('',3,(#25721,#25722,#25723,#25724,#25725,
#25726,#25727,#25728,#25729,#25730,#25731,#25732,#25733,#25734,#25735,#25736),
 .UNSPECIFIED.,.F.,.F.,(4,1,1,1,1,1,1,1,1,1,1,1,1,4),(28.274333882308,28.7108320461755,
29.2086901352165,29.7065482242575,30.2044063132985,30.7022644023394,31.2001224913804,
31.6979805804214,32.1958386694624,32.6936967585034,33.1915548475444,33.6894129365854,
34.1872710256263,34.5575191894876),.UNSPECIFIED.);
#408=B_SPLINE_CURVE_WITH_KNOTS('',3,(#25741,#25742,#25743,#25744,#25745,
#25746,#25747,#25748,#25749,#25750,#25751,#25752,#25753,#25754,#25755,#25756,
#25757),.UNSPECIFIED.,.F.,.F.,(4,1,1,1,1,1,1,1,1,1,1,1,1,1,4),(21.9911485751285,
22.0699922577002,22.5678503467411,23.0657084357821,23.5635665248231,24.0614246138641,
24.5592827029051,25.0571407919461,25.554998880987,26.052856970028,26.550715059069,
27.04857314811,27.546431237151,28.044289326192,28.274333882308),
 .UNSPECIFIED.);
#409=B_SPLINE_CURVE_WITH_KNOTS('',3,(#25758,#25759,#25760,#25761,#25762,
#25763,#25764,#25765,#25766,#25767,#25768,#25769,#25770,#25771,#25772,#25773,
#25774),.UNSPECIFIED.,.F.,.F.,(4,1,1,1,1,1,1,1,1,1,1,1,1,1,4),(21.9911485751285,
22.2386768886427,22.7365349776837,23.2343930667247,23.7322511557656,24.2301092448066,
24.7279673338476,25.2258254228886,25.7236835119296,26.2215416009706,26.7193996900116,
27.2172577790525,27.7151158680935,28.2129739571345,28.274333882308),
 .UNSPECIFIED.);
#410=B_SPLINE_CURVE_WITH_KNOTS('',3,(#25779,#25780,#25781,#25782,#25783,
#25784,#25785,#25786,#25787,#25788,#25789,#25790,#25791,#25792,#25793,#25794),
 .UNSPECIFIED.,.F.,.F.,(4,1,1,1,1,1,1,1,1,1,1,1,1,4),(15.7079632679489,
16.0956951892083,16.5935532782493,17.0914113672903,17.5892694563313,18.0871275453723,
18.5849856344133,19.0828437234542,19.5807018124952,20.0785599015362,20.5764179905772,
21.0742760796182,21.5721341686592,21.9911485751285),.UNSPECIFIED.);
#411=B_SPLINE_CURVE_WITH_KNOTS('',3,(#25795,#25796,#25797,#25798,#25799,
#25800,#25801,#25802,#25803,#25804,#25805,#25806,#25807,#25808,#25809,#25810,
#25811),.UNSPECIFIED.,.F.,.F.,(4,1,1,1,1,1,1,1,1,1,1,1,1,1,4),(15.7079632679489,
15.7665217311099,16.2643798201509,16.7622379091919,17.2600959982328,17.7579540872738,
18.2558121763148,18.7536702653558,19.2515283543968,19.7493864434378,20.2472445324787,
20.7451026215197,21.2429607105607,21.7408187996017,21.9911485751285),
 .UNSPECIFIED.);
#412=B_SPLINE_CURVE_WITH_KNOTS('',3,(#25817,#25818,#25819,#25820,#25821,
#25822,#25823,#25824,#25825,#25826,#25827,#25828,#25829,#25830,#25831,#25832),
 .UNSPECIFIED.,.F.,.F.,(4,3,3,3,3,4),(-4.09299088010945,-3.9439579802929,
-3.45096323275628,-2.95796848521967,-2.46497373768306,-2.07752579179387),
 .UNSPECIFIED.);
#413=B_SPLINE_CURVE_WITH_KNOTS('',3,(#25835,#25836,#25837,#25838,#25839,
#25840,#25841,#25842,#25843,#25844),.UNSPECIFIED.,.F.,.F.,(4,3,3,4),(0.,
0.492994747536612,0.985989495073225,1.12612756527419),.UNSPECIFIED.);
#414=B_SPLINE_CURVE_WITH_KNOTS('',3,(#25849,#25850,#25851,#25852,#25853,
#25854,#25855,#25856,#25857,#25858,#25859,#25860,#25861,#25862,#25863,#25864,
#25865,#25866,#25867,#25868,#25869,#25870,#25871,#25872,#25873,#25874,#25875,
#25876,#25877,#25878,#25879,#25880,#25881,#25882,#25883,#25884,#25885,#25886,
#25887,#25888,#25889,#25890,#25891),.UNSPECIFIED.,.F.,.F.,(4,3,3,3,3,3,
3,3,3,3,3,3,3,3,4),(-10.3761761872891,-10.3528896982689,-9.85989495073224,
-9.36690020319563,-8.87390545565902,-8.38091070812241,-7.88791596058579,
-7.39492121304918,-6.90192646551257,-6.40893171797596,-5.91593697043935,
-5.42294222290273,-4.92994747536612,-4.43695272782951,-4.09299088010945),
 .UNSPECIFIED.);
#415=B_SPLINE_CURVE_WITH_KNOTS('',3,(#25892,#25893,#25894,#25895,#25896,
#25897,#25898,#25899,#25900,#25901,#25902,#25903,#25904,#25905,#25906,#25907,
#25908,#25909,#25910,#25911,#25912,#25913,#25914,#25915,#25916,#25917,#25918,
#25919,#25920,#25921,#25922,#25923,#25924,#25925,#25926,#25927,#25928,#25929,
#25930,#25931,#25932,#25933,#25934),.UNSPECIFIED.,.F.,.F.,(4,3,3,3,3,3,
3,3,3,3,3,3,3,3,4),(1.12612756527419,1.47898424260984,1.97197899014645,
2.46497373768306,2.95796848521968,3.45096323275629,3.9439579802929,4.43695272782951,
4.92994747536613,5.42294222290274,5.91593697043935,6.40893171797596,6.90192646551257,
7.39492121304918,7.40931287245371),.UNSPECIFIED.);
#416=B_SPLINE_CURVE_WITH_KNOTS('',3,(#25939,#25940,#25941,#25942,#25943,
#25944,#25945,#25946,#25947,#25948,#25949,#25950,#25951,#25952,#25953,#25954,
#25955,#25956,#25957,#25958,#25959,#25960,#25961,#25962,#25963,#25964,#25965,
#25966,#25967,#25968,#25969,#25970,#25971,#25972,#25973,#25974,#25975,#25976,
#25977,#25978),.UNSPECIFIED.,.F.,.F.,(4,3,3,3,3,3,3,3,3,3,3,3,3,4),(-16.6593614944687,
-16.2688266687082,-15.7758319211716,-15.282837173635,-14.7898424260984,
-14.2968476785617,-13.8038529310251,-13.3108581834885,-12.8178634359519,
-12.3248686884153,-11.8318739408787,-11.3388791933421,-10.8458844458055,
-10.3761761872891),.UNSPECIFIED.);
#417=B_SPLINE_CURVE_WITH_KNOTS('',3,(#25979,#25980,#25981,#25982,#25983,
#25984,#25985,#25986,#25987,#25988,#25989,#25990,#25991,#25992,#25993,#25994,
#25995,#25996,#25997,#25998,#25999,#26000,#26001,#26002,#26003,#26004,#26005,
#26006,#26007,#26008,#26009,#26010,#26011,#26012,#26013,#26014,#26015,#26016,
#26017,#26018),.UNSPECIFIED.,.F.,.F.,(4,3,3,3,3,3,3,3,3,3,3,3,3,4),(7.40931287245371,
7.8879159605858,8.38091070812241,8.87390545565902,9.36690020319563,9.85989495073224,
10.3528896982689,10.8458844458055,11.3388791933421,11.8318739408787,12.3248686884153,
12.8178634359519,13.3108581834885,13.6924981796333),.UNSPECIFIED.);
#418=B_SPLINE_CURVE_WITH_KNOTS('',3,(#26023,#26024,#26025,#26026,#26027,
#26028,#26029,#26030,#26031,#26032,#26033,#26034,#26035,#26036,#26037,#26038,
#26039,#26040,#26041,#26042,#26043,#26044,#26045,#26046,#26047,#26048,#26049,
#26050,#26051,#26052,#26053,#26054,#26055,#26056,#26057,#26058,#26059,#26060,
#26061,#26062,#26063,#26064,#26065),.UNSPECIFIED.,.F.,.F.,(4,3,3,3,3,3,
3,3,3,3,3,3,3,3,4),(-22.9425468016483,-22.6777583866842,-22.1847636391475,
-21.6917688916109,-21.1987741440743,-20.7057793965377,-20.2127846490011,
-19.7197899014645,-19.2267951539279,-18.7338004063913,-18.2408056588546,
-17.747810911318,-17.2548161637814,-16.7618214162448,-16.6593614944687),
 .UNSPECIFIED.);
#419=B_SPLINE_CURVE_WITH_KNOTS('',3,(#26066,#26067,#26068,#26069,#26070,
#26071,#26072,#26073,#26074,#26075,#26076,#26077,#26078,#26079,#26080,#26081,
#26082,#26083,#26084,#26085,#26086,#26087,#26088,#26089,#26090,#26091,#26092,
#26093,#26094,#26095,#26096,#26097,#26098,#26099,#26100,#26101,#26102,#26103,
#26104,#26105,#26106,#26107,#26108),.UNSPECIFIED.,.F.,.F.,(4,3,3,3,3,3,
3,3,3,3,3,3,3,3,4),(13.6924981796333,13.8038529310251,14.2968476785617,
14.7898424260984,15.282837173635,15.7758319211716,16.2688266687082,16.7618214162448,
17.2548161637814,17.747810911318,18.2408056588546,18.7338004063913,19.2267951539279,
19.7197899014645,19.9756834868129),.UNSPECIFIED.);
#420=B_SPLINE_CURVE_WITH_KNOTS('',3,(#26113,#26114,#26115,#26116,#26117,
#26118,#26119,#26120,#26121,#26122,#26123,#26124,#26125,#26126,#26127,#26128,
#26129,#26130,#26131,#26132,#26133,#26134,#26135,#26136,#26137,#26138,#26139,
#26140,#26141,#26142,#26143,#26144,#26145,#26146,#26147,#26148,#26149,#26150,
#26151,#26152,#26153,#26154,#26155),.UNSPECIFIED.,.F.,.F.,(4,3,3,3,3,3,
3,3,3,3,3,3,3,3,4),(-29.2257321088278,-29.0866901046601,-28.5936953571235,
-28.1007006095869,-27.6077058620503,-27.1147111145137,-26.621716366977,
-26.1287216194404,-25.6357268719038,-25.1427321243672,-24.6497373768306,
-24.156742629294,-23.6637478817574,-23.1707531342208,-22.9425468016483),
 .UNSPECIFIED.);
#421=B_SPLINE_CURVE_WITH_KNOTS('',3,(#26156,#26157,#26158,#26159,#26160,
#26161,#26162,#26163,#26164,#26165,#26166,#26167,#26168,#26169,#26170,#26171,
#26172,#26173,#26174,#26175,#26176,#26177,#26178,#26179,#26180,#26181,#26182,
#26183,#26184,#26185,#26186,#26187,#26188,#26189,#26190,#26191,#26192,#26193,
#26194,#26195,#26196,#26197,#26198),.UNSPECIFIED.,.F.,.F.,(4,3,3,3,3,3,
3,3,3,3,3,3,3,3,4),(19.9756834868129,20.2127846490011,20.7057793965377,
21.1987741440743,21.6917688916109,22.1847636391475,22.6777583866842,23.1707531342208,
23.6637478817574,24.156742629294,24.6497373768306,25.1427321243672,25.6357268719038,
26.1287216194404,26.2588687939925),.UNSPECIFIED.);
#422=B_SPLINE_CURVE_WITH_KNOTS('',3,(#26203,#26204,#26205,#26206,#26207,
#26208,#26209,#26210,#26211,#26212,#26213,#26214,#26215,#26216,#26217,#26218,
#26219,#26220,#26221,#26222,#26223,#26224,#26225,#26226,#26227,#26228,#26229,
#26230,#26231,#26232,#26233,#26234,#26235,#26236,#26237,#26238,#26239,#26240,
#26241,#26242,#26243,#26244,#26245),.UNSPECIFIED.,.F.,.F.,(4,3,3,3,3,3,
3,3,3,3,3,3,3,3,4),(-35.5089174160074,-35.4956218226361,-35.0026270750994,
-34.5096323275628,-34.0166375800262,-33.5236428324896,-33.030648084953,
-32.5376533374164,-32.0446585898798,-31.5516638423432,-31.0586690948066,
-30.5656743472699,-30.0726795997333,-29.5796848521967,-29.2257321088278),
 .UNSPECIFIED.);
#423=B_SPLINE_CURVE_WITH_KNOTS('',3,(#26246,#26247,#26248,#26249,#26250,
#26251,#26252,#26253,#26254,#26255,#26256,#26257,#26258,#26259,#26260,#26261,
#26262,#26263,#26264,#26265,#26266,#26267,#26268,#26269,#26270,#26271,#26272,
#26273,#26274,#26275,#26276,#26277,#26278,#26279,#26280,#26281,#26282,#26283,
#26284,#26285,#26286,#26287,#26288),.UNSPECIFIED.,.F.,.F.,(4,3,3,3,3,3,
3,3,3,3,3,3,3,3,4),(26.2588687939925,26.621716366977,27.1147111145136,27.6077058620503,
28.1007006095869,28.5936953571235,29.0866901046601,29.5796848521967,30.0726795997333,
30.5656743472699,31.0586690948066,31.5516638423432,32.0446585898798,32.5376533374164,
32.5420541011721),.UNSPECIFIED.);
#424=B_SPLINE_CURVE_WITH_KNOTS('',3,(#26293,#26294,#26295,#26296,#26297,
#26298,#26299,#26300,#26301,#26302,#26303,#26304,#26305,#26306,#26307,#26308,
#26309,#26310,#26311,#26312,#26313,#26314,#26315,#26316,#26317,#26318,#26319,
#26320,#26321,#26322,#26323,#26324,#26325,#26326,#26327,#26328,#26329,#26330,
#26331,#26332),.UNSPECIFIED.,.F.,.F.,(4,3,3,3,3,3,3,3,3,3,3,3,3,4),(-41.792102723187,
-41.4115587930754,-40.9185640455388,-40.4255692980022,-39.9325745504656,
-39.439579802929,-38.9465850553923,-38.4535903078557,-37.9605955603191,
-37.4676008127825,-36.9746060652459,-36.4816113177093,-35.9886165701727,
-35.5089174160074),.UNSPECIFIED.);
#425=B_SPLINE_CURVE_WITH_KNOTS('',3,(#26333,#26334,#26335,#26336,#26337,
#26338,#26339,#26340,#26341,#26342,#26343,#26344,#26345,#26346,#26347,#26348,
#26349,#26350,#26351,#26352,#26353,#26354,#26355,#26356,#26357,#26358,#26359,
#26360,#26361,#26362,#26363,#26364,#26365,#26366,#26367,#26368,#26369,#26370,
#26371,#26372),.UNSPECIFIED.,.F.,.F.,(4,3,3,3,3,3,3,3,3,3,3,3,3,4),(32.5420541011721,
33.030648084953,33.5236428324896,34.0166375800262,34.5096323275628,35.0026270750995,
35.4956218226361,35.9886165701727,36.4816113177093,36.9746060652459,37.4676008127825,
37.9605955603191,38.4535903078557,38.8252394083517),.UNSPECIFIED.);
#426=B_SPLINE_CURVE_WITH_KNOTS('',3,(#26377,#26378,#26379,#26380,#26381,
#26382,#26383,#26384,#26385,#26386,#26387,#26388,#26389,#26390,#26391,#26392,
#26393,#26394,#26395,#26396,#26397,#26398,#26399,#26400,#26401,#26402,#26403,
#26404,#26405,#26406,#26407,#26408,#26409,#26410,#26411,#26412,#26413,#26414,
#26415,#26416,#26417,#26418,#26419),.UNSPECIFIED.,.F.,.F.,(4,3,3,3,3,3,
3,3,3,3,3,3,3,3,4),(-48.0752880303666,-47.8204905110514,-47.3274957635147,
-46.8345010159781,-46.3415062684415,-45.8485115209049,-45.3555167733683,
-44.8625220258317,-44.3695272782951,-43.8765325307585,-43.3835377832218,
-42.8905430356852,-42.3975482881486,-41.904553540612,-41.792102723187),
 .UNSPECIFIED.);
#427=B_SPLINE_CURVE_WITH_KNOTS('',3,(#26420,#26421,#26422,#26423,#26424,
#26425,#26426,#26427,#26428,#26429,#26430,#26431,#26432,#26433,#26434,#26435,
#26436,#26437,#26438,#26439,#26440,#26441,#26442,#26443,#26444,#26445,#26446,
#26447,#26448,#26449,#26450,#26451,#26452,#26453,#26454,#26455,#26456,#26457,
#26458,#26459,#26460,#26461,#26462),.UNSPECIFIED.,.F.,.F.,(4,3,3,3,3,3,
3,3,3,3,3,3,3,3,4),(38.8252394083517,38.9465850553923,39.439579802929,39.9325745504656,
40.4255692980022,40.9185640455388,41.4115587930754,41.904553540612,42.3975482881486,
42.8905430356852,43.3835377832219,43.8765325307585,44.3695272782951,44.8625220258317,
45.1084247155313),.UNSPECIFIED.);
#428=B_SPLINE_CURVE_WITH_KNOTS('',3,(#26467,#26468,#26469,#26470,#26471,
#26472,#26473,#26474,#26475,#26476,#26477,#26478,#26479,#26480,#26481,#26482,
#26483,#26484,#26485,#26486,#26487,#26488,#26489,#26490,#26491,#26492,#26493,
#26494,#26495,#26496,#26497,#26498,#26499,#26500,#26501,#26502,#26503,#26504,
#26505,#26506,#26507,#26508,#26509),.UNSPECIFIED.,.F.,.F.,(4,3,3,3,3,3,
3,3,3,3,3,3,3,3,4),(-54.3584733375463,-54.2294222290273,-53.7364274814907,
-53.2434327339541,-52.7504379864175,-52.2574432388809,-51.7644484913443,
-51.2714537438076,-50.778458996271,-50.2854642487344,-49.7924695011978,
-49.2994747536612,-48.8064800061246,-48.313485258588,-48.0752880303666),
 .UNSPECIFIED.);
#429=B_SPLINE_CURVE_WITH_KNOTS('',3,(#26510,#26511,#26512,#26513,#26514,
#26515,#26516,#26517,#26518,#26519,#26520,#26521,#26522,#26523,#26524,#26525,
#26526,#26527,#26528,#26529,#26530,#26531,#26532,#26533,#26534,#26535,#26536,
#26537,#26538,#26539,#26540,#26541,#26542,#26543,#26544,#26545,#26546,#26547,
#26548,#26549,#26550,#26551,#26552),.UNSPECIFIED.,.F.,.F.,(4,3,3,3,3,3,
3,3,3,3,3,3,3,3,4),(45.1084247155313,45.3555167733683,45.8485115209049,
46.3415062684415,46.8345010159781,47.3274957635147,47.8204905110514,48.313485258588,
48.8064800061246,49.2994747536612,49.7924695011978,50.2854642487344,50.778458996271,
51.2714537438076,51.3916100227108),.UNSPECIFIED.);
#430=B_SPLINE_CURVE_WITH_KNOTS('',3,(#26557,#26558,#26559,#26560,#26561,
#26562,#26563,#26564,#26565,#26566,#26567,#26568,#26569,#26570,#26571,#26572,
#26573,#26574,#26575,#26576,#26577,#26578,#26579,#26580,#26581,#26582,#26583,
#26584,#26585,#26586,#26587,#26588,#26589,#26590,#26591,#26592,#26593,#26594,
#26595,#26596,#26597,#26598,#26599),.UNSPECIFIED.,.F.,.F.,(4,3,3,3,3,3,
3,3,3,3,3,3,3,3,4),(-60.6416586447258,-60.6383539470033,-60.1453591994667,
-59.6523644519301,-59.1593697043935,-58.6663749568568,-58.1733802093202,
-57.6803854617836,-57.187390714247,-56.6943959667104,-56.2014012191738,
-55.7084064716372,-55.2154117241005,-54.7224169765639,-54.3584733375463),
 .UNSPECIFIED.);
#431=B_SPLINE_CURVE_WITH_KNOTS('',3,(#26600,#26601,#26602,#26603,#26604,
#26605,#26606,#26607,#26608,#26609,#26610,#26611,#26612,#26613,#26614,#26615,
#26616,#26617,#26618,#26619,#26620,#26621,#26622,#26623,#26624,#26625,#26626,
#26627,#26628,#26629,#26630,#26631,#26632,#26633,#26634,#26635,#26636,#26637,
#26638,#26639),.UNSPECIFIED.,.F.,.F.,(4,3,3,3,3,3,3,3,3,3,3,3,3,4),(51.3916100227108,
51.7644484913443,52.2574432388809,52.7504379864175,53.2434327339541,53.7364274814907,
54.2294222290273,54.7224169765639,55.2154117241005,55.7084064716371,56.2014012191738,
56.6943959667104,57.187390714247,57.6747953298905),.UNSPECIFIED.);
#432=B_SPLINE_CURVE_WITH_KNOTS('',3,(#26646,#26647,#26648,#26649,#26650,
#26651,#26652,#26653,#26654,#26655,#26656,#26657,#26658,#26659,#26660,#26661,
#26662,#26663,#26664,#26665,#26666,#26667,#26668,#26669,#26670,#26671,#26672,
#26673,#26674,#26675,#26676,#26677,#26678,#26679),.UNSPECIFIED.,.F.,.F.,
(4,3,3,3,3,3,3,3,3,3,3,4),(-66.061296169906,-65.5683014223694,-65.0753066748328,
-64.5823119272962,-64.0893171797595,-63.5963224322229,-63.1033276846864,
-62.6103329371497,-62.1173381896131,-61.6243434420765,-61.1313486945399,
-60.6416586447258),.UNSPECIFIED.);
#433=B_SPLINE_CURVE_WITH_KNOTS('',3,(#26680,#26681,#26682,#26683,#26684,
#26685,#26686,#26687,#26688,#26689,#26690,#26691,#26692,#26693,#26694,#26695,
#26696,#26697,#26698,#26699,#26700,#26701,#26702,#26703,#26704,#26705,#26706,
#26707,#26708,#26709,#26710,#26711,#26712,#26713,#26714,#26715,#26716,#26717,
#26718,#26719,#26720,#26721,#26722),.UNSPECIFIED.,.F.,.F.,(4,3,3,3,3,3,
3,3,3,3,3,3,3,3,4),(57.6747953298905,57.6803854617836,58.1733802093202,
58.6663749568568,59.1593697043934,59.65236445193,60.1453591994666,60.6383539470033,
61.1313486945399,61.6243434420765,62.1173381896131,62.6103329371497,63.1033276846863,
63.5963224322229,63.95798063707),.UNSPECIFIED.);
#434=B_SPLINE_CURVE_WITH_KNOTS('',3,(#26728,#26729,#26730,#26731,#26732,
#26733,#26734,#26735,#26736,#26737),.UNSPECIFIED.,.F.,.F.,(4,1,1,1,1,1,
1,4),(72.2566310325652,72.7463210823793,73.2393158299159,73.7323105774525,
74.2253053249892,74.7183000725258,75.2112948200624,75.5987427659515),
 .UNSPECIFIED.);
#435=B_SPLINE_CURVE_WITH_KNOTS('',3,(#26740,#26741,#26742,#26743,#26744,
#26745,#26746,#26747),.UNSPECIFIED.,.F.,.F.,(4,1,1,1,1,4),(72.2566310325652,
72.3879675752547,72.8809623227913,73.3739570703279,73.8669518178645,74.3599465654011),
 .UNSPECIFIED.);
#436=B_SPLINE_CURVE_WITH_KNOTS('',3,(#26752,#26753,#26754,#26755,#26756,
#26757,#26758,#26759,#26760,#26761,#26762,#26763,#26764,#26765,#26766,#26767,
#26768),.UNSPECIFIED.,.F.,.F.,(4,1,1,1,1,1,1,1,1,1,1,1,1,1,4),(65.9734457253857,
66.3373893644034,66.83038411194,67.3233788594766,67.8163736070132,68.3093683545498,
68.8023631020864,69.295357849623,69.7883525971596,70.2813473446963,70.7743420922329,
71.2673368397695,71.7603315873061,72.2533263348427,72.2566310325652),
 .UNSPECIFIED.);
#437=B_SPLINE_CURVE_WITH_KNOTS('',3,(#26769,#26770,#26771,#26772,#26773,
#26774,#26775,#26776,#26777,#26778,#26779,#26780,#26781,#26782,#26783,#26784,
#26785),.UNSPECIFIED.,.F.,.F.,(4,1,1,1,1,1,1,1,1,1,1,1,1,1,4),(65.9734457253857,
65.9790358572787,66.4720306048154,66.965025352352,67.4580200998886,67.9510148474252,
68.4440095949618,68.9370043424984,69.429999090035,69.9229938375716,70.4159885851083,
70.9089833326449,71.4019780801815,71.8949728277181,72.2566310325652),
 .UNSPECIFIED.);
#438=B_SPLINE_CURVE_WITH_KNOTS('',3,(#26790,#26791,#26792,#26793,#26794,
#26795,#26796,#26797,#26798,#26799,#26800,#26801,#26802,#26803,#26804,#26805,
#26806),.UNSPECIFIED.,.F.,.F.,(4,1,1,1,1,1,1,1,1,1,1,1,1,1,4),(59.690260418206,
59.9284576464274,60.421452393964,60.9144471415006,61.4074418890372,61.9004366365738,
62.3934313841105,62.8864261316471,63.3794208791837,63.8724156267203,64.3654103742569,
64.8584051217935,65.3513998693301,65.8443946168668,65.9734457253857),
 .UNSPECIFIED.);
#439=B_SPLINE_CURVE_WITH_KNOTS('',3,(#26807,#26808,#26809,#26810,#26811,
#26812,#26813,#26814,#26815,#26816,#26817,#26818,#26819,#26820,#26821,#26822),
 .UNSPECIFIED.,.F.,.F.,(4,1,1,1,1,1,1,1,1,1,1,1,1,4),(59.690260418206,60.0630988868394,
60.556093634376,61.0490883819126,61.5420831294492,62.0350778769859,62.5280726245225,
63.0210673720591,63.5140621195957,64.0070568671323,64.5000516146689,64.9930463622055,
65.4860411097421,65.9734457253857),.UNSPECIFIED.);
#440=B_SPLINE_CURVE_WITH_KNOTS('',3,(#26827,#26828,#26829,#26830,#26831,
#26832,#26833,#26834,#26835,#26836,#26837,#26838,#26839,#26840,#26841,#26842,
#26843),.UNSPECIFIED.,.F.,.F.,(4,1,1,1,1,1,1,1,1,1,1,1,1,1,4),(53.4070751110265,
53.5195259284514,54.0125206759881,54.5055154235247,54.9985101710613,55.4915049185979,
55.9844996661345,56.4774944136711,56.9704891612077,57.4634839087443,57.956478656281,
58.4494734038176,58.9424681513542,59.4354628988908,59.690260418206),
 .UNSPECIFIED.);
#441=B_SPLINE_CURVE_WITH_KNOTS('',3,(#26844,#26845,#26846,#26847,#26848,
#26849,#26850,#26851,#26852,#26853,#26854,#26855,#26856,#26857,#26858,#26859,
#26860),.UNSPECIFIED.,.F.,.F.,(4,1,1,1,1,1,1,1,1,1,1,1,1,1,4),(53.4070751110265,
53.6541671688635,54.1471619164001,54.6401566639367,55.1331514114733,55.6261461590099,
56.1191409065465,56.6121356540831,57.1051304016197,57.5981251491563,58.091119896693,
58.5841146442296,59.0771093917662,59.5701041393028,59.690260418206),
 .UNSPECIFIED.);
#442=B_SPLINE_CURVE_WITH_KNOTS('',3,(#26865,#26866,#26867,#26868,#26869,
#26870,#26871,#26872,#26873,#26874,#26875,#26876,#26877,#26878,#26879,#26880),
 .UNSPECIFIED.,.F.,.F.,(4,1,1,1,1,1,1,1,1,1,1,1,1,4),(47.1238898038469,
47.6035889580121,48.0965837055487,48.5895784530853,49.0825732006219,49.5755679481586,
50.0685626956952,50.5615574432318,51.0545521907684,51.547546938305,52.0405416858416,
52.5335364333782,53.0265311809148,53.4070751110265),.UNSPECIFIED.);
#443=B_SPLINE_CURVE_WITH_KNOTS('',3,(#26881,#26882,#26883,#26884,#26885,
#26886,#26887,#26888,#26889,#26890,#26891,#26892,#26893,#26894,#26895,#26896,
#26897),.UNSPECIFIED.,.F.,.F.,(4,1,1,1,1,1,1,1,1,1,1,1,1,1,4),(47.1238898038469,
47.2452354508875,47.7382301984241,48.2312249459607,48.7242196934973,49.2172144410339,
49.7102091885705,50.2032039361072,50.6961986836438,51.1891934311804,51.682188178717,
52.1751829262536,52.6681776737902,53.1611724213268,53.4070751110265),
 .UNSPECIFIED.);
#444=B_SPLINE_CURVE_WITH_KNOTS('',3,(#26902,#26903,#26904,#26905,#26906,
#26907,#26908,#26909,#26910,#26911,#26912,#26913,#26914,#26915,#26916,#26917,
#26918),.UNSPECIFIED.,.F.,.F.,(4,1,1,1,1,1,1,1,1,1,1,1,1,1,4),(40.8407044966673,
41.1946572400362,41.6876519875728,42.1806467351094,42.673641482646,43.1666362301826,
43.6596309777192,44.1526257252558,44.6456204727924,45.138615220329,45.6316099678657,
46.1246047154023,46.6175994629389,47.1105942104755,47.1238898038469),
 .UNSPECIFIED.);
#445=B_SPLINE_CURVE_WITH_KNOTS('',3,(#26919,#26920,#26921,#26922,#26923,
#26924,#26925,#26926,#26927,#26928,#26929,#26930,#26931,#26932,#26933,#26934),
 .UNSPECIFIED.,.F.,.F.,(4,1,1,1,1,1,1,1,1,1,1,1,1,4),(40.8407044966673,
41.3292984804481,41.8222932279848,42.3152879755214,42.808282723058,43.3012774705946,
43.7942722181312,44.2872669656678,44.7802617132044,45.273256460741,45.7662512082777,
46.2592459558143,46.7522407033509,47.1238898038469),.UNSPECIFIED.);
#446=B_SPLINE_CURVE_WITH_KNOTS('',3,(#26939,#26940,#26941,#26942,#26943,
#26944,#26945,#26946,#26947,#26948,#26949,#26950,#26951,#26952,#26953,#26954,
#26955),.UNSPECIFIED.,.F.,.F.,(4,1,1,1,1,1,1,1,1,1,1,1,1,1,4),(34.5575191894877,
34.7857255220602,35.2787202695968,35.7717150171334,36.26470976467,36.7577045122066,
37.2506992597433,37.7436940072799,38.2366887548165,38.7296835023531,39.2226782498897,
39.7156729974263,40.2086677449629,40.7016624924995,40.8407044966673),
 .UNSPECIFIED.);
#447=B_SPLINE_CURVE_WITH_KNOTS('',3,(#26956,#26957,#26958,#26959,#26960,
#26961,#26962,#26963,#26964,#26965,#26966,#26967,#26968,#26969,#26970,#26971,
#26972),.UNSPECIFIED.,.F.,.F.,(4,1,1,1,1,1,1,1,1,1,1,1,1,1,4),(34.5575191894877,
34.9203667624722,35.4133615100088,35.9063562575454,36.399351005082,36.8923457526186,
37.3853405001553,37.8783352476919,38.3713299952285,38.8643247427651,39.3573194903017,
39.8503142378383,40.3433089853749,40.8363037329115,40.8407044966673),
 .UNSPECIFIED.);
#448=B_SPLINE_CURVE_WITH_KNOTS('',3,(#26977,#26978,#26979,#26980,#26981,
#26982,#26983,#26984,#26985,#26986,#26987,#26988,#26989,#26990,#26991,#26992,
#26993),.UNSPECIFIED.,.F.,.F.,(4,1,1,1,1,1,1,1,1,1,1,1,1,1,4),(28.2743338823081,
28.3767938040842,28.8697885516209,29.3627832991575,29.8557780466941,30.3487727942307,
30.8417675417673,31.3347622893039,31.8277570368405,32.3207517843771,32.8137465319137,
33.3067412794504,33.799736026987,34.2927307745236,34.5575191894877),
 .UNSPECIFIED.);
#449=B_SPLINE_CURVE_WITH_KNOTS('',3,(#26994,#26995,#26996,#26997,#26998,
#26999,#27000,#27001,#27002,#27003,#27004,#27005,#27006,#27007,#27008,#27009,
#27010),.UNSPECIFIED.,.F.,.F.,(4,1,1,1,1,1,1,1,1,1,1,1,1,1,4),(28.2743338823081,
28.5114350444962,29.0044297920328,29.4974245395695,29.9904192871061,30.4834140346427,
30.9764087821793,31.4694035297159,31.9623982772525,32.4553930247891,32.9483877723257,
33.4413825198624,33.934377267399,34.4273720149356,34.5575191894877),
 .UNSPECIFIED.);
#450=B_SPLINE_CURVE_WITH_KNOTS('',3,(#27015,#27016,#27017,#27018,#27019,
#27020,#27021,#27022,#27023,#27024,#27025,#27026,#27027,#27028,#27029,#27030),
 .UNSPECIFIED.,.F.,.F.,(4,1,1,1,1,1,1,1,1,1,1,1,1,4),(21.9911485751285,
22.4608568336449,22.9538515811815,23.4468463287181,23.9398410762547,24.4328358237913,
24.925830571328,25.4188253188646,25.9118200664012,26.4048148139378,26.8978095614744,
27.390804309011,27.8837990565476,28.2743338823081),.UNSPECIFIED.);
#451=B_SPLINE_CURVE_WITH_KNOTS('',3,(#27031,#27032,#27033,#27034,#27035,
#27036,#27037,#27038,#27039,#27040,#27041,#27042,#27043,#27044,#27045,#27046,
#27047),.UNSPECIFIED.,.F.,.F.,(4,1,1,1,1,1,1,1,1,1,1,1,1,1,4),(21.9911485751285,
22.1025033265203,22.5954980740569,23.0884928215935,23.5814875691301,24.0744823166667,
24.5674770642033,25.06047181174,25.5534665592766,26.0464613068132,26.5394560543498,
27.0324508018864,27.525445549423,28.0184402969596,28.2743338823081),
 .UNSPECIFIED.);
#452=B_SPLINE_CURVE_WITH_KNOTS('',3,(#27052,#27053,#27054,#27055,#27056,
#27057,#27058,#27059,#27060,#27061,#27062,#27063,#27064,#27065,#27066,#27067,
#27068),.UNSPECIFIED.,.F.,.F.,(4,1,1,1,1,1,1,1,1,1,1,1,1,1,4),(15.7079632679489,
16.0519251156689,16.5449198632055,17.0379146107422,17.5309093582788,18.0239041058154,
18.516898853352,19.0098936008886,19.5028883484252,19.9958830959618,20.4888778434984,
20.9818725910351,21.4748673385717,21.9678620861083,21.9911485751285),
 .UNSPECIFIED.);
#453=B_SPLINE_CURVE_WITH_KNOTS('',3,(#27069,#27070,#27071,#27072,#27073,
#27074,#27075,#27076,#27077,#27078,#27079,#27080,#27081,#27082,#27083,#27084),
 .UNSPECIFIED.,.F.,.F.,(4,1,1,1,1,1,1,1,1,1,1,1,1,4),(15.7079632679489,
16.1865663560809,16.6795611036176,17.1725558511542,17.6655505986908,18.1585453462274,
18.651540093764,19.1445348413006,19.6375295888372,20.1305243363738,20.6235190839104,
21.1165138314471,21.6095085789837,21.9911485751285),.UNSPECIFIED.);
#454=B_SPLINE_CURVE_WITH_KNOTS('',3,(#27123,#27124,#27125,#27126,#27127,
#27128,#27129,#27130,#27131,#27132,#27133,#27134,#27135,#27136,#27137,#27138,
#27139,#27140,#27141,#27142,#27143,#27144,#27145,#27146,#27147,#27148,#27149,
#27150,#27151,#27152,#27153,#27154,#27155,#27156,#27157,#27158,#27159,#27160,
#27161,#27162,#27163,#27164,#27165,#27166,#27167,#27168,#27169,#27170,#27171,
#27172,#27173,#27174,#27175,#27176,#27177,#27178,#27179,#27180,#27181,#27182,
#27183,#27184,#27185,#27186,#27187,#27188,#27189,#27190,#27191,#27192,#27193,
#27194,#27195,#27196,#27197,#27198,#27199,#27200,#27201,#27202,#27203,#27204,
#27205,#27206,#27207,#27208,#27209,#27210,#27211,#27212,#27213,#27214,#27215,
#27216,#27217,#27218,#27219,#27220,#27221,#27222,#27223,#27224,#27225,#27226,
#27227,#27228,#27229,#27230,#27231,#27232,#27233,#27234,#27235,#27236,#27237,
#27238,#27239,#27240,#27241,#27242,#27243,#27244,#27245,#27246,#27247,#27248,
#27249,#27250,#27251,#27252,#27253,#27254,#27255,#27256,#27257,#27258,#27259,
#27260,#27261),.UNSPECIFIED.,.F.,.F.,(4,3,3,3,3,3,3,3,3,3,3,3,3,3,3,3,3,
3,3,3,3,3,3,3,3,3,3,3,3,3,3,3,3,3,3,3,3,3,3,3,3,3,3,3,3,3,4),(-3.33140537618017,
-3.22326787461695,-3.15817079917648,-3.049853301467,-2.96298085620029,-2.9249741613961,
-2.90862147149683,-2.89605517458874,-2.78842365923039,-2.68003617925612,
-2.57290868632918,-2.51839994958021,-2.48953284996429,-2.47285249228237,
-2.36566522894994,-2.35487373933332,-2.24815410350468,-2.14082940646807,
-2.03352875005321,-1.92687843487524,-1.88101360087459,-1.8578477981616,
-1.84418934496722,-1.73779564851565,-1.63148467619083,-1.55995976287002,
-1.45341767338637,-1.34699981245266,-1.27548160451177,-1.24419238853763,
-1.23174198713026,-1.22128582434211,-1.1161023209359,-1.01033276551643,
-0.904839743637061,-0.80044976709345,-0.774854148925534,-0.677997380309842,
-0.635622544040477,-0.618977051328633,-0.603748925809969,-0.49973180882737,
-0.394912479224905,-0.290040790477003,-0.18575703861591,-0.0831547939216665,
0.),.UNSPECIFIED.);
#455=B_SPLINE_CURVE_WITH_KNOTS('',3,(#27264,#27265,#27266,#27267,#27268,
#27269,#27270,#27271,#27272,#27273,#27274,#27275,#27276,#27277,#27278,#27279,
#27280,#27281,#27282,#27283,#27284,#27285,#27286,#27287,#27288,#27289,#27290,
#27291,#27292,#27293,#27294,#27295,#27296,#27297,#27298,#27299,#27300,#27301,
#27302,#27303,#27304,#27305,#27306,#27307,#27308,#27309,#27310,#27311,#27312,
#27313,#27314,#27315,#27316,#27317,#27318,#27319,#27320,#27321,#27322,#27323,
#27324,#27325,#27326,#27327,#27328,#27329,#27330,#27331,#27332,#27333,#27334,
#27335,#27336,#27337,#27338,#27339,#27340,#27341,#27342,#27343,#27344,#27345,
#27346,#27347,#27348,#27349,#27350,#27351,#27352,#27353,#27354,#27355,#27356,
#27357,#27358,#27359,#27360,#27361,#27362,#27363,#27364,#27365,#27366,#27367,
#27368,#27369,#27370,#27371,#27372,#27373,#27374,#27375,#27376,#27377,#27378,
#27379,#27380,#27381,#27382,#27383,#27384,#27385,#27386,#27387,#27388,#27389,
#27390,#27391,#27392,#27393,#27394,#27395,#27396,#27397,#27398,#27399,#27400,
#27401,#27402),.UNSPECIFIED.,.F.,.F.,(4,3,3,3,3,3,3,3,3,3,3,3,3,3,3,3,3,
3,3,3,3,3,3,3,3,3,3,3,3,3,3,3,3,3,3,3,3,3,3,3,3,3,3,3,3,3,4),(-3.3351521949513,
-3.23035412220627,-3.17020330978756,-3.06579909218576,-2.98176387938634,
-2.9449984737866,-2.92915657616349,-2.91720620520155,-2.81251162890031,
-2.7071228788428,-2.60200290909517,-2.54988152926899,-2.52416540839213,
-2.50878246245602,-2.40282819474695,-2.39351738979045,-2.28862560733202,
-2.18281471664314,-2.07663992389392,-1.97072839078126,-1.92506933135162,
-1.90124417079794,-1.8893117349777,-1.78281482245468,-1.67586957667813,
-1.60545591534413,-1.49883052806521,-1.39193067774417,-1.31887193544069,
-1.28690873568292,-1.27388989384833,-1.26361386894611,-1.15708585888843,
-1.04940938788384,-0.941663866948425,-0.834628763436338,-0.807460739316361,
-0.706528146901816,-0.662370137720452,-0.64258228962385,-0.631550073319128,
-0.524780997969994,-0.416884173936585,-0.308312901558949,-0.200010753330189,
-0.0930669769078746,0.),.UNSPECIFIED.);
#456=B_SPLINE_CURVE_WITH_KNOTS('',3,(#27409,#27410,#27411,#27412,#27413,
#27414),.UNSPECIFIED.,.F.,.F.,(4,2,4),(2.90070768857401,3.00706665159486,
3.1886726077324),.UNSPECIFIED.);
#457=B_SPLINE_CURVE_WITH_KNOTS('',3,(#27417,#27418,#27419,#27420,#27421,
#27422),.UNSPECIFIED.,.F.,.F.,(4,2,4),(3.1886726077324,3.37027856386994,
3.4766375268908),.UNSPECIFIED.);
#458=B_SPLINE_CURVE_WITH_KNOTS('',3,(#27435,#27436,#27437,#27438,#27439,
#27440,#27441,#27442,#27443,#27444,#27445,#27446,#27447,#27448,#27449,#27450,
#27451,#27452,#27453,#27454,#27455,#27456,#27457,#27458,#27459,#27460,#27461,
#27462,#27463,#27464,#27465,#27466,#27467,#27468,#27469,#27470,#27471,#27472,
#27473,#27474,#27475,#27476,#27477,#27478,#27479,#27480,#27481,#27482,#27483,
#27484,#27485,#27486,#27487,#27488,#27489,#27490,#27491,#27492,#27493,#27494,
#27495,#27496,#27497,#27498,#27499,#27500,#27501,#27502,#27503,#27504,#27505,
#27506,#27507,#27508,#27509,#27510,#27511,#27512,#27513,#27514,#27515,#27516,
#27517,#27518,#27519,#27520,#27521,#27522,#27523,#27524,#27525,#27526,#27527,
#27528,#27529,#27530,#27531,#27532,#27533,#27534,#27535,#27536,#27537,#27538,
#27539,#27540,#27541,#27542,#27543,#27544,#27545,#27546,#27547,#27548,#27549,
#27550,#27551,#27552,#27553,#27554,#27555,#27556,#27557,#27558,#27559,#27560,
#27561,#27562,#27563,#27564,#27565,#27566,#27567,#27568,#27569,#27570,#27571,
#27572,#27573),.UNSPECIFIED.,.F.,.F.,(4,3,3,3,3,3,3,3,3,3,3,3,3,3,3,3,3,
3,3,3,3,3,3,3,3,3,3,3,3,3,3,3,3,3,3,3,3,3,3,3,3,3,3,3,3,3,4),(-3.3351521949513,
-3.23035412240041,-3.17020330978753,-3.06579909250646,-2.98176387966696,
-2.94499847404967,-2.92915657746123,-2.9172062091037,-2.81251163327298,
-2.70712288308388,-2.60200291309312,-2.54988153226745,-2.52416540972209,
-2.50878246249469,-2.40282819474078,-2.39351738979045,-2.28862560698356,
-2.18281471621706,-2.07663992322332,-1.97072838921362,-1.92506932997993,
-1.90124416858194,-1.88931173446478,-1.78281482187671,-1.67586957561123,
-1.60545591534413,-1.49883052685415,-1.39193067699312,-1.31887193478353,
-1.28690873506683,-1.27388989154254,-1.26361386703925,-1.15708585497168,
-1.04940938370439,-0.941663864345138,-0.834628765543497,-0.807460739316348,
-0.706528146901805,-0.662370137720442,-0.642582289491659,-0.631550074280081,
-0.524781005409625,-0.41688418584941,-0.308312912995514,-0.200010761086136,
-0.0930669761911965,0.),.UNSPECIFIED.);
#459=B_SPLINE_CURVE_WITH_KNOTS('',3,(#27576,#27577,#27578,#27579,#27580,
#27581,#27582,#27583,#27584,#27585,#27586,#27587,#27588,#27589,#27590,#27591,
#27592,#27593,#27594,#27595,#27596,#27597,#27598,#27599,#27600,#27601,#27602,
#27603,#27604,#27605,#27606,#27607,#27608,#27609,#27610,#27611,#27612,#27613,
#27614,#27615,#27616,#27617,#27618,#27619,#27620,#27621,#27622,#27623,#27624,
#27625,#27626,#27627,#27628,#27629,#27630,#27631,#27632,#27633,#27634,#27635,
#27636,#27637,#27638,#27639,#27640,#27641,#27642,#27643,#27644,#27645,#27646,
#27647,#27648,#27649,#27650,#27651,#27652,#27653,#27654,#27655,#27656,#27657,
#27658,#27659,#27660,#27661,#27662,#27663,#27664,#27665,#27666,#27667,#27668,
#27669,#27670,#27671,#27672,#27673,#27674,#27675,#27676,#27677,#27678,#27679,
#27680,#27681,#27682,#27683,#27684,#27685,#27686,#27687,#27688,#27689,#27690,
#27691,#27692,#27693,#27694,#27695,#27696,#27697,#27698,#27699,#27700,#27701,
#27702,#27703,#27704,#27705,#27706,#27707,#27708,#27709,#27710,#27711,#27712,
#27713,#27714),.UNSPECIFIED.,.F.,.F.,(4,3,3,3,3,3,3,3,3,3,3,3,3,3,3,3,3,
3,3,3,3,3,3,3,3,3,3,3,3,3,3,3,3,3,3,3,3,3,3,3,3,3,3,3,3,3,4),(-3.33140537617985,
-3.22326787425814,-3.15817079917634,-3.0498533014283,-2.96298085616642,
-2.92497416136434,-2.90862147116675,-2.8960551743525,-2.78842365887399,
-2.6800361789888,-2.5729086860616,-2.51839994937951,-2.48953284992468,-2.47285249229225,
-2.36566522904863,-2.35487373933324,-2.24815410347614,-2.14082940659152,
-2.03352875103554,-1.92687843770874,-1.88101360335389,-1.85784780192153,
-1.84418934498894,-1.73779564875492,-1.63148467770906,-1.55995976286992,
-1.45341767352125,-1.34699981034086,-1.27548160266394,-1.24419238680529,
-1.23174197960383,-1.22128582242241,-1.11610232056299,-1.01033276385257,
-0.904839738472552,-0.800449755260466,-0.774854148925471,-0.677997380309787,
-0.635622544040425,-0.618977051412567,-0.603748926550004,-0.49973180431923,
-0.394912472330862,-0.290040786684448,-0.18575704090222,-0.0831548060731709,
0.),.UNSPECIFIED.);
#460=B_SPLINE_CURVE_WITH_KNOTS('',3,(#28263,#28264,#28265,#28266),
 .UNSPECIFIED.,.F.,.F.,(4,4),(63.95798063707,63.9837703781121),
 .UNSPECIFIED.);
#461=B_SPLINE_CURVE_WITH_KNOTS('',3,(#28267,#28268,#28269,#28270,#28271,
#28272,#28273,#28274,#28275,#28276,#28277,#28278,#28279,#28280,#28281),
 .UNSPECIFIED.,.F.,.F.,(4,1,1,1,1,1,1,1,1,1,1,1,4),(10.376176187289,10.7636241331782,
11.2566188807148,11.7496136282514,12.242608375788,12.7356031233247,13.2285978708613,
13.7215926183979,14.2145873659345,14.7075821134711,15.2005768610077,15.6935716085443,
15.7079632679489),.UNSPECIFIED.);
#462=B_SPLINE_CURVE_WITH_KNOTS('',3,(#28283,#28284,#28285,#28286,#28287,
#28288,#28289,#28290,#28291,#28292,#28293,#28294),.UNSPECIFIED.,.F.,.F.,
(4,1,1,1,1,1,1,1,1,4),(11.6149723878394,12.107967135376,12.6009618829127,
13.0939566304493,13.5869513779859,14.0799461255225,14.5729408730591,15.0659356205957,
15.5589303681323,15.7079632679489),.UNSPECIFIED.);
#463=B_SPLINE_CURVE_WITH_KNOTS('',3,(#29658,#29659,#29660,#29661,#29662,
#29663,#29664,#29665,#29666,#29667,#29668,#29669,#29670,#29671,#29672,#29673,
#29674,#29675,#29676,#29677,#29678,#29679,#29680,#29681,#29682,#29683,#29684,
#29685,#29686,#29687,#29688,#29689,#29690,#29691,#29692,#29693,#29694,#29695,
#29696,#29697,#29698,#29699,#29700,#29701,#29702,#29703,#29704,#29705,#29706,
#29707,#29708,#29709,#29710,#29711,#29712,#29713,#29714,#29715,#29716,#29717,
#29718,#29719,#29720,#29721,#29722,#29723,#29724,#29725,#29726,#29727,#29728,
#29729,#29730,#29731,#29732,#29733,#29734,#29735,#29736,#29737,#29738,#29739,
#29740,#29741,#29742,#29743,#29744,#29745,#29746,#29747,#29748,#29749,#29750,
#29751,#29752,#29753,#29754,#29755,#29756,#29757,#29758,#29759,#29760,#29761,
#29762,#29763,#29764,#29765,#29766,#29767,#29768,#29769,#29770,#29771,#29772,
#29773,#29774,#29775,#29776,#29777,#29778,#29779,#29780,#29781,#29782,#29783,
#29784,#29785,#29786,#29787,#29788,#29789,#29790,#29791,#29792,#29793),
 .UNSPECIFIED.,.F.,.F.,(4,3,3,3,3,3,3,3,3,3,3,3,3,3,3,3,3,3,3,3,3,3,3,3,
3,3,3,3,3,3,3,3,3,3,3,3,3,3,3,3,3,3,3,3,3,4),(-4.26859401472304,-4.13873007688789,
-4.08850162055165,-3.95858584619281,-3.82847709951256,-3.73149748136453,
-3.71631594412289,-3.58696529636488,-3.45338401085574,-3.32450556188697,
-3.19666996642904,-3.18303474098074,-3.05264015432834,-2.92417890259064,
-2.79512825168043,-2.6658735005123,-2.53709505709189,-2.4090588279256,-2.39050563042798,
-2.3791326398393,-2.36740010056182,-2.23913691627976,-2.11091291541336,
-2.0249501404267,-1.89655785726426,-1.76815488394767,-1.67303375966788,
-1.58980277592306,-1.57904949215431,-1.45212314108153,-1.32439228312005,
-1.19687411471462,-1.07054011091882,-1.00718588970934,-0.881287653495677,
-0.826207175152197,-0.798981472708049,-0.78720874403541,-0.775317236286388,
-0.649547843460037,-0.522822362146257,-0.392116771609693,-0.26578478676463,
-0.140456274469436,-0.0170309231504542,0.),.UNSPECIFIED.);
#464=B_SPLINE_CURVE_WITH_KNOTS('',3,(#29794,#29795,#29796,#29797,#29798,
#29799,#29800,#29801,#29802,#29803,#29804,#29805,#29806,#29807,#29808,#29809),
 .UNSPECIFIED.,.F.,.F.,(4,3,3,3,3,4),(95.373907172968,95.5887530958692,
96.0866111849102,96.5844692739512,97.0823273629921,97.4940920164032),
 .UNSPECIFIED.);
#465=B_SPLINE_CURVE_WITH_KNOTS('',3,(#29811,#29812,#29813,#29814,#29815,
#29816,#29817,#29818,#29819,#29820,#29821,#29822,#29823,#29824,#29825,#29826,
#29827,#29828,#29829,#29830,#29831,#29832,#29833,#29834,#29835,#29836,#29837,
#29838,#29839,#29840,#29841,#29842,#29843,#29844,#29845,#29846,#29847,#29848,
#29849,#29850,#29851,#29852,#29853,#29854,#29855,#29856,#29857,#29858,#29859,
#29860,#29861,#29862,#29863,#29864,#29865,#29866,#29867,#29868,#29869,#29870,
#29871,#29872,#29873,#29874,#29875,#29876,#29877,#29878,#29879,#29880,#29881,
#29882,#29883,#29884,#29885,#29886,#29887,#29888,#29889,#29890,#29891,#29892,
#29893,#29894,#29895,#29896,#29897,#29898,#29899,#29900,#29901,#29902,#29903,
#29904,#29905,#29906,#29907,#29908,#29909,#29910,#29911,#29912,#29913,#29914,
#29915,#29916,#29917,#29918,#29919,#29920,#29921,#29922,#29923,#29924,#29925,
#29926,#29927,#29928,#29929,#29930,#29931,#29932,#29933,#29934,#29935,#29936,
#29937,#29938,#29939,#29940),.UNSPECIFIED.,.F.,.F.,(4,3,3,3,3,3,3,3,3,3,
3,3,3,3,3,3,3,3,3,3,3,3,3,3,3,3,3,3,3,3,3,3,3,3,3,3,3,3,3,3,3,3,3,4),(-4.27233968854161,
-4.14561602726014,-4.09907448469013,-3.97290709741126,-3.84621089191813,
-3.749773654366,-3.73627839431146,-3.60966162132612,-3.47994220953063,-3.35296282839602,
-3.22187340127008,-3.20970027001722,-3.09078397414414,-2.96324940449412,
-2.83568998921265,-2.70759606171859,-2.57963130546553,-2.45235033333514,
-2.43126259133011,-2.41607773241749,-2.28771734257599,-2.15890271920814,
-2.07050741694398,-1.94169654380679,-1.81290382296933,-1.71629339907897,
-1.63175927817491,-1.62010485283798,-1.49191166190089,-1.36241267866765,
-1.23282152109643,-1.10403428197821,-1.04002043184644,-0.910017877865636,
-0.853141760499034,-0.824352398485974,-0.813502334414714,-0.685266483128497,
-0.555745255190819,-0.425490911420356,-0.295356067993986,-0.165943780746531,
-0.0382708826685432,0.),.UNSPECIFIED.);
#466=B_SPLINE_CURVE_WITH_KNOTS('',3,(#29941,#29942,#29943,#29944,#29945,
#29946,#29947,#29948,#29949,#29950,#29951,#29952,#29953,#29954),
 .UNSPECIFIED.,.F.,.F.,(4,1,1,1,1,1,1,1,1,1,1,4),(10.376176187289,10.7879408407,
11.285798929741,11.783657018782,12.281515107823,12.779373196864,13.277231285905,
13.7750893749459,14.2729474639869,14.7708055530279,15.2686636420689,15.7079632679489),
 .UNSPECIFIED.);
#467=B_SPLINE_CURVE_WITH_KNOTS('',3,(#29960,#29961,#29962,#29963,#29964,
#29965,#29966,#29967,#29968,#29969,#29970,#29971,#29972,#29973,#29974,#29975,
#29976,#29977,#29978,#29979,#29980,#29981,#29982,#29983,#29984,#29985,#29986,
#29987,#29988,#29989,#29990,#29991,#29992,#29993,#29994,#29995,#29996,#29997,
#29998,#29999,#30000,#30001,#30002,#30003,#30004,#30005,#30006,#30007,#30008,
#30009,#30010,#30011,#30012,#30013,#30014,#30015,#30016,#30017,#30018,#30019,
#30020,#30021,#30022,#30023,#30024,#30025,#30026,#30027,#30028,#30029,#30030,
#30031,#30032,#30033,#30034,#30035,#30036,#30037,#30038,#30039,#30040,#30041,
#30042,#30043,#30044,#30045,#30046,#30047,#30048,#30049,#30050,#30051,#30052,
#30053,#30054,#30055,#30056,#30057,#30058,#30059,#30060,#30061,#30062,#30063,
#30064,#30065,#30066,#30067,#30068,#30069,#30070,#30071,#30072,#30073,#30074,
#30075,#30076,#30077,#30078,#30079,#30080,#30081,#30082,#30083,#30084,#30085,
#30086,#30087,#30088,#30089,#30090,#30091,#30092,#30093,#30094,#30095),
 .UNSPECIFIED.,.F.,.F.,(4,3,3,3,3,3,3,3,3,3,3,3,3,3,3,3,3,3,3,3,3,3,3,3,
3,3,3,3,3,3,3,3,3,3,3,3,3,3,3,3,3,3,3,3,3,4),(-4.26859401472303,-4.13873007862848,
-4.08850162055171,-3.95858584686358,-3.82847709974972,-3.73149748157205,
-3.71631594239557,-3.58696529527702,-3.45338401003986,-3.32450556087226,
-3.19666996624169,-3.18303474029221,-3.05264015432835,-2.92417890259064,
-2.7951282517208,-2.66587349878086,-2.53709505009457,-2.4090588226776,-2.39050561977311,
-2.37913262630794,-2.36740009695194,-2.23913691213895,-2.11091290702005,
-2.02495014042667,-1.89655785461699,-1.76815488608368,-1.67303376153689,
-1.58980277755845,-1.57904949311201,-1.4521231353151,-1.32439227972488,
-1.19687412089341,-1.07054013824695,-1.00718588970937,-0.881287653495698,
-0.826207175152217,-0.798981472541323,-0.78720874864497,-0.775317237411105,
-0.64954786276476,-0.522822391081097,-0.392116793310822,-0.265784790792495,
-0.140456252484584,-0.0170308663221606,0.),.UNSPECIFIED.);
#468=B_SPLINE_CURVE_WITH_KNOTS('',3,(#30098,#30099,#30100,#30101,#30102,
#30103,#30104,#30105,#30106,#30107,#30108,#30109),.UNSPECIFIED.,.F.,.F.,
(4,1,1,1,1,1,1,1,1,4),(11.6149723878395,12.1128304768804,12.6106885659214,
13.1085466549624,13.6064047440034,14.1042628330444,14.6021209220854,15.0999790111264,
15.5978371001673,15.7079632679489),.UNSPECIFIED.);
#469=B_SPLINE_CURVE_WITH_KNOTS('',3,(#30923,#30924,#30925,#30926,#30927,
#30928,#30929,#30930,#30931,#30932,#30933,#30934,#30935,#30936,#30937,#30938,
#30939,#30940,#30941,#30942,#30943,#30944,#30945,#30946,#30947,#30948,#30949,
#30950,#30951,#30952,#30953,#30954,#30955,#30956,#30957,#30958,#30959,#30960,
#30961,#30962,#30963,#30964,#30965,#30966,#30967,#30968,#30969,#30970,#30971,
#30972,#30973,#30974,#30975,#30976,#30977,#30978,#30979,#30980,#30981,#30982,
#30983,#30984,#30985,#30986,#30987,#30988,#30989,#30990,#30991,#30992,#30993,
#30994,#30995,#30996,#30997,#30998,#30999,#31000,#31001,#31002,#31003,#31004,
#31005,#31006,#31007,#31008,#31009,#31010,#31011,#31012,#31013,#31014,#31015,
#31016,#31017,#31018,#31019,#31020,#31021,#31022,#31023,#31024,#31025,#31026,
#31027,#31028,#31029,#31030,#31031,#31032,#31033,#31034,#31035,#31036,#31037,
#31038,#31039,#31040,#31041,#31042,#31043,#31044,#31045,#31046,#31047,#31048,
#31049,#31050,#31051,#31052),.UNSPECIFIED.,.F.,.F.,(4,3,3,3,3,3,3,3,3,3,
3,3,3,3,3,3,3,3,3,3,3,3,3,3,3,3,3,3,3,3,3,3,3,3,3,3,3,3,3,3,3,3,3,4),(-4.27233968854153,
-4.14561602839147,-4.09907448469005,-3.97290709931656,-3.84621089389475,
-3.74977366118721,-3.73627840644343,-3.60966163550516,-3.47994222016488,
-3.35296283800287,-3.22187340607345,-3.2097002822526,-3.09078397414404,
-2.96324940449404,-2.83568998898437,-2.70759606104771,-2.57963130228954,
-2.45235033095315,-2.43126258472487,-2.41607773095023,-2.28771734093045,
-2.15890271577605,-2.07050741694398,-1.94169654380679,-1.81290382315168,
-1.71629339923853,-1.63175927831451,-1.62010485805667,-1.49191165955653,
-1.36241267466591,-1.2328215214719,-1.10403429784844,-1.04002043184644,
-0.910017877865632,-0.85314176049903,-0.824352398286953,-0.813502334914016,
-0.685266505329869,-0.555745292861926,-0.425490955509816,-0.295356101878412,
-0.165943794724452,-0.0382708649850161,0.),.UNSPECIFIED.);
#470=B_SPLINE_CURVE_WITH_KNOTS('',3,(#31053,#31054,#31055,#31056,#31057,
#31058,#31059,#31060,#31061,#31062),.UNSPECIFIED.,.F.,.F.,(4,3,3,4),(-99.571617808197,
-99.0737597191561,-98.5759016301151,-98.3407704878033),.UNSPECIFIED.);
#471=B_SPLINE_CURVE_WITH_KNOTS('',3,(#31066,#31067,#31068,#31069,#31070,
#31071),.UNSPECIFIED.,.F.,.F.,(4,2,4),(0.,0.152964636529855,0.281059164612023),
 .UNSPECIFIED.);
#472=B_SPLINE_CURVE_WITH_KNOTS('',3,(#31075,#31076,#31077,#31078,#31079,
#31080,#31081,#31082,#31083,#31084),.UNSPECIFIED.,.F.,.F.,(4,2,2,2,4),(0.0909639115113299,
0.113933562624914,0.136903213738499,0.159492703061009,0.182082192383519),
 .UNSPECIFIED.);
#473=B_SPLINE_CURVE_WITH_KNOTS('',3,(#31090,#31091,#31092,#31093,#31094,
#31095),.UNSPECIFIED.,.F.,.F.,(4,2,4),(0.57279622617395,0.700890754256119,
0.853855390785973),.UNSPECIFIED.);
#474=B_SPLINE_CURVE_WITH_KNOTS('',3,(#31099,#31100,#31101,#31102,#31103,
#31104,#31105,#31106,#31107,#31108),.UNSPECIFIED.,.F.,.F.,(4,2,2,2,4),(0.,
0.036890778159456,0.073781556318912,0.147563112637824,0.287928080070797),
 .UNSPECIFIED.);
#475=B_SPLINE_CURVE_WITH_KNOTS('',3,(#31109,#31110,#31111,#31112,#31113,
#31114,#31115,#31116),.UNSPECIFIED.,.F.,.F.,(4,2,2,4),(-1.22072109304768,
-1.09399903701061,-0.96727698097355,-0.914517589488587),.UNSPECIFIED.);
#476=B_SPLINE_CURVE_WITH_KNOTS('',3,(#31118,#31119,#31120,#31121,#31122,
#31123,#31124,#31125),.UNSPECIFIED.,.F.,.F.,(4,2,2,4),(-0.306203503559089,
-0.253444112074126,-0.126722056037063,0.),.UNSPECIFIED.);
#477=B_SPLINE_CURVE_WITH_KNOTS('',3,(#31127,#31128,#31129,#31130,#31131,
#31132,#31133,#31134,#31135,#31136),.UNSPECIFIED.,.F.,.F.,(4,2,2,2,4),(-0.287928080070797,
-0.147563112637824,-0.0737815563189121,-0.0368907781594561,0.),
 .UNSPECIFIED.);
#478=B_SPLINE_CURVE_WITH_KNOTS('',3,(#31144,#31145,#31146,#31147,#31148,
#31149,#31150,#31151,#31152,#31153),.UNSPECIFIED.,.F.,.F.,(4,2,2,2,4),(0.182082136548056,
0.204671625870566,0.227261115193076,0.25023076630666,0.273200417420245),
 .UNSPECIFIED.);
#479=B_SPLINE_CURVE_WITH_KNOTS('',3,(#31158,#31159,#31160,#31161,#31162,
#31163,#31164,#31165,#31166,#31167),.UNSPECIFIED.,.F.,.F.,(4,2,2,2,4),(0.182082136548057,
0.204766091123424,0.22745004569879,0.250325299199413,0.267311238580278),
 .UNSPECIFIED.);
#480=B_SPLINE_CURVE_WITH_KNOTS('',3,(#31174,#31175,#31176,#31177,#31178,
#31179,#31180,#31181,#31182,#31183),.UNSPECIFIED.,.F.,.F.,(4,2,2,2,4),(0.0968538675768226,
0.113933506789453,0.136903157903037,0.159492647225547,0.182082136548057),
 .UNSPECIFIED.);
#481=B_SPLINE_CURVE_WITH_KNOTS('',3,(#31213,#31214,#31215,#31216,#31217,
#31218,#31219,#31220,#31221,#31222,#31223,#31224,#31225,#31226,#31227,#31228,
#31229,#31230,#31231,#31232,#31233,#31234,#31235,#31236,#31237,#31238,#31239),
 .UNSPECIFIED.,.F.,.F.,(4,2,2,2,2,2,3,2,2,2,2,2,4),(5.99649261281881,6.24600544998076,
6.4955182871427,6.99454396146659,7.4949337226125,7.74512860318546,7.99532348375842,
8.24551836433138,8.49571324490433,8.99610300605025,9.49512868037414,9.74464151753608,
9.99415435469802),.UNSPECIFIED.);
#482=B_SPLINE_CURVE_WITH_KNOTS('',3,(#31240,#31241,#31242,#31243,#31244,
#31245,#31246,#31247,#31248,#31249,#31250,#31251,#31252,#31253,#31254,#31255,
#31256,#31257,#31258,#31259,#31260,#31261,#31262,#31263,#31264,#31265),
 .UNSPECIFIED.,.F.,.F.,(4,2,2,2,2,2,2,2,2,2,2,2,4),(9.99415435469802,10.24366719186,
10.4931800290219,10.9922057033458,11.4925954644917,11.7427903450647,11.9929852256376,
12.2431801062106,12.4933749867835,12.9937647479295,13.4927904222533,13.7423032594153,
13.9918160965772),.UNSPECIFIED.);
#483=B_SPLINE_CURVE_WITH_KNOTS('',3,(#31267,#31268,#31269,#31270,#31271,
#31272,#31273,#31274,#31275,#31276,#31277,#31278,#31279,#31280,#31281,#31282,
#31283,#31284,#31285,#31286,#31287,#31288,#31289,#31290,#31291,#31292,#31293,
#31294,#31295,#31296,#31297),.UNSPECIFIED.,.F.,.F.,(4,2,2,2,2,2,2,2,2,2,
2,3,2,2,4),(1.95850633937799,2.2855721728953,2.6667178301167,3.04786348733809,
3.42900914455948,3.81015480178088,4.19097501639401,4.57179523100713,4.95261544562026,
5.33343566023339,5.71458131745479,6.09572697467618,6.47687263189757,6.85801828911897,
7.18508412263628),.UNSPECIFIED.);
#484=B_SPLINE_CURVE_WITH_KNOTS('',3,(#32149,#32150,#32151,#32152,#32153,
#32154,#32155,#32156,#32157,#32158,#32159,#32160,#32161,#32162,#32163,#32164,
#32165,#32166,#32167,#32168,#32169,#32170,#32171,#32172,#32173,#32174,#32175,
#32176,#32177,#32178,#32179,#32180,#32181,#32182,#32183,#32184,#32185,#32186,
#32187,#32188,#32189,#32190,#32191,#32192,#32193,#32194,#32195,#32196,#32197,
#32198,#32199,#32200,#32201,#32202,#32203,#32204,#32205,#32206,#32207,#32208,
#32209,#32210,#32211,#32212,#32213,#32214,#32215,#32216,#32217,#32218,#32219,
#32220,#32221,#32222,#32223),.UNSPECIFIED.,.F.,.F.,(4,1,1,1,1,1,1,1,1,1,
1,1,1,1,1,1,1,1,1,1,1,1,1,1,1,1,1,1,1,1,1,1,1,1,1,1,1,1,1,1,1,1,1,1,1,1,
1,1,1,1,1,1,1,1,1,1,1,1,1,1,1,1,1,1,1,1,1,1,1,1,1,1,4),(0.,0.00892857142857143,
0.0178571428571429,0.0357142857142857,0.0535714285714286,0.0714285714285714,
0.0892857142857143,0.107142857142857,0.116071428571429,0.125,0.133928571428571,
0.142857142857143,0.154761904761905,0.166666666666667,0.178571428571429,
0.19047619047619,0.202380952380952,0.214285714285714,0.232142857142857,
0.25,0.267857142857143,0.285714285714286,0.303571428571429,0.321428571428571,
0.339285714285714,0.357142857142857,0.376984126984127,0.380952380952381,
0.392857142857143,0.404761904761905,0.416666666666667,0.428571428571429,
0.44047619047619,0.452380952380952,0.464285714285714,0.476190476190476,
0.492063492063492,0.5,0.517857142857143,0.535714285714286,0.553571428571429,
0.571428571428571,0.589285714285714,0.607142857142857,0.625,0.642857142857143,
0.654761904761905,0.666666666666667,0.678571428571428,0.69047619047619,
0.702380952380952,0.714285714285714,0.726190476190476,0.738095238095238,
0.75,0.761904761904762,0.773809523809524,0.785714285714286,0.797619047619047,
0.809523809523809,0.821428571428571,0.833333333333333,0.845238095238095,
0.857142857142857,0.875,0.892857142857143,0.910714285714286,0.928571428571429,
0.946428571428571,0.964285714285714,0.982142857142857,0.991071428571429,
1.),.UNSPECIFIED.);
#485=B_SPLINE_CURVE_WITH_KNOTS('',2,(#32438,#32439,#32440),
 .UNSPECIFIED.,.F.,.F.,(3,3),(0.,1.),.UNSPECIFIED.);
#486=B_SPLINE_CURVE_WITH_KNOTS('',2,(#32452,#32453,#32454),
 .UNSPECIFIED.,.F.,.F.,(3,3),(0.,1.),.UNSPECIFIED.);
#487=B_SPLINE_CURVE_WITH_KNOTS('',2,(#32456,#32457,#32458),
 .UNSPECIFIED.,.F.,.F.,(3,3),(0.,1.),.UNSPECIFIED.);
#488=B_SPLINE_CURVE_WITH_KNOTS('',2,(#32466,#32467,#32468),
 .UNSPECIFIED.,.F.,.F.,(3,3),(0.,1.),.UNSPECIFIED.);
#489=B_SPLINE_CURVE_WITH_KNOTS('',2,(#32470,#32471,#32472),
 .UNSPECIFIED.,.F.,.F.,(3,3),(0.,1.),.UNSPECIFIED.);
#490=B_SPLINE_CURVE_WITH_KNOTS('',2,(#32483,#32484,#32485),
 .UNSPECIFIED.,.F.,.F.,(3,3),(0.,1.),.UNSPECIFIED.);
#491=B_SPLINE_CURVE_WITH_KNOTS('',2,(#32504,#32505,#32506),
 .UNSPECIFIED.,.F.,.F.,(3,3),(0.,1.),.UNSPECIFIED.);
#492=B_SPLINE_CURVE_WITH_KNOTS('',2,(#32508,#32509,#32510),
 .UNSPECIFIED.,.F.,.F.,(3,3),(0.,1.),.UNSPECIFIED.);
#493=B_SPLINE_CURVE_WITH_KNOTS('',2,(#32512,#32513,#32514),
 .UNSPECIFIED.,.F.,.F.,(3,3),(0.,1.),.UNSPECIFIED.);
#494=B_SPLINE_CURVE_WITH_KNOTS('',2,(#32516,#32517,#32518),
 .UNSPECIFIED.,.F.,.F.,(3,3),(0.,1.),.UNSPECIFIED.);
#495=B_SPLINE_CURVE_WITH_KNOTS('',2,(#32520,#32521,#32522),
 .UNSPECIFIED.,.F.,.F.,(3,3),(0.,1.),.UNSPECIFIED.);
#496=B_SPLINE_CURVE_WITH_KNOTS('',2,(#32524,#32525,#32526),
 .UNSPECIFIED.,.F.,.F.,(3,3),(0.,1.),.UNSPECIFIED.);
#497=B_SPLINE_CURVE_WITH_KNOTS('',2,(#32528,#32529,#32530),
 .UNSPECIFIED.,.F.,.F.,(3,3),(0.,1.),.UNSPECIFIED.);
#498=B_SPLINE_CURVE_WITH_KNOTS('',2,(#32532,#32533,#32534),
 .UNSPECIFIED.,.F.,.F.,(3,3),(0.,1.),.UNSPECIFIED.);
#499=B_SPLINE_CURVE_WITH_KNOTS('',2,(#32536,#32537,#32538),
 .UNSPECIFIED.,.F.,.F.,(3,3),(0.,1.),.UNSPECIFIED.);
#500=B_SPLINE_CURVE_WITH_KNOTS('',2,(#32540,#32541,#32542),
 .UNSPECIFIED.,.F.,.F.,(3,3),(0.,1.),.UNSPECIFIED.);
#501=B_SPLINE_CURVE_WITH_KNOTS('',2,(#32544,#32545,#32546),
 .UNSPECIFIED.,.F.,.F.,(3,3),(0.,1.),.UNSPECIFIED.);
#502=B_SPLINE_CURVE_WITH_KNOTS('',2,(#32547,#32548,#32549),
 .UNSPECIFIED.,.F.,.F.,(3,3),(0.,1.),.UNSPECIFIED.);
#503=B_SPLINE_CURVE_WITH_KNOTS('',2,(#32552,#32553,#32554),
 .UNSPECIFIED.,.F.,.F.,(3,3),(0.,1.),.UNSPECIFIED.);
#504=B_SPLINE_CURVE_WITH_KNOTS('',2,(#32564,#32565,#32566),
 .UNSPECIFIED.,.F.,.F.,(3,3),(0.,1.),.UNSPECIFIED.);
#505=B_SPLINE_CURVE_WITH_KNOTS('',2,(#32568,#32569,#32570),
 .UNSPECIFIED.,.F.,.F.,(3,3),(0.,1.),.UNSPECIFIED.);
#506=B_SPLINE_CURVE_WITH_KNOTS('',2,(#32573,#32574,#32575),
 .UNSPECIFIED.,.F.,.F.,(3,3),(0.,1.),.UNSPECIFIED.);
#507=B_SPLINE_CURVE_WITH_KNOTS('',2,(#32578,#32579,#32580),
 .UNSPECIFIED.,.F.,.F.,(3,3),(0.,1.),.UNSPECIFIED.);
#508=B_SPLINE_CURVE_WITH_KNOTS('',2,(#32592,#32593,#32594),
 .UNSPECIFIED.,.F.,.F.,(3,3),(0.,1.),.UNSPECIFIED.);
#509=B_SPLINE_CURVE_WITH_KNOTS('',2,(#32596,#32597,#32598),
 .UNSPECIFIED.,.F.,.F.,(3,3),(0.,1.),.UNSPECIFIED.);
#510=B_SPLINE_CURVE_WITH_KNOTS('',2,(#32600,#32601,#32602),
 .UNSPECIFIED.,.F.,.F.,(3,3),(0.,1.),.UNSPECIFIED.);
#511=B_SPLINE_CURVE_WITH_KNOTS('',2,(#32604,#32605,#32606),
 .UNSPECIFIED.,.F.,.F.,(3,3),(0.,1.),.UNSPECIFIED.);
#512=B_SPLINE_CURVE_WITH_KNOTS('',2,(#32608,#32609,#32610),
 .UNSPECIFIED.,.F.,.F.,(3,3),(0.,1.),.UNSPECIFIED.);
#513=B_SPLINE_CURVE_WITH_KNOTS('',2,(#32612,#32613,#32614),
 .UNSPECIFIED.,.F.,.F.,(3,3),(0.,1.),.UNSPECIFIED.);
#514=B_SPLINE_CURVE_WITH_KNOTS('',2,(#32616,#32617,#32618),
 .UNSPECIFIED.,.F.,.F.,(3,3),(0.,1.),.UNSPECIFIED.);
#515=B_SPLINE_CURVE_WITH_KNOTS('',2,(#32620,#32621,#32622),
 .UNSPECIFIED.,.F.,.F.,(3,3),(0.,1.),.UNSPECIFIED.);
#516=B_SPLINE_CURVE_WITH_KNOTS('',2,(#32624,#32625,#32626),
 .UNSPECIFIED.,.F.,.F.,(3,3),(0.,1.),.UNSPECIFIED.);
#517=B_SPLINE_CURVE_WITH_KNOTS('',2,(#32628,#32629,#32630),
 .UNSPECIFIED.,.F.,.F.,(3,3),(0.,1.),.UNSPECIFIED.);
#518=B_SPLINE_CURVE_WITH_KNOTS('',2,(#32632,#32633,#32634),
 .UNSPECIFIED.,.F.,.F.,(3,3),(0.,1.),.UNSPECIFIED.);
#519=B_SPLINE_CURVE_WITH_KNOTS('',2,(#32638,#32639,#32640),
 .UNSPECIFIED.,.F.,.F.,(3,3),(0.,1.),.UNSPECIFIED.);
#520=B_SPLINE_CURVE_WITH_KNOTS('',2,(#32642,#32643,#32644),
 .UNSPECIFIED.,.F.,.F.,(3,3),(0.,1.),.UNSPECIFIED.);
#521=B_SPLINE_CURVE_WITH_KNOTS('',2,(#32646,#32647,#32648),
 .UNSPECIFIED.,.F.,.F.,(3,3),(0.,1.),.UNSPECIFIED.);
#522=B_SPLINE_CURVE_WITH_KNOTS('',2,(#32650,#32651,#32652),
 .UNSPECIFIED.,.F.,.F.,(3,3),(0.,1.),.UNSPECIFIED.);
#523=B_SPLINE_CURVE_WITH_KNOTS('',2,(#32654,#32655,#32656),
 .UNSPECIFIED.,.F.,.F.,(3,3),(0.,1.),.UNSPECIFIED.);
#524=B_SPLINE_CURVE_WITH_KNOTS('',2,(#32658,#32659,#32660),
 .UNSPECIFIED.,.F.,.F.,(3,3),(0.,1.),.UNSPECIFIED.);
#525=B_SPLINE_CURVE_WITH_KNOTS('',2,(#32662,#32663,#32664),
 .UNSPECIFIED.,.F.,.F.,(3,3),(0.,1.),.UNSPECIFIED.);
#526=B_SPLINE_CURVE_WITH_KNOTS('',2,(#32666,#32667,#32668),
 .UNSPECIFIED.,.F.,.F.,(3,3),(0.,1.),.UNSPECIFIED.);
#527=B_SPLINE_CURVE_WITH_KNOTS('',2,(#32670,#32671,#32672),
 .UNSPECIFIED.,.F.,.F.,(3,3),(0.,1.),.UNSPECIFIED.);
#528=B_SPLINE_CURVE_WITH_KNOTS('',2,(#32674,#32675,#32676),
 .UNSPECIFIED.,.F.,.F.,(3,3),(0.,1.),.UNSPECIFIED.);
#529=B_SPLINE_CURVE_WITH_KNOTS('',2,(#32677,#32678,#32679),
 .UNSPECIFIED.,.F.,.F.,(3,3),(0.,1.),.UNSPECIFIED.);
#530=B_SPLINE_CURVE_WITH_KNOTS('',2,(#32712,#32713,#32714),
 .UNSPECIFIED.,.F.,.F.,(3,3),(0.,1.),.UNSPECIFIED.);
#531=B_SPLINE_CURVE_WITH_KNOTS('',2,(#32724,#32725,#32726),
 .UNSPECIFIED.,.F.,.F.,(3,3),(0.,1.),.UNSPECIFIED.);
#532=B_SPLINE_CURVE_WITH_KNOTS('',2,(#32755,#32756,#32757),
 .UNSPECIFIED.,.F.,.F.,(3,3),(0.,1.),.UNSPECIFIED.);
#533=B_SPLINE_CURVE_WITH_KNOTS('',2,(#32766,#32767,#32768),
 .UNSPECIFIED.,.F.,.F.,(3,3),(0.,1.),.UNSPECIFIED.);
#534=B_SPLINE_CURVE_WITH_KNOTS('',2,(#32789,#32790,#32791),
 .UNSPECIFIED.,.F.,.F.,(3,3),(0.,1.),.UNSPECIFIED.);
#535=B_SPLINE_CURVE_WITH_KNOTS('',2,(#32800,#32801,#32802),
 .UNSPECIFIED.,.F.,.F.,(3,3),(0.,1.),.UNSPECIFIED.);
#536=B_SPLINE_CURVE_WITH_KNOTS('',2,(#32864,#32865,#32866),
 .UNSPECIFIED.,.F.,.F.,(3,3),(0.,1.),.UNSPECIFIED.);
#537=B_SPLINE_CURVE_WITH_KNOTS('',2,(#32876,#32877,#32878),
 .UNSPECIFIED.,.F.,.F.,(3,3),(0.,1.),.UNSPECIFIED.);
#538=B_SPLINE_CURVE_WITH_KNOTS('',2,(#32887,#32888,#32889),
 .UNSPECIFIED.,.F.,.F.,(3,3),(0.,1.),.UNSPECIFIED.);
#539=B_SPLINE_CURVE_WITH_KNOTS('',2,(#32898,#32899,#32900),
 .UNSPECIFIED.,.F.,.F.,(3,3),(0.,1.),.UNSPECIFIED.);
#540=B_SPLINE_CURVE_WITH_KNOTS('',2,(#32909,#32910,#32911),
 .UNSPECIFIED.,.F.,.F.,(3,3),(0.,1.),.UNSPECIFIED.);
#541=B_SPLINE_CURVE_WITH_KNOTS('',2,(#32920,#32921,#32922),
 .UNSPECIFIED.,.F.,.F.,(3,3),(0.,1.),.UNSPECIFIED.);
#542=B_SPLINE_CURVE_WITH_KNOTS('',2,(#32931,#32932,#32933),
 .UNSPECIFIED.,.F.,.F.,(3,3),(0.,1.),.UNSPECIFIED.);
#543=B_SPLINE_CURVE_WITH_KNOTS('',2,(#32942,#32943,#32944),
 .UNSPECIFIED.,.F.,.F.,(3,3),(0.,1.),.UNSPECIFIED.);
#544=B_SPLINE_CURVE_WITH_KNOTS('',2,(#32953,#32954,#32955),
 .UNSPECIFIED.,.F.,.F.,(3,3),(0.,1.),.UNSPECIFIED.);
#545=B_SPLINE_CURVE_WITH_KNOTS('',2,(#32964,#32965,#32966),
 .UNSPECIFIED.,.F.,.F.,(3,3),(0.,1.),.UNSPECIFIED.);
#546=B_SPLINE_CURVE_WITH_KNOTS('',2,(#32975,#32976,#32977),
 .UNSPECIFIED.,.F.,.F.,(3,3),(0.,1.),.UNSPECIFIED.);
#547=B_SPLINE_CURVE_WITH_KNOTS('',2,(#32984,#32985,#32986),
 .UNSPECIFIED.,.F.,.F.,(3,3),(0.,1.),.UNSPECIFIED.);
#548=B_SPLINE_CURVE_WITH_KNOTS('',2,(#32997,#32998,#32999),
 .UNSPECIFIED.,.F.,.F.,(3,3),(0.,1.),.UNSPECIFIED.);
#549=B_SPLINE_CURVE_WITH_KNOTS('',2,(#33009,#33010,#33011),
 .UNSPECIFIED.,.F.,.F.,(3,3),(0.,1.),.UNSPECIFIED.);
#550=B_SPLINE_CURVE_WITH_KNOTS('',2,(#33024,#33025,#33026),
 .UNSPECIFIED.,.F.,.F.,(3,3),(0.,1.),.UNSPECIFIED.);
#551=B_SPLINE_CURVE_WITH_KNOTS('',2,(#33035,#33036,#33037),
 .UNSPECIFIED.,.F.,.F.,(3,3),(0.,1.),.UNSPECIFIED.);
#552=B_SPLINE_CURVE_WITH_KNOTS('',2,(#33062,#33063,#33064),
 .UNSPECIFIED.,.F.,.F.,(3,3),(0.,1.),.UNSPECIFIED.);
#553=B_SPLINE_CURVE_WITH_KNOTS('',2,(#33074,#33075,#33076),
 .UNSPECIFIED.,.F.,.F.,(3,3),(0.,1.),.UNSPECIFIED.);
#554=B_SPLINE_CURVE_WITH_KNOTS('',2,(#33085,#33086,#33087),
 .UNSPECIFIED.,.F.,.F.,(3,3),(0.,1.),.UNSPECIFIED.);
#555=B_SPLINE_CURVE_WITH_KNOTS('',2,(#33096,#33097,#33098),
 .UNSPECIFIED.,.F.,.F.,(3,3),(0.,1.),.UNSPECIFIED.);
#556=B_SPLINE_CURVE_WITH_KNOTS('',2,(#33107,#33108,#33109),
 .UNSPECIFIED.,.F.,.F.,(3,3),(0.,1.),.UNSPECIFIED.);
#557=B_SPLINE_CURVE_WITH_KNOTS('',2,(#33118,#33119,#33120),
 .UNSPECIFIED.,.F.,.F.,(3,3),(0.,1.),.UNSPECIFIED.);
#558=B_SPLINE_CURVE_WITH_KNOTS('',2,(#33129,#33130,#33131),
 .UNSPECIFIED.,.F.,.F.,(3,3),(0.,1.),.UNSPECIFIED.);
#559=B_SPLINE_CURVE_WITH_KNOTS('',2,(#33140,#33141,#33142),
 .UNSPECIFIED.,.F.,.F.,(3,3),(0.,1.),.UNSPECIFIED.);
#560=B_SPLINE_CURVE_WITH_KNOTS('',2,(#33151,#33152,#33153),
 .UNSPECIFIED.,.F.,.F.,(3,3),(0.,1.),.UNSPECIFIED.);
#561=B_SPLINE_CURVE_WITH_KNOTS('',2,(#33162,#33163,#33164),
 .UNSPECIFIED.,.F.,.F.,(3,3),(0.,1.),.UNSPECIFIED.);
#562=B_SPLINE_CURVE_WITH_KNOTS('',2,(#33173,#33174,#33175),
 .UNSPECIFIED.,.F.,.F.,(3,3),(0.,1.),.UNSPECIFIED.);
#563=B_SPLINE_CURVE_WITH_KNOTS('',2,(#33184,#33185,#33186),
 .UNSPECIFIED.,.F.,.F.,(3,3),(0.,1.),.UNSPECIFIED.);
#564=B_SPLINE_CURVE_WITH_KNOTS('',2,(#33199,#33200,#33201),
 .UNSPECIFIED.,.F.,.F.,(3,3),(0.,1.),.UNSPECIFIED.);
#565=B_SPLINE_CURVE_WITH_KNOTS('',2,(#33210,#33211,#33212),
 .UNSPECIFIED.,.F.,.F.,(3,3),(0.,1.),.UNSPECIFIED.);
#566=B_SPLINE_CURVE_WITH_KNOTS('',2,(#33221,#33222,#33223),
 .UNSPECIFIED.,.F.,.F.,(3,3),(0.,1.),.UNSPECIFIED.);
#567=B_SPLINE_CURVE_WITH_KNOTS('',2,(#33232,#33233,#33234),
 .UNSPECIFIED.,.F.,.F.,(3,3),(0.,1.),.UNSPECIFIED.);
#568=B_SPLINE_CURVE_WITH_KNOTS('',2,(#33243,#33244,#33245),
 .UNSPECIFIED.,.F.,.F.,(3,3),(0.,1.),.UNSPECIFIED.);
#569=B_SPLINE_CURVE_WITH_KNOTS('',2,(#33254,#33255,#33256),
 .UNSPECIFIED.,.F.,.F.,(3,3),(0.,1.),.UNSPECIFIED.);
#570=B_SPLINE_CURVE_WITH_KNOTS('',2,(#33265,#33266,#33267),
 .UNSPECIFIED.,.F.,.F.,(3,3),(0.,1.),.UNSPECIFIED.);
#571=B_SPLINE_CURVE_WITH_KNOTS('',2,(#33276,#33277,#33278),
 .UNSPECIFIED.,.F.,.F.,(3,3),(0.,1.),.UNSPECIFIED.);
#572=B_SPLINE_CURVE_WITH_KNOTS('',2,(#33287,#33288,#33289),
 .UNSPECIFIED.,.F.,.F.,(3,3),(0.,1.),.UNSPECIFIED.);
#573=B_SPLINE_CURVE_WITH_KNOTS('',2,(#33298,#33299,#33300),
 .UNSPECIFIED.,.F.,.F.,(3,3),(0.,1.),.UNSPECIFIED.);
#574=B_SPLINE_CURVE_WITH_KNOTS('',2,(#33309,#33310,#33311),
 .UNSPECIFIED.,.F.,.F.,(3,3),(0.,1.),.UNSPECIFIED.);
#575=B_SPLINE_CURVE_WITH_KNOTS('',3,(#33394,#33395,#33396,#33397,#33398,
#33399,#33400,#33401,#33402,#33403,#33404,#33405,#33406,#33407,#33408,#33409),
 .UNSPECIFIED.,.F.,.F.,(4,3,3,3,3,4),(-4.0929908801096,-3.9700734175722,
-3.47381424037567,-2.97755506317915,-2.48129588598262,-2.07752579179387),
 .UNSPECIFIED.);
#576=B_SPLINE_CURVE_WITH_KNOTS('',3,(#33412,#33413,#33414,#33415,#33416,
#33417,#33418,#33419,#33420,#33421),.UNSPECIFIED.,.F.,.F.,(4,3,3,4),(0.,
0.496259177196522,0.992518354393046,1.12612756527419),.UNSPECIFIED.);
#577=B_SPLINE_CURVE_WITH_KNOTS('',3,(#33426,#33427,#33428,#33429,#33430,
#33431,#33432,#33433,#33434,#33435,#33436,#33437,#33438,#33439,#33440,#33441,
#33442,#33443,#33444,#33445,#33446,#33447,#33448,#33449,#33450,#33451,#33452,
#33453,#33454,#33455,#33456,#33457,#33458,#33459,#33460,#33461,#33462,#33463,
#33464,#33465),.UNSPECIFIED.,.F.,.F.,(4,3,3,3,3,3,3,3,3,3,3,3,3,4),(-10.3761761872891,
-9.92518354393049,-9.42892436673396,-8.93266518953744,-8.43640601234091,
-7.94014683514439,-7.44388765794787,-6.94762848075134,-6.45136930355482,
-5.95511012635829,-5.45885094916177,-4.96259177196524,-4.46633259476872,
-4.0929908801096),.UNSPECIFIED.);
#578=B_SPLINE_CURVE_WITH_KNOTS('',3,(#33466,#33467,#33468,#33469,#33470,
#33471,#33472,#33473,#33474,#33475,#33476,#33477,#33478,#33479,#33480,#33481,
#33482,#33483,#33484,#33485,#33486,#33487,#33488,#33489,#33490,#33491,#33492,
#33493,#33494,#33495,#33496,#33497,#33498,#33499,#33500,#33501,#33502,#33503,
#33504,#33505),.UNSPECIFIED.,.F.,.F.,(4,3,3,3,3,3,3,3,3,3,3,3,3,4),(1.12612756527419,
1.48877753158957,1.9850367087861,2.48129588598262,2.97755506317914,3.47381424037567,
3.97007341757219,4.46633259476871,4.96259177196524,5.45885094916176,5.95511012635829,
6.45136930355481,6.94762848075133,7.40931287245371),.UNSPECIFIED.);
#579=B_SPLINE_CURVE_WITH_KNOTS('',3,(#33510,#33511,#33512,#33513,#33514,
#33515,#33516,#33517,#33518,#33519,#33520,#33521,#33522,#33523,#33524,#33525,
#33526,#33527,#33528,#33529,#33530,#33531,#33532,#33533,#33534,#33535,#33536,
#33537,#33538,#33539,#33540,#33541,#33542,#33543,#33544,#33545,#33546,#33547,
#33548,#33549,#33550,#33551,#33552),.UNSPECIFIED.,.F.,.F.,(4,3,3,3,3,3,
3,3,3,3,3,3,3,3,4),(-16.6593614944688,-16.3765528474853,-15.8802936702888,
-15.3840344930923,-14.8877753158957,-14.3915161386992,-13.8952569615027,
-13.3989977843062,-12.9027386071096,-12.4064794299131,-11.9102202527166,
-11.4139610755201,-10.9177018983235,-10.421442721127,-10.3761761872891),
 .UNSPECIFIED.);
#580=B_SPLINE_CURVE_WITH_KNOTS('',3,(#33553,#33554,#33555,#33556,#33557,
#33558,#33559,#33560,#33561,#33562,#33563,#33564,#33565,#33566,#33567,#33568,
#33569,#33570,#33571,#33572,#33573,#33574,#33575,#33576,#33577,#33578,#33579,
#33580,#33581,#33582,#33583,#33584,#33585,#33586,#33587,#33588,#33589,#33590,
#33591,#33592,#33593,#33594,#33595),.UNSPECIFIED.,.F.,.F.,(4,3,3,3,3,3,
3,3,3,3,3,3,3,3,4),(7.40931287245371,7.44388765794786,7.94014683514438,
8.43640601234091,8.93266518953743,9.42892436673395,9.92518354393048,10.421442721127,
10.9177018983235,11.41396107552,11.9102202527166,12.4064794299131,12.9027386071096,
13.3989977843061,13.6924981796334),.UNSPECIFIED.);
#581=B_SPLINE_CURVE_WITH_KNOTS('',3,(#33600,#33601,#33602,#33603,#33604,
#33605,#33606,#33607,#33608,#33609,#33610,#33611,#33612,#33613,#33614,#33615,
#33616,#33617,#33618,#33619,#33620,#33621,#33622,#33623,#33624,#33625,#33626,
#33627,#33628,#33629,#33630,#33631,#33632,#33633,#33634,#33635,#33636,#33637,
#33638,#33639,#33640,#33641,#33642),.UNSPECIFIED.,.F.,.F.,(4,3,3,3,3,3,
3,3,3,3,3,3,3,3,4),(-22.9425468016483,-22.8279221510401,-22.3316629738436,
-21.8354037966471,-21.3391446194506,-20.842885442254,-20.3466262650575,
-19.850367087861,-19.3541079106645,-18.8578487334679,-18.3615895562714,
-17.8653303790749,-17.3690712018784,-16.8728120246818,-16.6593614944688),
 .UNSPECIFIED.);
#582=B_SPLINE_CURVE_WITH_KNOTS('',3,(#33643,#33644,#33645,#33646,#33647,
#33648,#33649,#33650,#33651,#33652,#33653,#33654,#33655,#33656,#33657,#33658,
#33659,#33660,#33661,#33662,#33663,#33664,#33665,#33666,#33667,#33668,#33669,
#33670,#33671,#33672,#33673,#33674,#33675,#33676,#33677,#33678,#33679,#33680,
#33681,#33682,#33683,#33684,#33685),.UNSPECIFIED.,.F.,.F.,(4,3,3,3,3,3,
3,3,3,3,3,3,3,3,4),(13.6924981796334,13.8952569615027,14.3915161386992,
14.8877753158957,15.3840344930922,15.8802936702888,16.3765528474853,16.8728120246818,
17.3690712018783,17.8653303790749,18.3615895562714,18.8578487334679,19.3541079106644,
19.850367087861,19.9756834868129),.UNSPECIFIED.);
#583=B_SPLINE_CURVE_WITH_KNOTS('',3,(#33690,#33691,#33692,#33693,#33694,
#33695,#33696,#33697,#33698,#33699,#33700,#33701,#33702,#33703,#33704,#33705,
#33706,#33707,#33708,#33709,#33710,#33711,#33712,#33713,#33714,#33715,#33716,
#33717,#33718,#33719,#33720,#33721,#33722,#33723,#33724,#33725,#33726,#33727,
#33728,#33729),.UNSPECIFIED.,.F.,.F.,(4,3,3,3,3,3,3,3,3,3,3,3,3,4),(-29.2257321088278,
-28.7830322773984,-28.2867731002019,-27.7905139230054,-27.2942547458088,
-26.7979955686123,-26.3017363914158,-25.8054772142193,-25.3092180370227,
-24.8129588598262,-24.3166996826297,-23.8204405054332,-23.3241813282366,
-22.9425468016483),.UNSPECIFIED.);
#584=B_SPLINE_CURVE_WITH_KNOTS('',3,(#33730,#33731,#33732,#33733,#33734,
#33735,#33736,#33737,#33738,#33739,#33740,#33741,#33742,#33743,#33744,#33745,
#33746,#33747,#33748,#33749,#33750,#33751,#33752,#33753,#33754,#33755,#33756,
#33757,#33758,#33759,#33760,#33761,#33762,#33763,#33764,#33765,#33766,#33767,
#33768,#33769),.UNSPECIFIED.,.F.,.F.,(4,3,3,3,3,3,3,3,3,3,3,3,3,4),(19.9756834868129,
20.3466262650575,20.842885442254,21.3391446194505,21.8354037966471,22.3316629738436,
22.8279221510401,23.3241813282366,23.8204405054331,24.3166996826297,24.8129588598262,
25.3092180370227,25.8054772142192,26.2588687939926),.UNSPECIFIED.);
#585=B_SPLINE_CURVE_WITH_KNOTS('',3,(#33774,#33775,#33776,#33777,#33778,
#33779,#33780,#33781,#33782,#33783,#33784,#33785,#33786,#33787,#33788,#33789,
#33790,#33791,#33792,#33793,#33794,#33795,#33796,#33797,#33798,#33799,#33800,
#33801,#33802,#33803,#33804,#33805,#33806,#33807,#33808,#33809,#33810,#33811,
#33812,#33813,#33814,#33815,#33816),.UNSPECIFIED.,.F.,.F.,(4,3,3,3,3,3,
3,3,3,3,3,3,3,3,4),(-35.5089174160075,-35.2344015809532,-34.7381424037567,
-34.2418832265602,-33.7456240493637,-33.2493648721671,-32.7531056949706,
-32.2568465177741,-31.7605873405776,-31.264328163381,-30.7680689861845,
-30.271809808988,-29.7755506317915,-29.2792914545949,-29.2257321088278),
 .UNSPECIFIED.);
#586=B_SPLINE_CURVE_WITH_KNOTS('',3,(#33817,#33818,#33819,#33820,#33821,
#33822,#33823,#33824,#33825,#33826,#33827,#33828,#33829,#33830,#33831,#33832,
#33833,#33834,#33835,#33836,#33837,#33838,#33839,#33840,#33841,#33842,#33843,
#33844,#33845,#33846,#33847,#33848,#33849,#33850,#33851,#33852,#33853,#33854,
#33855,#33856,#33857,#33858,#33859),.UNSPECIFIED.,.F.,.F.,(4,3,3,3,3,3,
3,3,3,3,3,3,3,3,4),(26.2588687939926,26.3017363914158,26.7979955686123,
27.2942547458088,27.7905139230053,28.2867731002019,28.7830322773984,29.2792914545949,
29.7755506317914,30.271809808988,30.7680689861845,31.264328163381,31.7605873405775,
32.2568465177741,32.5420541011721),.UNSPECIFIED.);
#587=B_SPLINE_CURVE_WITH_KNOTS('',3,(#33864,#33865,#33866,#33867,#33868,
#33869,#33870,#33871,#33872,#33873,#33874,#33875,#33876,#33877,#33878,#33879,
#33880,#33881,#33882,#33883,#33884,#33885,#33886,#33887,#33888,#33889,#33890,
#33891,#33892,#33893,#33894,#33895,#33896,#33897,#33898,#33899,#33900,#33901,
#33902,#33903,#33904,#33905,#33906),.UNSPECIFIED.,.F.,.F.,(4,3,3,3,3,3,
3,3,3,3,3,3,3,3,4),(-41.792102723187,-41.685770884508,-41.1895117073115,
-40.693252530115,-40.1969933529185,-39.700734175722,-39.2044749985254,-38.7082158213289,
-38.2119566441324,-37.7156974669359,-37.2194382897393,-36.7231791125428,
-36.2269199353463,-35.7306607581498,-35.5089174160075),.UNSPECIFIED.);
#588=B_SPLINE_CURVE_WITH_KNOTS('',3,(#33907,#33908,#33909,#33910,#33911,
#33912,#33913,#33914,#33915,#33916,#33917,#33918,#33919,#33920,#33921,#33922,
#33923,#33924,#33925,#33926,#33927,#33928,#33929,#33930,#33931,#33932,#33933,
#33934,#33935,#33936,#33937,#33938,#33939,#33940,#33941,#33942,#33943,#33944,
#33945,#33946,#33947,#33948,#33949),.UNSPECIFIED.,.F.,.F.,(4,3,3,3,3,3,
3,3,3,3,3,3,3,3,4),(32.5420541011721,32.7531056949706,33.2493648721671,
33.7456240493636,34.2418832265602,34.7381424037567,35.2344015809532,35.7306607581497,
36.2269199353462,36.7231791125428,37.2194382897393,37.7156974669358,38.2119566441323,
38.7082158213289,38.8252394083516),.UNSPECIFIED.);
#589=B_SPLINE_CURVE_WITH_KNOTS('',3,(#33954,#33955,#33956,#33957,#33958,
#33959,#33960,#33961,#33962,#33963,#33964,#33965,#33966,#33967,#33968,#33969,
#33970,#33971,#33972,#33973,#33974,#33975,#33976,#33977,#33978,#33979,#33980,
#33981,#33982,#33983,#33984,#33985,#33986,#33987,#33988,#33989,#33990,#33991,
#33992,#33993),.UNSPECIFIED.,.F.,.F.,(4,3,3,3,3,3,3,3,3,3,3,3,3,4),(-48.0752880303667,
-47.6408810108663,-47.1446218336698,-46.6483626564733,-46.1521034792768,
-45.6558443020802,-45.1595851248837,-44.6633259476872,-44.1670667704907,
-43.6708075932941,-43.1745484160976,-42.6782892389011,-42.1820300617046,
-41.792102723187),.UNSPECIFIED.);
#590=B_SPLINE_CURVE_WITH_KNOTS('',3,(#33994,#33995,#33996,#33997,#33998,
#33999,#34000,#34001,#34002,#34003,#34004,#34005,#34006,#34007,#34008,#34009,
#34010,#34011,#34012,#34013,#34014,#34015,#34016,#34017,#34018,#34019,#34020,
#34021,#34022,#34023,#34024,#34025,#34026,#34027,#34028,#34029,#34030,#34031,
#34032,#34033),.UNSPECIFIED.,.F.,.F.,(4,3,3,3,3,3,3,3,3,3,3,3,3,4),(38.8252394083516,
39.2044749985254,39.7007341757219,40.1969933529184,40.693252530115,41.1895117073115,
41.685770884508,42.1820300617045,42.678289238901,43.1745484160976,43.6708075932941,
44.1670667704906,44.6633259476871,45.1084247155313),.UNSPECIFIED.);
#591=B_SPLINE_CURVE_WITH_KNOTS('',3,(#34038,#34039,#34040,#34041,#34042,
#34043,#34044,#34045,#34046,#34047,#34048,#34049,#34050,#34051,#34052,#34053,
#34054,#34055,#34056,#34057,#34058,#34059,#34060,#34061,#34062,#34063,#34064,
#34065,#34066,#34067,#34068,#34069,#34070,#34071,#34072,#34073,#34074,#34075,
#34076,#34077,#34078,#34079,#34080),.UNSPECIFIED.,.F.,.F.,(4,3,3,3,3,3,
3,3,3,3,3,3,3,3,4),(-54.3584733375463,-54.0922503144212,-53.5959911372246,
-53.0997319600281,-52.6034727828316,-52.1072136056351,-51.6109544284385,
-51.114695251242,-50.6184360740455,-50.122176896849,-49.6259177196524,-49.1296585424559,
-48.6333993652594,-48.1371401880629,-48.0752880303667),.UNSPECIFIED.);
#592=B_SPLINE_CURVE_WITH_KNOTS('',3,(#34081,#34082,#34083,#34084,#34085,
#34086,#34087,#34088,#34089,#34090,#34091,#34092,#34093,#34094,#34095,#34096,
#34097,#34098,#34099,#34100,#34101,#34102,#34103,#34104,#34105,#34106,#34107,
#34108,#34109,#34110,#34111,#34112,#34113,#34114,#34115,#34116,#34117,#34118,
#34119,#34120,#34121,#34122,#34123),.UNSPECIFIED.,.F.,.F.,(4,3,3,3,3,3,
3,3,3,3,3,3,3,3,4),(45.1084247155313,45.1595851248837,45.6558443020802,
46.1521034792767,46.6483626564732,47.1446218336698,47.6408810108663,48.1371401880628,
48.6333993652593,49.1296585424559,49.6259177196524,50.1221768968489,50.6184360740454,
51.114695251242,51.3916100227108),.UNSPECIFIED.);
#593=B_SPLINE_CURVE_WITH_KNOTS('',3,(#34128,#34129,#34130,#34131,#34132,
#34133,#34134,#34135,#34136,#34137,#34138,#34139,#34140,#34141,#34142,#34143,
#34144,#34145,#34146,#34147,#34148,#34149,#34150,#34151,#34152,#34153,#34154,
#34155,#34156,#34157,#34158,#34159,#34160,#34161,#34162,#34163,#34164,#34165,
#34166,#34167,#34168,#34169,#34170),.UNSPECIFIED.,.F.,.F.,(4,3,3,3,3,3,
3,3,3,3,3,3,3,3,4),(-60.6416586447259,-60.543619617976,-60.0473604407794,
-59.5511012635829,-59.0548420863864,-58.5585829091899,-58.0623237319934,
-57.5660645547968,-57.0698053776003,-56.5735462004038,-56.0772870232073,
-55.5810278460107,-55.0847686688142,-54.5885094916177,-54.3584733375463),
 .UNSPECIFIED.);
#594=B_SPLINE_CURVE_WITH_KNOTS('',3,(#34171,#34172,#34173,#34174,#34175,
#34176,#34177,#34178,#34179,#34180,#34181,#34182,#34183,#34184,#34185,#34186,
#34187,#34188,#34189,#34190,#34191,#34192,#34193,#34194,#34195,#34196,#34197,
#34198,#34199,#34200,#34201,#34202,#34203,#34204,#34205,#34206,#34207,#34208,
#34209,#34210,#34211,#34212,#34213),.UNSPECIFIED.,.F.,.F.,(4,3,3,3,3,3,
3,3,3,3,3,3,3,3,4),(51.3916100227108,51.6109544284385,52.107213605635,52.6034727828315,
53.0997319600281,53.5959911372246,54.0922503144211,54.5885094916176,55.0847686688141,
55.5810278460107,56.0772870232072,56.5735462004037,57.0698053776003,57.5660645547968,
57.6747953298905),.UNSPECIFIED.);
#595=B_SPLINE_CURVE_WITH_KNOTS('',3,(#34218,#34219,#34220,#34221,#34222,
#34223,#34224,#34225,#34226,#34227,#34228,#34229,#34230,#34231,#34232,#34233,
#34234,#34235,#34236,#34237,#34238,#34239,#34240,#34241,#34242,#34243,#34244,
#34245,#34246,#34247,#34248,#34249,#34250,#34251,#34252,#34253,#34254,#34255,
#34256,#34257),.UNSPECIFIED.,.F.,.F.,(4,3,3,3,3,3,3,3,3,3,3,3,3,4),(-66.9248439519054,
-66.4987297443343,-66.0024705671378,-65.5062113899412,-65.0099522127447,
-64.5136930355482,-64.0174338583517,-63.5211746811551,-63.0249155039586,
-62.5286563267621,-62.0323971495656,-61.536137972369,-61.0398787951725,
-60.6416586447259),.UNSPECIFIED.);
#596=B_SPLINE_CURVE_WITH_KNOTS('',3,(#34258,#34259,#34260,#34261,#34262,
#34263,#34264,#34265,#34266,#34267,#34268,#34269,#34270,#34271,#34272,#34273,
#34274,#34275,#34276,#34277,#34278,#34279,#34280,#34281,#34282,#34283,#34284,
#34285,#34286,#34287,#34288,#34289,#34290,#34291,#34292,#34293,#34294,#34295,
#34296,#34297),.UNSPECIFIED.,.F.,.F.,(4,3,3,3,3,3,3,3,3,3,3,3,3,4),(57.6747953298905,
58.0623237319933,58.5585829091898,59.0548420863863,59.5511012635829,60.0473604407794,
60.5436196179759,61.0398787951725,61.536137972369,62.0323971495655,62.528656326762,
63.0249155039585,63.5211746811551,63.95798063707),.UNSPECIFIED.);
#597=B_SPLINE_CURVE_WITH_KNOTS('',3,(#34302,#34303,#34304,#34305,#34306,
#34307,#34308,#34309,#34310,#34311,#34312,#34313,#34314,#34315,#34316,#34317,
#34318,#34319,#34320,#34321,#34322,#34323,#34324,#34325,#34326,#34327,#34328,
#34329,#34330,#34331,#34332,#34333,#34334,#34335,#34336,#34337,#34338,#34339,
#34340,#34341,#34342,#34343,#34344),.UNSPECIFIED.,.F.,.F.,(4,3,3,3,3,3,
3,3,3,3,3,3,3,3,4),(-73.2080292590851,-72.9500990478891,-72.4538398706926,
-71.957580693496,-71.4613215162995,-70.965062339103,-70.4688031619065,-69.97254398471,
-69.4762848075134,-68.9800256303169,-68.4837664531204,-67.9875072759238,
-67.4912480987273,-66.9949889215308,-66.9248439519054),.UNSPECIFIED.);
#598=B_SPLINE_CURVE_WITH_KNOTS('',3,(#34345,#34346,#34347,#34348,#34349,
#34350,#34351,#34352,#34353,#34354,#34355,#34356,#34357,#34358,#34359,#34360,
#34361,#34362,#34363,#34364,#34365,#34366,#34367,#34368,#34369,#34370,#34371,
#34372,#34373,#34374,#34375,#34376,#34377,#34378,#34379,#34380,#34381,#34382,
#34383,#34384,#34385,#34386,#34387),.UNSPECIFIED.,.F.,.F.,(4,3,3,3,3,3,
3,3,3,3,3,3,3,3,4),(63.95798063707,64.0174338583516,64.5136930355481,65.0099522127446,
65.5062113899412,66.0024705671377,66.4987297443342,66.9949889215307,67.4912480987273,
67.9875072759238,68.4837664531203,68.9800256303168,69.4762848075134,69.9725439847099,
70.2411659442497),.UNSPECIFIED.);
#599=B_SPLINE_CURVE_WITH_KNOTS('',3,(#34393,#34394,#34395,#34396,#34397,
#34398,#34399,#34400,#34401,#34402,#34403,#34404,#34405,#34406,#34407),
 .UNSPECIFIED.,.F.,.F.,(4,1,1,1,1,1,1,1,1,1,1,1,4),(78.5398163397448,78.6099613093701,
79.1062204865667,79.6024796637632,80.0987388409597,80.5949980181562,81.0912571953528,
81.5875163725493,82.0837755497458,82.5800347269423,83.0762939041389,83.5725530813354,
83.9763231755241),.UNSPECIFIED.);
#600=B_SPLINE_CURVE_WITH_KNOTS('',3,(#34410,#34411,#34412,#34413,#34414,
#34415,#34416,#34417,#34418,#34419,#34420,#34421),.UNSPECIFIED.,.F.,.F.,
(4,1,1,1,1,1,1,1,1,4),(78.5398163397448,78.7674535574015,79.263712734598,
79.7599719117945,80.2562310889911,80.7524902661876,81.2487494433841,81.7450086205806,
82.2412677977772,82.7375269749737),.UNSPECIFIED.);
#601=B_SPLINE_CURVE_WITH_KNOTS('',3,(#34426,#34427,#34428,#34429,#34430,
#34431,#34432,#34433,#34434,#34435,#34436,#34437,#34438,#34439,#34440,#34441),
 .UNSPECIFIED.,.F.,.F.,(4,1,1,1,1,1,1,1,1,1,1,1,1,4),(72.2566310325653,
72.6548511830118,73.1511103602084,73.6473695374049,74.1436287146014,74.6398878917979,
75.1361470689945,75.632406246191,76.1286654233875,76.624924600584,77.1211837777806,
77.6174429549771,78.1137021321736,78.5398163397448),.UNSPECIFIED.);
#602=B_SPLINE_CURVE_WITH_KNOTS('',3,(#34442,#34443,#34444,#34445,#34446,
#34447,#34448,#34449,#34450,#34451,#34452,#34453,#34454,#34455,#34456,#34457,
#34458),.UNSPECIFIED.,.F.,.F.,(4,1,1,1,1,1,1,1,1,1,1,1,1,1,4),(72.2566310325653,
72.3160842538467,72.8123434310432,73.3086026082397,73.8048617854362,74.3011209626328,
74.7973801398293,75.2936393170258,75.7898984942223,76.2861576714189,76.7824168486154,
77.2786760258119,77.7749352030084,78.271194380205,78.5398163397448),
 .UNSPECIFIED.);
#603=B_SPLINE_CURVE_WITH_KNOTS('',3,(#34463,#34464,#34465,#34466,#34467,
#34468,#34469,#34470,#34471,#34472,#34473,#34474,#34475,#34476,#34477,#34478,
#34479),.UNSPECIFIED.,.F.,.F.,(4,1,1,1,1,1,1,1,1,1,1,1,1,1,4),(65.9734457253856,
66.203481879457,66.6997410566536,67.1960002338501,67.6922594110466,68.1885185882431,
68.6847777654396,69.1810369426362,69.6772961198327,70.1735552970292,70.6698144742257,
71.1660736514223,71.6623328286188,72.1585920058153,72.2566310325653),
 .UNSPECIFIED.);
#604=B_SPLINE_CURVE_WITH_KNOTS('',3,(#34480,#34481,#34482,#34483,#34484,
#34485,#34486,#34487,#34488,#34489,#34490,#34491,#34492,#34493,#34494,#34495),
 .UNSPECIFIED.,.F.,.F.,(4,1,1,1,1,1,1,1,1,1,1,1,1,4),(65.9734457253856,
66.3609741274884,66.8572333046849,67.3534924818814,67.849751659078,68.3460108362745,
68.842270013471,69.3385291906675,69.8347883678641,70.3310475450606,70.8273067222571,
71.3235658994536,71.8198250766501,72.2566310325653),.UNSPECIFIED.);
#605=B_SPLINE_CURVE_WITH_KNOTS('',3,(#34500,#34501,#34502,#34503,#34504,
#34505,#34506,#34507,#34508,#34509,#34510,#34511,#34512,#34513,#34514,#34515,
#34516),.UNSPECIFIED.,.F.,.F.,(4,1,1,1,1,1,1,1,1,1,1,1,1,1,4),(59.6902604182061,
59.7521125759022,60.2483717530987,60.7446309302953,61.2408901074918,61.7371492846883,
62.2334084618848,62.7296676390814,63.2259268162779,63.7221859934744,64.2184451706709,
64.7147043478674,65.210963525064,65.7072227022605,65.9734457253856),
 .UNSPECIFIED.);
#606=B_SPLINE_CURVE_WITH_KNOTS('',3,(#34517,#34518,#34519,#34520,#34521,
#34522,#34523,#34524,#34525,#34526,#34527,#34528,#34529,#34530,#34531,#34532,
#34533),.UNSPECIFIED.,.F.,.F.,(4,1,1,1,1,1,1,1,1,1,1,1,1,1,4),(59.6902604182061,
59.9096048239336,60.4058640011301,60.9021231783266,61.3983823555232,61.8946415327197,
62.3909007099162,62.8871598871127,63.3834190643093,63.8796782415058,64.3759374187023,
64.8721965958988,65.3684557730953,65.8647149502919,65.9734457253856),
 .UNSPECIFIED.);
#607=B_SPLINE_CURVE_WITH_KNOTS('',3,(#34538,#34539,#34540,#34541,#34542,
#34543,#34544,#34545,#34546,#34547,#34548,#34549,#34550,#34551,#34552,#34553),
 .UNSPECIFIED.,.F.,.F.,(4,1,1,1,1,1,1,1,1,1,1,1,1,4),(53.4070751110264,
53.7970024495439,54.2932616267404,54.789520803937,55.2857799811335,55.78203915833,
56.2782983355265,56.7745575127231,57.2708166899196,57.7670758671161,58.2633350443126,
58.7595942215092,59.2558533987057,59.6902604182061),.UNSPECIFIED.);
#608=B_SPLINE_CURVE_WITH_KNOTS('',3,(#34554,#34555,#34556,#34557,#34558,
#34559,#34560,#34561,#34562,#34563,#34564,#34565,#34566,#34567,#34568,#34569,
#34570),.UNSPECIFIED.,.F.,.F.,(4,1,1,1,1,1,1,1,1,1,1,1,1,1,4),(53.4070751110264,
53.4582355203788,53.9544946975753,54.4507538747718,54.9470130519683,55.4432722291649,
55.9395314063614,56.4357905835579,56.9320497607544,57.428308937951,57.9245681151475,
58.420827292344,58.9170864695405,59.4133456467371,59.6902604182061),
 .UNSPECIFIED.);
#609=B_SPLINE_CURVE_WITH_KNOTS('',3,(#34575,#34576,#34577,#34578,#34579,
#34580,#34581,#34582,#34583,#34584,#34585,#34586,#34587,#34588,#34589,#34590,
#34591),.UNSPECIFIED.,.F.,.F.,(4,1,1,1,1,1,1,1,1,1,1,1,1,1,4),(47.1238898038469,
47.3456331459891,47.8418923231856,48.3381515003821,48.8344106775787,49.3306698547752,
49.8269290319717,50.3231882091682,50.8194473863648,51.3157065635613,51.8119657407578,
52.3082249179543,52.8044840951509,53.3007432723474,53.4070751110264),
 .UNSPECIFIED.);
#610=B_SPLINE_CURVE_WITH_KNOTS('',3,(#34592,#34593,#34594,#34595,#34596,
#34597,#34598,#34599,#34600,#34601,#34602,#34603,#34604,#34605,#34606,#34607),
 .UNSPECIFIED.,.F.,.F.,(4,1,1,1,1,1,1,1,1,1,1,1,1,4),(47.1238898038469,
47.5031253940205,47.999384571217,48.4956437484135,48.9919029256101,49.4881621028066,
49.9844212800031,50.4806804571996,50.9769396343962,51.4731988115927,51.9694579887892,
52.4657171659857,52.9619763431823,53.4070751110264),.UNSPECIFIED.);
#611=B_SPLINE_CURVE_WITH_KNOTS('',3,(#34612,#34613,#34614,#34615,#34616,
#34617,#34618,#34619,#34620,#34621,#34622,#34623,#34624,#34625,#34626,#34627,
#34628),.UNSPECIFIED.,.F.,.F.,(4,1,1,1,1,1,1,1,1,1,1,1,1,1,4),(40.8407044966672,
40.8942638424343,41.3905230196308,41.8867821968273,42.3830413740238,42.8793005512204,
43.3755597284169,43.8718189056134,44.36807808281,44.8643372600065,45.360596437203,
45.8568556143995,46.353114791596,46.8493739687926,47.1238898038469),
 .UNSPECIFIED.);
#612=B_SPLINE_CURVE_WITH_KNOTS('',3,(#34629,#34630,#34631,#34632,#34633,
#34634,#34635,#34636,#34637,#34638,#34639,#34640,#34641,#34642,#34643,#34644,
#34645),.UNSPECIFIED.,.F.,.F.,(4,1,1,1,1,1,1,1,1,1,1,1,1,1,4),(40.8407044966672,
41.0517560904657,41.5480152676622,42.0442744448587,42.5405336220552,43.0367927992518,
43.5330519764483,44.0293111536448,44.5255703308413,45.0218295080379,45.5180886852344,
46.0143478624309,46.5106070396274,47.006866216824,47.1238898038469),
 .UNSPECIFIED.);
#613=B_SPLINE_CURVE_WITH_KNOTS('',3,(#34650,#34651,#34652,#34653,#34654,
#34655,#34656,#34657,#34658,#34659,#34660,#34661,#34662,#34663,#34664,#34665),
 .UNSPECIFIED.,.F.,.F.,(4,1,1,1,1,1,1,1,1,1,1,1,1,4),(34.5575191894877,
34.939153716076,35.4354128932725,35.931672070469,36.4279312476656,36.9241904248621,
37.4204496020586,37.9167087792551,38.4129679564517,38.9092271336482,39.4054863108447,
39.9017454880412,40.3980046652377,40.8407044966672),.UNSPECIFIED.);
#614=B_SPLINE_CURVE_WITH_KNOTS('',3,(#34666,#34667,#34668,#34669,#34670,
#34671,#34672,#34673,#34674,#34675,#34676,#34677,#34678,#34679,#34680,#34681,
#34682),.UNSPECIFIED.,.F.,.F.,(4,1,1,1,1,1,1,1,1,1,1,1,1,1,4),(34.5575191894877,
34.6003867869109,35.0966459641074,35.5929051413039,36.0891643185004,36.585423495697,
37.0816826728935,37.57794185009,38.0742010272865,38.5704602044831,39.0667193816796,
39.5629785588761,40.0592377360726,40.5554969132692,40.8407044966672),
 .UNSPECIFIED.);
#615=B_SPLINE_CURVE_WITH_KNOTS('',3,(#34687,#34688,#34689,#34690,#34691,
#34692,#34693,#34694,#34695,#34696,#34697,#34698,#34699,#34700,#34701,#34702,
#34703),.UNSPECIFIED.,.F.,.F.,(4,1,1,1,1,1,1,1,1,1,1,1,1,1,4),(28.2743338823082,
28.4877844125212,28.9840435897177,29.4803027669142,29.9765619441107,30.4728211213073,
30.9690802985038,31.4653394757003,31.9615986528968,32.4578578300934,32.9541170072899,
33.4503761844864,33.9466353616829,34.4428945388795,34.5575191894877),
 .UNSPECIFIED.);
#616=B_SPLINE_CURVE_WITH_KNOTS('',3,(#34704,#34705,#34706,#34707,#34708,
#34709,#34710,#34711,#34712,#34713,#34714,#34715,#34716,#34717,#34718,#34719),
 .UNSPECIFIED.,.F.,.F.,(4,1,1,1,1,1,1,1,1,1,1,1,1,4),(28.2743338823082,
28.6452766605526,29.1415358377491,29.6377950149456,30.1340541921422,30.6303133693387,
31.1265725465352,31.6228317237317,32.1190909009282,32.6153500781248,33.1116092553213,
33.6078684325178,34.1041276097143,34.5575191894877),.UNSPECIFIED.);
#617=B_SPLINE_CURVE_WITH_KNOTS('',3,(#34724,#34725,#34726,#34727,#34728,
#34729,#34730,#34731,#34732,#34733,#34734,#34735,#34736,#34737,#34738,#34739,
#34740),.UNSPECIFIED.,.F.,.F.,(4,1,1,1,1,1,1,1,1,1,1,1,1,1,4),(21.9911485751285,
22.0364151089663,22.5326742861629,23.0289334633594,23.5251926405559,24.0214518177524,
24.517710994949,25.0139701721455,25.510229349342,26.0064885265385,26.5027477037351,
26.9990068809316,27.4952660581281,27.9915252353246,28.2743338823082),
 .UNSPECIFIED.);
#618=B_SPLINE_CURVE_WITH_KNOTS('',3,(#34741,#34742,#34743,#34744,#34745,
#34746,#34747,#34748,#34749,#34750,#34751,#34752,#34753,#34754,#34755,#34756,
#34757),.UNSPECIFIED.,.F.,.F.,(4,1,1,1,1,1,1,1,1,1,1,1,1,1,4),(21.9911485751285,
22.1939073569978,22.6901665341943,23.1864257113908,23.6826848885873,24.1789440657839,
24.6752032429804,25.1714624201769,25.6677215973734,26.16398077457,26.6602399517665,
27.156499128963,27.6527583061595,28.1490174833561,28.2743338823082),
 .UNSPECIFIED.);
#619=B_SPLINE_CURVE_WITH_KNOTS('',3,(#34762,#34763,#34764,#34765,#34766,
#34767,#34768,#34769,#34770,#34771,#34772,#34773,#34774,#34775,#34776,#34777),
 .UNSPECIFIED.,.F.,.F.,(4,1,1,1,1,1,1,1,1,1,1,1,1,4),(15.707963267949,16.0813049826081,
16.5775641598046,17.0738233370011,17.5700825141976,18.0663416913942,18.5626008685907,
19.0588600457872,19.5551192229837,20.0513784001803,20.5476375773768,21.0438967545733,
21.5401559317698,21.9911485751285),.UNSPECIFIED.);
#620=B_SPLINE_CURVE_WITH_KNOTS('',3,(#34778,#34779,#34780,#34781,#34782,
#34783,#34784,#34785,#34786,#34787,#34788,#34789,#34790,#34791,#34792,#34793,
#34794),.UNSPECIFIED.,.F.,.F.,(4,1,1,1,1,1,1,1,1,1,1,1,1,1,4),(15.707963267949,
15.742538053443,16.2387972306395,16.735056407836,17.2313155850325,17.7275747622291,
18.2238339394256,18.7200931166221,19.2163522938186,19.7126114710152,20.2088706482117,
20.7051298254082,21.2013890026047,21.6976481798012,21.9911485751285),
 .UNSPECIFIED.);
#621=B_SPLINE_CURVE_WITH_KNOTS('',3,(#34811,#34812,#34813,#34814,#34815,
#34816,#34817,#34818,#34819,#34820,#34821,#34822,#34823,#34824,#34825,#34826,
#34827,#34828,#34829,#34830,#34831,#34832,#34833,#34834,#34835,#34836,#34837,
#34838,#34839,#34840,#34841,#34842,#34843,#34844,#34845,#34846,#34847,#34848,
#34849,#34850,#34851,#34852,#34853,#34854,#34855,#34856,#34857,#34858,#34859,
#34860,#34861,#34862,#34863,#34864,#34865,#34866,#34867,#34868,#34869,#34870,
#34871,#34872,#34873,#34874,#34875,#34876,#34877,#34878,#34879,#34880,#34881,
#34882,#34883,#34884,#34885,#34886,#34887,#34888,#34889,#34890,#34891,#34892,
#34893,#34894,#34895,#34896,#34897,#34898,#34899,#34900,#34901,#34902,#34903,
#34904,#34905,#34906,#34907,#34908,#34909,#34910,#34911,#34912,#34913,#34914,
#34915,#34916,#34917,#34918,#34919,#34920,#34921,#34922,#34923,#34924,#34925,
#34926,#34927,#34928,#34929,#34930,#34931,#34932,#34933,#34934,#34935,#34936,
#34937,#34938,#34939,#34940),.UNSPECIFIED.,.F.,.F.,(4,3,3,3,3,3,3,3,3,3,
3,3,3,3,3,3,3,3,3,3,3,3,3,3,3,3,3,3,3,3,3,3,3,3,3,3,3,3,3,3,3,3,3,4),(-2.39439908413783,
-2.30957055714608,-2.28423857194394,-2.1992123713416,-2.13667984916741,
-2.10464861416482,-2.08645022218986,-2.07576631254953,-1.99136800162839,
-1.90707270778559,-1.82339088190019,-1.79228120991215,-1.77736472887211,
-1.7676964721655,-1.69895219394804,-1.61556580382843,-1.5316846344345,-1.44789196762844,
-1.36656757104543,-1.33607092232681,-1.32613672030475,-1.31756701322122,
-1.23465419226132,-1.15190857282007,-1.12259438129642,-1.03956979703191,
-0.956697216050081,-0.906629990836835,-0.883172486284775,-0.870094147064423,
-0.788031684106132,-0.705898296538195,-0.624514288049676,-0.556159414344109,
-0.486639487551095,-0.456224519579152,-0.437728905707078,-0.429197413628179,
-0.348523537028714,-0.267263381794694,-0.186163914396806,-0.105687092063476,
-0.0266190971408737,0.),.UNSPECIFIED.);
#622=B_SPLINE_CURVE_WITH_KNOTS('',3,(#34943,#34944,#34945,#34946,#34947,
#34948,#34949,#34950,#34951,#34952,#34953,#34954,#34955,#34956,#34957,#34958,
#34959,#34960,#34961,#34962,#34963,#34964,#34965,#34966,#34967,#34968,#34969,
#34970,#34971,#34972,#34973,#34974,#34975,#34976,#34977,#34978,#34979,#34980,
#34981,#34982,#34983,#34984,#34985,#34986,#34987,#34988,#34989,#34990,#34991,
#34992,#34993,#34994,#34995,#34996,#34997,#34998,#34999,#35000,#35001,#35002,
#35003,#35004,#35005,#35006,#35007,#35008,#35009,#35010,#35011,#35012,#35013,
#35014,#35015,#35016,#35017,#35018,#35019,#35020,#35021,#35022,#35023,#35024,
#35025,#35026,#35027,#35028,#35029,#35030,#35031,#35032,#35033,#35034,#35035,
#35036,#35037,#35038,#35039,#35040,#35041,#35042,#35043,#35044,#35045,#35046,
#35047,#35048,#35049,#35050,#35051,#35052,#35053,#35054,#35055,#35056,#35057,
#35058,#35059,#35060,#35061,#35062,#35063,#35064,#35065,#35066,#35067,#35068,
#35069,#35070,#35071,#35072),.UNSPECIFIED.,.F.,.F.,(4,3,3,3,3,3,3,3,3,3,
3,3,3,3,3,3,3,3,3,3,3,3,3,3,3,3,3,3,3,3,3,3,3,3,3,3,3,3,3,3,3,3,3,4),(-2.39814946016208,
-2.31696204037272,-2.29529569174575,-2.21456972428986,-2.15490479428083,
-2.12648768752725,-2.10829922528945,-2.09678298213356,-2.01553459190536,
-1.93371848537121,-1.85215105787095,-1.82342586445762,-1.81332878484419,
-1.80373550389277,-1.73725028421764,-1.65586989418317,-1.57363756065892,
-1.49104149188928,-1.41031007232168,-1.38003578998382,-1.37054045619564,
-1.36256005099984,-1.27951391668103,-1.19605898221033,-1.16811581361885,
-1.08502370473436,-1.00162059695019,-0.950031361007238,-0.926067853715056,
-0.912515238783363,-0.828732204328819,-0.744476329949599,-0.660367719531965,
-0.588906709406546,-0.515293370730728,-0.483087535060058,-0.463174686736147,
-0.454053033267499,-0.370331877320448,-0.285650817662844,-0.200462204104426,
-0.115556056832656,-0.0317686426882691,0.),.UNSPECIFIED.);
#623=B_SPLINE_CURVE_WITH_KNOTS('',3,(#35085,#35086,#35087,#35088,#35089,
#35090,#35091,#35092,#35093,#35094,#35095,#35096,#35097,#35098,#35099,#35100,
#35101,#35102,#35103,#35104,#35105,#35106,#35107,#35108,#35109,#35110,#35111,
#35112,#35113,#35114,#35115,#35116,#35117,#35118,#35119,#35120,#35121,#35122,
#35123,#35124,#35125,#35126,#35127,#35128,#35129,#35130,#35131,#35132,#35133,
#35134,#35135,#35136,#35137,#35138,#35139,#35140,#35141,#35142,#35143,#35144,
#35145,#35146,#35147,#35148,#35149,#35150,#35151,#35152,#35153,#35154,#35155,
#35156,#35157,#35158,#35159,#35160,#35161,#35162,#35163,#35164,#35165,#35166,
#35167,#35168,#35169,#35170,#35171,#35172,#35173,#35174,#35175,#35176,#35177,
#35178,#35179,#35180,#35181,#35182,#35183,#35184,#35185,#35186,#35187,#35188,
#35189,#35190,#35191,#35192,#35193,#35194,#35195,#35196,#35197,#35198,#35199,
#35200,#35201,#35202,#35203,#35204,#35205,#35206,#35207,#35208,#35209,#35210,
#35211,#35212,#35213,#35214),.UNSPECIFIED.,.F.,.F.,(4,3,3,3,3,3,3,3,3,3,
3,3,3,3,3,3,3,3,3,3,3,3,3,3,3,3,3,3,3,3,3,3,3,3,3,3,3,3,3,3,3,3,3,4),(-2.39814946016205,
-2.31696204062401,-2.29529569174573,-2.2145697251006,-2.15490479499024,
-2.12648768749454,-2.10829922547412,-2.0967829822177,-2.01553459282142,
-1.93371848603571,-1.85215105805855,-1.82342586459833,-1.81332878335441,
-1.80373550349862,-1.73725028421766,-1.65586989316896,-1.5736375593772,
-1.4910414902031,-1.41031007105705,-1.38003578887728,-1.37054045289983,
-1.36256004385421,-1.27951390929298,-1.19605897401236,-1.16811581361891,
-1.08502370215676,-1.00162059508676,-0.950031359376745,-0.926067851441389,
-0.912515239871559,-0.828732202575563,-0.744476327910997,-0.660367724053132,
-0.588906709406608,-0.515293370730782,-0.483087535060108,-0.463174686568405,
-0.454053033116952,-0.370331890792948,-0.285650840288278,-0.200462224975479,
-0.115556068532172,-0.0317686353808436,0.),.UNSPECIFIED.);
#624=B_SPLINE_CURVE_WITH_KNOTS('',3,(#35219,#35220,#35221,#35222,#35223,
#35224,#35225,#35226,#35227,#35228,#35229,#35230,#35231,#35232,#35233,#35234,
#35235,#35236,#35237,#35238,#35239,#35240,#35241,#35242,#35243,#35244,#35245,
#35246,#35247,#35248,#35249,#35250,#35251,#35252,#35253,#35254,#35255,#35256,
#35257,#35258,#35259,#35260,#35261,#35262,#35263,#35264,#35265,#35266,#35267,
#35268,#35269,#35270,#35271,#35272,#35273,#35274,#35275,#35276,#35277,#35278,
#35279,#35280,#35281,#35282,#35283,#35284,#35285,#35286,#35287,#35288,#35289,
#35290,#35291,#35292,#35293,#35294,#35295,#35296,#35297,#35298,#35299,#35300,
#35301,#35302,#35303,#35304,#35305,#35306,#35307,#35308,#35309,#35310,#35311,
#35312,#35313,#35314,#35315,#35316,#35317,#35318,#35319,#35320,#35321,#35322,
#35323,#35324,#35325,#35326,#35327,#35328,#35329,#35330,#35331,#35332,#35333,
#35334,#35335,#35336,#35337,#35338,#35339,#35340,#35341,#35342,#35343,#35344,
#35345,#35346,#35347,#35348),.UNSPECIFIED.,.F.,.F.,(4,3,3,3,3,3,3,3,3,3,
3,3,3,3,3,3,3,3,3,3,3,3,3,3,3,3,3,3,3,3,3,3,3,3,3,3,3,3,3,3,3,3,3,4),(-2.3943990841377,
-2.30957055649357,-2.28423857194396,-2.19921237127506,-2.13667984910918,
-2.1046486142086,-2.08645022202531,-2.07576631330251,-1.99136800229055,
-1.90707270864944,-1.82339088267649,-1.79228121049439,-1.77736473146188,
-1.76769647286273,-1.69895219394807,-1.61556580382811,-1.53168463492449,
-1.44789197014347,-1.36656757293171,-1.3360709239773,-1.3261367157783,-1.31756701043144,
-1.23465419018272,-1.15190857364025,-1.12259438129642,-1.03956979670933,
-0.956697210017908,-0.906629985558681,-0.883172477530608,-0.87009415021638,
-0.788031687387272,-0.705898295573491,-0.624514274873492,-0.556159414344086,
-0.486639487551075,-0.456224519579133,-0.437728905932789,-0.429197413839012,
-0.348523527132435,-0.267263368798083,-0.186163910537152,-0.105687103755617,
-0.0266191312671287,0.),.UNSPECIFIED.);
#625=B_SPLINE_CURVE_WITH_KNOTS('',3,(#35961,#35962,#35963,#35964,#35965,
#35966,#35967,#35968,#35969,#35970,#35971,#35972,#35973,#35974,#35975,#35976),
 .UNSPECIFIED.,.F.,.F.,(4,3,3,3,3,4),(70.2411659442497,70.4688031619064,
70.9650623391029,71.4613215162994,71.9575806934959,72.3613507876847),
 .UNSPECIFIED.);
#626=B_SPLINE_CURVE_WITH_KNOTS('',3,(#35977,#35978,#35979,#35980,#35981,
#35982,#35983,#35984,#35985,#35986,#35987,#35988,#35989,#35990),
 .UNSPECIFIED.,.F.,.F.,(4,1,1,1,1,1,1,1,1,1,1,4),(10.376176187289,10.7799462814777,
11.2762054586742,11.7724646358708,12.2687238130673,12.7649829902638,13.2612421674603,
13.7575013446569,14.2537605218534,14.7500196990499,15.2462788762464,15.707963267949),
 .UNSPECIFIED.);
#627=B_SPLINE_CURVE_WITH_KNOTS('',3,(#35992,#35993,#35994,#35995,#35996,
#35997,#35998,#35999,#36000,#36001,#36002,#36003),.UNSPECIFIED.,.F.,.F.,
(4,1,1,1,1,1,1,1,1,4),(11.6149723878393,12.1112315650359,12.6074907422324,
13.1037499194289,13.6000090966254,14.096268273822,14.5925274510185,15.088786628215,
15.5850458054115,15.707963267949),.UNSPECIFIED.);
#628=B_SPLINE_CURVE_WITH_KNOTS('',3,(#36616,#36617,#36618,#36619,#36620,
#36621,#36622,#36623,#36624,#36625),.UNSPECIFIED.,.F.,.F.,(4,3,3,4),(-74.4388765794786,
-73.9426174022821,-73.4463582250856,-73.2080292590851),.UNSPECIFIED.);
#629=B_SPLINE_CURVE_WITH_KNOTS('',3,(#36664,#36665,#36666,#36667,#36668,
#36669,#36670,#36671,#36672,#36673,#36674,#36675,#36676,#36677,#36678,#36679),
 .UNSPECIFIED.,.F.,.F.,(4,3,3,3,3,4),(-4.09293042013086,-3.98050199480518,
-3.48293924545453,-2.98537649610388,-2.48781374675323,-2.06773127522693),
 .UNSPECIFIED.);
#630=B_SPLINE_CURVE_WITH_KNOTS('',3,(#36682,#36683,#36684,#36685,#36686,
#36687,#36688,#36689,#36690,#36691),.UNSPECIFIED.,.F.,.F.,(4,3,3,4),(0.,
0.497562749350642,0.995125498701295,1.11639350868636),.UNSPECIFIED.);
#631=B_SPLINE_CURVE_WITH_KNOTS('',3,(#36696,#36697,#36698,#36699,#36700,
#36701,#36702,#36703,#36704,#36705,#36706,#36707,#36708,#36709,#36710,#36711,
#36712,#36713,#36714,#36715,#36716,#36717,#36718,#36719,#36720,#36721,#36722,
#36723,#36724,#36725,#36726,#36727,#36728,#36729,#36730,#36731,#36732,#36733,
#36734,#36735),.UNSPECIFIED.,.F.,.F.,(4,3,3,3,3,3,3,3,3,3,3,3,3,4),(-10.3761157273103,
-9.95125498701294,-9.45369223766229,-8.95612948831165,-8.458566738961,-7.96100398961035,
-7.46344124025971,-6.96587849090906,-6.46831574155841,-5.97075299220777,
-5.47319024285712,-4.97562749350647,-4.47806474415583,-4.09293042013086),
 .UNSPECIFIED.);
#632=B_SPLINE_CURVE_WITH_KNOTS('',3,(#36736,#36737,#36738,#36739,#36740,
#36741,#36742,#36743,#36744,#36745,#36746,#36747,#36748,#36749,#36750,#36751,
#36752,#36753,#36754,#36755,#36756,#36757,#36758,#36759,#36760,#36761,#36762,
#36763,#36764,#36765,#36766,#36767,#36768,#36769,#36770,#36771,#36772,#36773,
#36774,#36775),.UNSPECIFIED.,.F.,.F.,(4,3,3,3,3,3,3,3,3,3,3,3,3,4),(1.11639350868636,
1.49268824805194,1.99025099740259,2.48781374675324,2.98537649610388,3.48293924545453,
3.98050199480518,4.47806474415582,4.97562749350647,5.47319024285711,5.97075299220776,
6.46831574155841,6.96587849090906,7.39957881586581),.UNSPECIFIED.);
#633=B_SPLINE_CURVE_WITH_KNOTS('',3,(#36780,#36781,#36782,#36783,#36784,
#36785,#36786,#36787,#36788,#36789,#36790,#36791,#36792,#36793,#36794,#36795,
#36796,#36797,#36798,#36799,#36800,#36801,#36802,#36803,#36804,#36805,#36806,
#36807,#36808,#36809,#36810,#36811,#36812,#36813,#36814,#36815,#36816,#36817,
#36818,#36819,#36820,#36821,#36822),.UNSPECIFIED.,.F.,.F.,(4,3,3,3,3,3,
3,3,3,3,3,3,3,3,4),(-16.65930103449,-16.4195707285714,-15.9220079792207,
-15.4244452298701,-14.9268824805194,-14.4293197311688,-13.9317569818181,
-13.4341942324675,-12.9366314831168,-12.4390687337662,-11.9415059844155,
-11.4439432350649,-10.9463804857142,-10.4488177363636,-10.3761157273103),
 .UNSPECIFIED.);
#634=B_SPLINE_CURVE_WITH_KNOTS('',3,(#36823,#36824,#36825,#36826,#36827,
#36828,#36829,#36830,#36831,#36832,#36833,#36834,#36835,#36836,#36837,#36838,
#36839,#36840,#36841,#36842,#36843,#36844,#36845,#36846,#36847,#36848,#36849,
#36850,#36851,#36852,#36853,#36854,#36855,#36856,#36857,#36858,#36859,#36860,
#36861,#36862,#36863,#36864,#36865),.UNSPECIFIED.,.F.,.F.,(4,3,3,3,3,3,
3,3,3,3,3,3,3,3,4),(7.39957881586581,7.4634412402597,7.96100398961035,8.45856673896099,
8.95612948831164,9.45369223766228,9.95125498701293,10.4488177363636,10.9463804857142,
11.4439432350649,11.9415059844155,12.4390687337662,12.9366314831168,13.4341942324675,
13.6827641230455),.UNSPECIFIED.);
#635=B_SPLINE_CURVE_WITH_KNOTS('',3,(#36870,#36871,#36872,#36873,#36874,
#36875,#36876,#36877,#36878,#36879,#36880,#36881,#36882,#36883,#36884,#36885,
#36886,#36887,#36888,#36889,#36890,#36891,#36892,#36893,#36894,#36895,#36896,
#36897,#36898,#36899,#36900,#36901,#36902,#36903,#36904,#36905,#36906,#36907,
#36908,#36909,#36910,#36911,#36912),.UNSPECIFIED.,.F.,.F.,(4,3,3,3,3,3,
3,3,3,3,3,3,3,3,4),(-22.9424863416697,-22.8878864701298,-22.3903237207791,
-21.8927609714285,-21.3951982220778,-20.8976354727272,-20.4000727233765,
-19.9025099740259,-19.4049472246752,-18.9073844753246,-18.4098217259739,
-17.9122589766233,-17.4146962272727,-16.917133477922,-16.65930103449),
 .UNSPECIFIED.);
#636=B_SPLINE_CURVE_WITH_KNOTS('',3,(#36913,#36914,#36915,#36916,#36917,
#36918,#36919,#36920,#36921,#36922,#36923,#36924,#36925,#36926,#36927,#36928,
#36929,#36930,#36931,#36932,#36933,#36934,#36935,#36936,#36937,#36938,#36939,
#36940,#36941,#36942,#36943,#36944,#36945,#36946,#36947,#36948,#36949,#36950,
#36951,#36952,#36953,#36954,#36955),.UNSPECIFIED.,.F.,.F.,(4,3,3,3,3,3,
3,3,3,3,3,3,3,3,4),(13.6827641230455,13.9317569818181,14.4293197311687,
14.9268824805194,15.42444522987,15.9220079792207,16.4195707285713,16.917133477922,
17.4146962272726,17.9122589766233,18.4098217259739,18.9073844753246,19.4049472246752,
19.9025099740259,19.9659494302252),.UNSPECIFIED.);
#637=B_SPLINE_CURVE_WITH_KNOTS('',3,(#36960,#36961,#36962,#36963,#36964,
#36965,#36966,#36967,#36968,#36969,#36970,#36971,#36972,#36973,#36974,#36975,
#36976,#36977,#36978,#36979,#36980,#36981,#36982,#36983,#36984,#36985,#36986,
#36987,#36988,#36989,#36990,#36991,#36992,#36993,#36994,#36995,#36996,#36997,
#36998,#36999),.UNSPECIFIED.,.F.,.F.,(4,3,3,3,3,3,3,3,3,3,3,3,3,4),(-29.2256716488491,
-28.8586394623375,-28.3610767129869,-27.8635139636362,-27.3659512142856,
-26.8683884649349,-26.3708257155843,-25.8732629662337,-25.375700216883,
-24.8781374675324,-24.3805747181817,-23.8830119688311,-23.3854492194804,
-22.9424863416697),.UNSPECIFIED.);
#638=B_SPLINE_CURVE_WITH_KNOTS('',3,(#37000,#37001,#37002,#37003,#37004,
#37005,#37006,#37007,#37008,#37009,#37010,#37011,#37012,#37013,#37014,#37015,
#37016,#37017,#37018,#37019,#37020,#37021,#37022,#37023,#37024,#37025,#37026,
#37027,#37028,#37029,#37030,#37031,#37032,#37033,#37034,#37035,#37036,#37037,
#37038,#37039),.UNSPECIFIED.,.F.,.F.,(4,3,3,3,3,3,3,3,3,3,3,3,3,4),(19.9659494302252,
20.4000727233765,20.8976354727272,21.3951982220778,21.8927609714285,22.3903237207791,
22.8878864701297,23.3854492194804,23.883011968831,24.3805747181817,24.8781374675323,
25.375700216883,25.8732629662336,26.2491347374046),.UNSPECIFIED.);
#639=B_SPLINE_CURVE_WITH_KNOTS('',3,(#37044,#37045,#37046,#37047,#37048,
#37049,#37050,#37051,#37052,#37053,#37054,#37055,#37056,#37057,#37058,#37059,
#37060,#37061,#37062,#37063,#37064,#37065,#37066,#37067,#37068,#37069,#37070,
#37071,#37072,#37073,#37074,#37075,#37076,#37077,#37078,#37079,#37080,#37081,
#37082,#37083,#37084,#37085,#37086),.UNSPECIFIED.,.F.,.F.,(4,3,3,3,3,3,
3,3,3,3,3,3,3,3,4),(-35.5088569560288,-35.3269552038959,-34.8293924545453,
-34.3318297051947,-33.834266955844,-33.3367042064934,-32.8391414571427,
-32.3415787077921,-31.8440159584414,-31.3464532090908,-30.8488904597401,
-30.3513277103895,-29.8537649610388,-29.3562022116882,-29.2256716488491),
 .UNSPECIFIED.);
#640=B_SPLINE_CURVE_WITH_KNOTS('',3,(#37087,#37088,#37089,#37090,#37091,
#37092,#37093,#37094,#37095,#37096,#37097,#37098,#37099,#37100,#37101,#37102,
#37103,#37104,#37105,#37106,#37107,#37108,#37109,#37110,#37111,#37112,#37113,
#37114,#37115,#37116,#37117,#37118,#37119,#37120,#37121,#37122,#37123,#37124,
#37125,#37126,#37127,#37128,#37129),.UNSPECIFIED.,.F.,.F.,(4,3,3,3,3,3,
3,3,3,3,3,3,3,3,4),(26.2491347374046,26.3708257155843,26.8683884649349,
27.3659512142856,27.8635139636362,28.3610767129869,28.8586394623375,29.3562022116881,
29.8537649610388,30.3513277103894,30.8488904597401,31.3464532090907,31.8440159584414,
32.341578707792,32.5323200445843),.UNSPECIFIED.);
#641=B_SPLINE_CURVE_WITH_KNOTS('',3,(#37134,#37135,#37136,#37137,#37138,
#37139,#37140,#37141,#37142,#37143,#37144,#37145,#37146,#37147,#37148,#37149,
#37150,#37151,#37152,#37153,#37154,#37155,#37156,#37157,#37158,#37159,#37160,
#37161,#37162,#37163,#37164,#37165,#37166,#37167,#37168,#37169,#37170,#37171,
#37172,#37173),.UNSPECIFIED.,.F.,.F.,(4,3,3,3,3,3,3,3,3,3,3,3,3,4),(-41.7920422632082,
-41.2977081961037,-40.8001454467531,-40.3025826974024,-39.8050199480518,
-39.3074571987011,-38.8098944493505,-38.3123316999998,-37.8147689506492,
-37.3172062012985,-36.8196434519479,-36.3220807025972,-35.8245179532466,
-35.5088569560288),.UNSPECIFIED.);
#642=B_SPLINE_CURVE_WITH_KNOTS('',3,(#37174,#37175,#37176,#37177,#37178,
#37179,#37180,#37181,#37182,#37183,#37184,#37185,#37186,#37187,#37188,#37189,
#37190,#37191,#37192,#37193,#37194,#37195,#37196,#37197,#37198,#37199,#37200,
#37201,#37202,#37203,#37204,#37205,#37206,#37207,#37208,#37209,#37210,#37211,
#37212,#37213,#37214,#37215,#37216),.UNSPECIFIED.,.F.,.F.,(4,3,3,3,3,3,
3,3,3,3,3,3,3,3,4),(32.5323200445843,32.8391414571427,33.3367042064933,
33.834266955844,34.3318297051946,34.8293924545453,35.3269552038959,35.8245179532466,
36.3220807025972,36.8196434519478,37.3172062012985,37.8147689506491,38.3123316999998,
38.8098944493504,38.815505351764),.UNSPECIFIED.);
#643=B_SPLINE_CURVE_WITH_KNOTS('',3,(#37221,#37222,#37223,#37224,#37225,
#37226,#37227,#37228,#37229,#37230,#37231,#37232,#37233,#37234,#37235,#37236,
#37237,#37238,#37239,#37240,#37241,#37242,#37243,#37244,#37245,#37246,#37247,
#37248,#37249,#37250,#37251,#37252,#37253,#37254,#37255,#37256,#37257,#37258,
#37259,#37260,#37261,#37262,#37263),.UNSPECIFIED.,.F.,.F.,(4,3,3,3,3,3,
3,3,3,3,3,3,3,3,4),(-48.0752275703879,-47.7660239376621,-47.2684611883115,
-46.7708984389608,-46.2733356896102,-45.7757729402595,-45.2782101909089,
-44.7806474415582,-44.2830846922076,-43.7855219428569,-43.2879591935063,
-42.7903964441556,-42.292833694805,-41.7952709454544,-41.7920422632082),
 .UNSPECIFIED.);
#644=B_SPLINE_CURVE_WITH_KNOTS('',3,(#37264,#37265,#37266,#37267,#37268,
#37269,#37270,#37271,#37272,#37273,#37274,#37275,#37276,#37277,#37278,#37279,
#37280,#37281,#37282,#37283,#37284,#37285,#37286,#37287,#37288,#37289,#37290,
#37291,#37292,#37293,#37294,#37295,#37296,#37297,#37298,#37299,#37300,#37301,
#37302,#37303),.UNSPECIFIED.,.F.,.F.,(4,3,3,3,3,3,3,3,3,3,3,3,3,4),(38.815505351764,
39.3074571987011,39.8050199480517,40.3025826974024,40.800145446753,41.2977081961037,
41.7952709454543,42.292833694805,42.7903964441556,43.2879591935063,43.7855219428569,
44.2830846922076,44.7806474415582,45.0986906589434),.UNSPECIFIED.);
#645=B_SPLINE_CURVE_WITH_KNOTS('',3,(#37308,#37309,#37310,#37311,#37312,
#37313,#37314,#37315,#37316,#37317,#37318,#37319,#37320,#37321,#37322,#37323,
#37324,#37325,#37326,#37327,#37328,#37329,#37330,#37331,#37332,#37333,#37334,
#37335,#37336,#37337,#37338,#37339,#37340,#37341,#37342,#37343,#37344,#37345,
#37346,#37347,#37348,#37349,#37350),.UNSPECIFIED.,.F.,.F.,(4,3,3,3,3,3,
3,3,3,3,3,3,3,3,4),(-54.3584128775676,-54.2343396792205,-53.7367769298699,
-53.2392141805192,-52.7416514311686,-52.2440886818179,-51.7465259324673,
-51.2489631831167,-50.751400433766,-50.2538376844154,-49.7562749350647,
-49.2587121857141,-48.7611494363634,-48.2635866870128,-48.0752275703879),
 .UNSPECIFIED.);
#646=B_SPLINE_CURVE_WITH_KNOTS('',3,(#37351,#37352,#37353,#37354,#37355,
#37356,#37357,#37358,#37359,#37360,#37361,#37362,#37363,#37364,#37365,#37366,
#37367,#37368,#37369,#37370,#37371,#37372,#37373,#37374,#37375,#37376,#37377,
#37378,#37379,#37380,#37381,#37382,#37383,#37384,#37385,#37386,#37387,#37388,
#37389,#37390,#37391,#37392,#37393),.UNSPECIFIED.,.F.,.F.,(4,3,3,3,3,3,
3,3,3,3,3,3,3,3,4),(45.0986906589434,45.2782101909088,45.7757729402595,
46.2733356896101,46.7708984389608,47.2684611883114,47.7660239376621,48.2635866870127,
48.7611494363634,49.258712185714,49.7562749350647,50.2538376844153,50.751400433766,
51.2489631831166,51.3818759661231),.UNSPECIFIED.);
#647=B_SPLINE_CURVE_WITH_KNOTS('',3,(#37398,#37399,#37400,#37401,#37402,
#37403,#37404,#37405,#37406,#37407,#37408,#37409,#37410,#37411,#37412,#37413,
#37414,#37415,#37416,#37417,#37418,#37419,#37420,#37421,#37422,#37423,#37424,
#37425,#37426,#37427,#37428,#37429,#37430,#37431,#37432,#37433,#37434,#37435,
#37436,#37437),.UNSPECIFIED.,.F.,.F.,(4,3,3,3,3,3,3,3,3,3,3,3,3,4),(-60.641598184747,
-60.2050926714283,-59.7075299220777,-59.209967172727,-58.7124044233764,
-58.2148416740257,-57.7172789246751,-57.2197161753244,-56.7221534259738,
-56.2245906766231,-55.7270279272725,-55.2294651779218,-54.7319024285712,
-54.3584128775676),.UNSPECIFIED.);
#648=B_SPLINE_CURVE_WITH_KNOTS('',3,(#37438,#37439,#37440,#37441,#37442,
#37443,#37444,#37445,#37446,#37447,#37448,#37449,#37450,#37451,#37452,#37453,
#37454,#37455,#37456,#37457,#37458,#37459,#37460,#37461,#37462,#37463,#37464,
#37465,#37466,#37467,#37468,#37469,#37470,#37471,#37472,#37473,#37474,#37475,
#37476,#37477),.UNSPECIFIED.,.F.,.F.,(4,3,3,3,3,3,3,3,3,3,3,3,3,4),(51.3818759661231,
51.7465259324672,52.2440886818179,52.7416514311685,53.2392141805192,53.7367769298698,
54.2343396792205,54.7319024285711,55.2294651779218,55.7270279272724,56.2245906766231,
56.7221534259737,57.2197161753244,57.6650612733025),.UNSPECIFIED.);
#649=B_SPLINE_CURVE_WITH_KNOTS('',3,(#37482,#37483,#37484,#37485,#37486,
#37487,#37488,#37489,#37490,#37491,#37492,#37493,#37494,#37495,#37496,#37497,
#37498,#37499,#37500,#37501,#37502,#37503,#37504,#37505,#37506,#37507,#37508,
#37509,#37510,#37511,#37512,#37513,#37514,#37515,#37516,#37517,#37518,#37519,
#37520,#37521,#37522,#37523,#37524),.UNSPECIFIED.,.F.,.F.,(4,3,3,3,3,3,
3,3,3,3,3,3,3,3,4),(-66.9247834919267,-66.6734084129867,-66.1758456636361,
-65.6782829142854,-65.1807201649348,-64.6831574155841,-64.1855946662335,
-63.6880319168828,-63.1904691675322,-62.6929064181815,-62.1953436688309,
-61.6977809194803,-61.2002181701296,-60.702655420779,-60.641598184747),
 .UNSPECIFIED.);
#650=B_SPLINE_CURVE_WITH_KNOTS('',3,(#37525,#37526,#37527,#37528,#37529,
#37530,#37531,#37532,#37533,#37534,#37535,#37536,#37537,#37538,#37539,#37540,
#37541,#37542,#37543,#37544,#37545,#37546,#37547,#37548,#37549,#37550,#37551,
#37552,#37553,#37554,#37555,#37556,#37557,#37558,#37559,#37560,#37561,#37562,
#37563,#37564,#37565,#37566,#37567),.UNSPECIFIED.,.F.,.F.,(4,3,3,3,3,3,
3,3,3,3,3,3,3,3,4),(57.6650612733025,57.717278924675,58.2148416740257,58.7124044233763,
59.2099671727269,59.7075299220776,60.2050926714282,60.7026554207789,61.2002181701295,
61.6977809194802,62.1953436688308,62.6929064181815,63.1904691675321,63.6880319168828,
63.9482465804822),.UNSPECIFIED.);
#651=B_SPLINE_CURVE_WITH_KNOTS('',3,(#37572,#37573,#37574,#37575,#37576,
#37577,#37578,#37579,#37580,#37581,#37582,#37583,#37584,#37585,#37586,#37587,
#37588,#37589,#37590,#37591,#37592,#37593,#37594,#37595,#37596,#37597,#37598,
#37599,#37600,#37601,#37602,#37603,#37604,#37605,#37606,#37607,#37608,#37609,
#37610,#37611,#37612,#37613,#37614),.UNSPECIFIED.,.F.,.F.,(4,3,3,3,3,3,
3,3,3,3,3,3,3,3,4),(-73.2079687991064,-73.1417241545451,-72.6441614051945,
-72.1465986558438,-71.6490359064932,-71.1514731571425,-70.6539104077919,
-70.1563476584412,-69.6587849090906,-69.1612221597399,-68.6636594103893,
-68.1660966610387,-67.668533911688,-67.1709711623374,-66.9247834919267),
 .UNSPECIFIED.);
#652=B_SPLINE_CURVE_WITH_KNOTS('',3,(#37615,#37616,#37617,#37618,#37619,
#37620,#37621,#37622,#37623,#37624,#37625,#37626,#37627,#37628,#37629,#37630,
#37631,#37632,#37633,#37634,#37635,#37636,#37637,#37638,#37639,#37640,#37641,
#37642,#37643,#37644,#37645,#37646,#37647,#37648,#37649,#37650,#37651,#37652,
#37653,#37654,#37655,#37656,#37657),.UNSPECIFIED.,.F.,.F.,(4,3,3,3,3,3,
3,3,3,3,3,3,3,3,4),(63.9482465804822,64.1855946662334,64.6831574155841,
65.1807201649347,65.6782829142853,66.175845663636,66.6734084129866,67.1709711623373,
67.6685339116879,68.1660966610386,68.6636594103892,69.1612221597399,69.6587849090905,
70.1563476584412,70.2314318876619),.UNSPECIFIED.);
#653=B_SPLINE_CURVE_WITH_KNOTS('',3,(#37662,#37663,#37664,#37665,#37666,
#37667,#37668,#37669,#37670,#37671,#37672,#37673,#37674,#37675,#37676,#37677,
#37678,#37679,#37680,#37681,#37682,#37683,#37684,#37685,#37686,#37687,#37688,
#37689,#37690,#37691,#37692,#37693,#37694,#37695,#37696,#37697,#37698,#37699,
#37700,#37701),.UNSPECIFIED.,.F.,.F.,(4,3,3,3,3,3,3,3,3,3,3,3,3,4),(-79.4911541062858,
-79.1124771467529,-78.6149143974022,-78.1173516480516,-77.6197888987009,
-77.1222261493503,-76.6246633999996,-76.127100650649,-75.6295379012984,
-75.1319751519477,-74.6344124025971,-74.1368496532464,-73.6392869038958,
-73.2079687991064),.UNSPECIFIED.);
#654=B_SPLINE_CURVE_WITH_KNOTS('',3,(#37702,#37703,#37704,#37705,#37706,
#37707,#37708,#37709,#37710,#37711,#37712,#37713,#37714,#37715,#37716,#37717,
#37718,#37719,#37720,#37721,#37722,#37723,#37724,#37725,#37726,#37727,#37728,
#37729,#37730,#37731,#37732,#37733,#37734,#37735,#37736,#37737,#37738,#37739,
#37740,#37741),.UNSPECIFIED.,.F.,.F.,(4,3,3,3,3,3,3,3,3,3,3,3,3,4),(70.2314318876619,
70.6539104077918,71.1514731571425,71.6490359064931,72.1465986558438,72.6441614051944,
73.141724154545,73.6392869038957,74.1368496532463,74.634412402597,75.1319751519476,
75.6295379012983,76.1271006506489,76.5146171948413),.UNSPECIFIED.);
#655=B_SPLINE_CURVE_WITH_KNOTS('',3,(#37747,#37748,#37749,#37750),
 .UNSPECIFIED.,.F.,.F.,(4,4),(91.1061869541039,91.1475924660972),
 .UNSPECIFIED.);
#656=B_SPLINE_CURVE_WITH_KNOTS('',3,(#37756,#37757,#37758,#37759,#37760,
#37761,#37762,#37763,#37764,#37765,#37766,#37767,#37768,#37769,#37770,#37771),
 .UNSPECIFIED.,.F.,.F.,(4,1,1,1,1,1,1,1,1,1,1,1,1,4),(84.8230016469245,
85.2543197517139,85.7518825010645,86.2494452504152,86.7470079997658,87.2445707491165,
87.7421334984671,88.2396962478177,88.7372589971684,89.234821746519,89.7323844958697,
90.2299472452203,90.727509994571,91.1061869541039),.UNSPECIFIED.);
#657=B_SPLINE_CURVE_WITH_KNOTS('',3,(#37774,#37775,#37776,#37777,#37778,
#37779,#37780,#37781,#37782,#37783,#37784,#37785,#37786,#37787),
 .UNSPECIFIED.,.F.,.F.,(4,1,1,1,1,1,1,1,1,1,1,4),(84.8230016469245,84.9330478520825,
85.4306106014332,85.9281733507838,86.4257361001345,86.9232988494851,87.4208615988357,
87.9184243481864,88.415987097537,88.9135498468877,89.4111125962383,89.908675345589),
 .UNSPECIFIED.);
#658=B_SPLINE_CURVE_WITH_KNOTS('',3,(#37792,#37793,#37794,#37795,#37796,
#37797,#37798,#37799,#37800,#37801,#37802,#37803,#37804,#37805,#37806,#37807,
#37808),.UNSPECIFIED.,.F.,.F.,(4,1,1,1,1,1,1,1,1,1,1,1,1,1,4),(78.5398163397448,
78.7860040101555,79.2835667595061,79.7811295088568,80.2786922582074,80.776255007558,
81.2738177569087,81.7713805062593,82.26894325561,82.7665060049606,83.2640687543113,
83.7616315036619,84.2591942530126,84.7567570023632,84.8230016469245),
 .UNSPECIFIED.);
#659=B_SPLINE_CURVE_WITH_KNOTS('',3,(#37809,#37810,#37811,#37812,#37813,
#37814,#37815,#37816,#37817,#37818,#37819,#37820,#37821,#37822,#37823,#37824),
 .UNSPECIFIED.,.F.,.F.,(4,1,1,1,1,1,1,1,1,1,1,1,1,4),(78.5398163397448,
78.9622948598747,79.4598576092254,79.957420358576,80.4549831079267,80.9525458572773,
81.450108606628,81.9476713559786,82.4452341053293,82.9427968546799,83.4403596040306,
83.9379223533812,84.4354851027319,84.8230016469245),.UNSPECIFIED.);
#660=B_SPLINE_CURVE_WITH_KNOTS('',3,(#37829,#37830,#37831,#37832,#37833,
#37834,#37835,#37836,#37837,#37838,#37839,#37840,#37841,#37842,#37843,#37844,
#37845),.UNSPECIFIED.,.F.,.F.,(4,1,1,1,1,1,1,1,1,1,1,1,1,1,4),(72.2566310325652,
72.317688268597,72.8152510179477,73.3128137672983,73.810376516649,74.3079392659996,
74.8055020153503,75.3030647647009,75.8006275140516,76.2981902634022,76.7957530127529,
77.2933157621035,77.7908785114542,78.2884412608048,78.5398163397448),
 .UNSPECIFIED.);
#661=B_SPLINE_CURVE_WITH_KNOTS('',3,(#37846,#37847,#37848,#37849,#37850,
#37851,#37852,#37853,#37854,#37855,#37856,#37857,#37858,#37859,#37860,#37861,
#37862),.UNSPECIFIED.,.F.,.F.,(4,1,1,1,1,1,1,1,1,1,1,1,1,1,4),(72.2566310325651,
72.4939791183163,72.991541867667,73.4891046170176,73.9866673663683,74.4842301157189,
74.9817928650696,75.4793556144202,75.9769183637709,76.4744811131215,76.9720438624722,
77.4696066118228,77.9671693611735,78.4647321105241,78.5398163397448),
 .UNSPECIFIED.);
#662=B_SPLINE_CURVE_WITH_KNOTS('',3,(#37867,#37868,#37869,#37870,#37871,
#37872,#37873,#37874,#37875,#37876,#37877,#37878,#37879,#37880,#37881,#37882),
 .UNSPECIFIED.,.F.,.F.,(4,1,1,1,1,1,1,1,1,1,1,1,1,4),(65.9734457253857,
66.3469352763893,66.8444980257399,67.3420607750906,67.8396235244412,68.3371862737919,
68.8347490231425,69.3323117724932,69.8298745218438,70.3274372711945,70.8250000205451,
71.3225627698958,71.8201255192464,72.2566310325652),.UNSPECIFIED.);
#663=B_SPLINE_CURVE_WITH_KNOTS('',3,(#37883,#37884,#37885,#37886,#37887,
#37888,#37889,#37890,#37891,#37892,#37893,#37894,#37895,#37896,#37897,#37898,
#37899),.UNSPECIFIED.,.F.,.F.,(4,1,1,1,1,1,1,1,1,1,1,1,1,1,4),(65.9734457253857,
66.0256633767579,66.5232261261086,67.0207888754592,67.5183516248099,68.0159143741605,
68.5134771235112,69.0110398728618,69.5086026222125,70.0061653715631,70.5037281209138,
71.0012908702644,71.498853619615,71.9964163689657,72.2566310325651),
 .UNSPECIFIED.);
#664=B_SPLINE_CURVE_WITH_KNOTS('',3,(#37904,#37905,#37906,#37907,#37908,
#37909,#37910,#37911,#37912,#37913,#37914,#37915,#37916,#37917,#37918,#37919,
#37920),.UNSPECIFIED.,.F.,.F.,(4,1,1,1,1,1,1,1,1,1,1,1,1,1,4),(59.690260418206,
59.8786195348309,60.3761822841815,60.8737450335322,61.3713077828828,61.8688705322335,
62.3664332815841,62.8639960309348,63.3615587802854,63.859121529636,64.3566842789867,
64.8542470283373,65.351809777688,65.8493725270386,65.9734457253857),
 .UNSPECIFIED.);
#665=B_SPLINE_CURVE_WITH_KNOTS('',3,(#37921,#37922,#37923,#37924,#37925,
#37926,#37927,#37928,#37929,#37930,#37931,#37932,#37933,#37934,#37935,#37936),
 .UNSPECIFIED.,.F.,.F.,(4,1,1,1,1,1,1,1,1,1,1,1,1,4),(59.690260418206,60.0549103845502,
60.5524731339008,61.0500358832515,61.5475986326021,62.0451613819528,62.5427241313034,
63.0402868806541,63.5378496300047,64.0354123793553,64.532975128706,65.0305378780566,
65.5281006274073,65.9734457253857),.UNSPECIFIED.);
#666=B_SPLINE_CURVE_WITH_KNOTS('',3,(#37941,#37942,#37943,#37944,#37945,
#37946,#37947,#37948,#37949,#37950,#37951,#37952,#37953,#37954,#37955,#37956,
#37957),.UNSPECIFIED.,.F.,.F.,(4,1,1,1,1,1,1,1,1,1,1,1,1,1,4),(53.4070751110263,
53.4103037932725,53.9078665426231,54.4054292919737,54.9029920413244,55.400554790675,
55.8981175400257,56.3956802893763,56.893243038727,57.3908057880776,57.8883685374283,
58.3859312867789,58.8834940361296,59.3810567854802,59.690260418206),
 .UNSPECIFIED.);
#667=B_SPLINE_CURVE_WITH_KNOTS('',3,(#37958,#37959,#37960,#37961,#37962,
#37963,#37964,#37965,#37966,#37967,#37968,#37969,#37970,#37971,#37972,#37973,
#37974),.UNSPECIFIED.,.F.,.F.,(4,1,1,1,1,1,1,1,1,1,1,1,1,1,4),(53.4070751110263,
53.5865946429918,54.0841573923424,54.5817201416931,55.0792828910437,55.5768456403944,
56.074408389745,56.5719711390957,57.0695338884463,57.5670966377969,58.0646593871476,
58.5622221364982,59.0597848858489,59.5573476351995,59.690260418206),
 .UNSPECIFIED.);
#668=B_SPLINE_CURVE_WITH_KNOTS('',3,(#37979,#37980,#37981,#37982,#37983,
#37984,#37985,#37986,#37987,#37988,#37989,#37990,#37991,#37992,#37993,#37994),
 .UNSPECIFIED.,.F.,.F.,(4,1,1,1,1,1,1,1,1,1,1,1,1,4),(47.1238898038469,
47.4395508010647,47.9371135504153,48.434676299766,48.9322390491166,49.4298017984673,
49.9273645478179,50.4249272971686,50.9224900465192,51.4200527958699,51.9176155452205,
52.4151782945712,52.9127410439218,53.4070751110263),.UNSPECIFIED.);
#669=B_SPLINE_CURVE_WITH_KNOTS('',3,(#37995,#37996,#37997,#37998,#37999,
#38000,#38001,#38002,#38003,#38004,#38005,#38006,#38007,#38008,#38009,#38010),
 .UNSPECIFIED.,.F.,.F.,(4,1,1,1,1,1,1,1,1,1,1,1,1,4),(47.1238898038469,
47.615841650784,48.1134044001347,48.6109671494853,49.108529898836,49.6060926481866,
50.1036553975372,50.6012181468879,51.0987808962385,51.5963436455892,52.0939063949398,
52.5914691442905,53.0890318936411,53.4070751110263),.UNSPECIFIED.);
#670=B_SPLINE_CURVE_WITH_KNOTS('',3,(#38015,#38016,#38017,#38018,#38019,
#38020,#38021,#38022,#38023,#38024,#38025,#38026,#38027,#38028,#38029,#38030,
#38031),.UNSPECIFIED.,.F.,.F.,(4,1,1,1,1,1,1,1,1,1,1,1,1,1,4),(40.8407044966672,
40.9712350595063,41.4687978088569,41.9663605582076,42.4639233075582,42.9614860569089,
43.4590488062595,43.9566115556102,44.4541743049608,44.9517370543115,45.4492998036621,
45.9468625530127,46.4444253023634,46.941988051714,47.1238898038469),
 .UNSPECIFIED.);
#671=B_SPLINE_CURVE_WITH_KNOTS('',3,(#38032,#38033,#38034,#38035,#38036,
#38037,#38038,#38039,#38040,#38041,#38042,#38043,#38044,#38045,#38046,#38047,
#38048),.UNSPECIFIED.,.F.,.F.,(4,1,1,1,1,1,1,1,1,1,1,1,1,1,4),(40.8407044966672,
41.1475259092256,41.6450886585762,42.1426514079269,42.6402141572775,43.1377769066282,
43.6353396559788,44.1329024053295,44.6304651546801,45.1280279040308,45.6255906533814,
46.1231534027321,46.6207161520827,47.1182789014334,47.1238898038469),
 .UNSPECIFIED.);
#672=B_SPLINE_CURVE_WITH_KNOTS('',3,(#38053,#38054,#38055,#38056,#38057,
#38058,#38059,#38060,#38061,#38062,#38063,#38064,#38065,#38066,#38067,#38068),
 .UNSPECIFIED.,.F.,.F.,(4,1,1,1,1,1,1,1,1,1,1,1,1,4),(34.5575191894878,
35.0004820672985,35.4980448166492,35.9956075659998,36.4931703153505,36.9907330647011,
37.4882958140517,37.9858585634024,38.483421312753,38.9809840621037,39.4785468114543,
39.976109560805,40.4736723101556,40.8407044966672),.UNSPECIFIED.);
#673=B_SPLINE_CURVE_WITH_KNOTS('',3,(#38069,#38070,#38071,#38072,#38073,
#38074,#38075,#38076,#38077,#38078,#38079,#38080,#38081,#38082,#38083,#38084,
#38085),.UNSPECIFIED.,.F.,.F.,(4,1,1,1,1,1,1,1,1,1,1,1,1,1,4),(34.5575191894878,
34.6792101676672,35.1767729170178,35.6743356663685,36.1718984157191,36.6694611650698,
37.1670239144204,37.6645866637711,38.1621494131217,38.6597121624724,39.157274911823,
39.6548376611737,40.1524004105243,40.649963159875,40.8407044966672),
 .UNSPECIFIED.);
#674=B_SPLINE_CURVE_WITH_KNOTS('',3,(#38090,#38091,#38092,#38093,#38094,
#38095,#38096,#38097,#38098,#38099,#38100,#38101,#38102,#38103,#38104,#38105,
#38106),.UNSPECIFIED.,.F.,.F.,(4,1,1,1,1,1,1,1,1,1,1,1,1,1,4),(28.2743338823081,
28.5321663257401,29.0297290750907,29.5272918244414,30.024854573792,30.5224173231427,
31.0199800724933,31.517542821844,32.0151055711946,32.5126683205453,33.0102310698959,
33.5077938192466,34.0053565685972,34.5029193179479,34.5575191894878),
 .UNSPECIFIED.);
#675=B_SPLINE_CURVE_WITH_KNOTS('',3,(#38107,#38108,#38109,#38110,#38111,
#38112,#38113,#38114,#38115,#38116,#38117,#38118,#38119,#38120,#38121,#38122),
 .UNSPECIFIED.,.F.,.F.,(4,1,1,1,1,1,1,1,1,1,1,1,1,4),(28.2743338823081,
28.7084571754594,29.2060199248101,29.7035826741607,30.2011454235114,30.698708172862,
31.1962709222127,31.6938336715633,32.191396420914,32.6889591702646,33.1865219196153,
33.6840846689659,34.1816474183166,34.5575191894878),.UNSPECIFIED.);
#676=B_SPLINE_CURVE_WITH_KNOTS('',3,(#38127,#38128,#38129,#38130,#38131,
#38132,#38133,#38134,#38135,#38136,#38137,#38138,#38139,#38140,#38141,#38142,
#38143),.UNSPECIFIED.,.F.,.F.,(4,1,1,1,1,1,1,1,1,1,1,1,1,1,4),(21.9911485751284,
22.0638505841817,22.5614133335323,23.058976082883,23.5565388322336,24.0541015815843,
24.5516643309349,25.0492270802856,25.5467898296362,26.0443525789869,26.5419153283375,
27.0394780776882,27.5370408270388,28.0346035763895,28.2743338823081),
 .UNSPECIFIED.);
#677=B_SPLINE_CURVE_WITH_KNOTS('',3,(#38144,#38145,#38146,#38147,#38148,
#38149,#38150,#38151,#38152,#38153,#38154,#38155,#38156,#38157,#38158,#38159,
#38160),.UNSPECIFIED.,.F.,.F.,(4,1,1,1,1,1,1,1,1,1,1,1,1,1,4),(21.9911485751284,
22.240141433901,22.7377041832517,23.2352669326023,23.732829681953,24.2303924313036,
24.7279551806543,25.2255179300049,25.7230806793556,26.2206434287062,26.7182061780569,
27.2157689274075,27.7133316767581,28.2108944261088,28.2743338823081),
 .UNSPECIFIED.);
#678=B_SPLINE_CURVE_WITH_KNOTS('',3,(#38165,#38166,#38167,#38168,#38169,
#38170,#38171,#38172,#38173,#38174,#38175,#38176,#38177,#38178,#38179,#38180),
 .UNSPECIFIED.,.F.,.F.,(4,1,1,1,1,1,1,1,1,1,1,1,1,4),(15.707963267949,16.0930975919739,
16.5906603413246,17.0882230906752,17.5857858400259,18.0833485893765,18.5809113387272,
19.0784740880778,19.5760368374285,20.0735995867791,20.5711623361297,21.0687250854804,
21.566287834831,21.9911485751284),.UNSPECIFIED.);
#679=B_SPLINE_CURVE_WITH_KNOTS('',3,(#38181,#38182,#38183,#38184,#38185,
#38186,#38187,#38188,#38189,#38190,#38191,#38192,#38193,#38194,#38195,#38196,
#38197),.UNSPECIFIED.,.F.,.F.,(4,1,1,1,1,1,1,1,1,1,1,1,1,1,4),(15.707963267949,
15.7718256923426,16.2693884416933,16.7669511910439,17.2645139403946,17.7620766897452,
18.2596394390959,18.7572021884465,19.2547649377972,19.7523276871478,20.2498904364984,
20.7474531858491,21.2450159351997,21.7425786845504,21.9911485751284),
 .UNSPECIFIED.);
#680=B_SPLINE_CURVE_WITH_KNOTS('',3,(#39121,#39122,#39123,#39124,#39125,
#39126,#39127,#39128,#39129,#39130,#39131,#39132,#39133,#39134,#39135,#39136,
#39137,#39138,#39139,#39140,#39141,#39142,#39143,#39144,#39145,#39146,#39147,
#39148,#39149,#39150,#39151,#39152,#39153,#39154,#39155,#39156,#39157,#39158,
#39159,#39160,#39161,#39162,#39163,#39164,#39165,#39166,#39167,#39168,#39169,
#39170,#39171,#39172,#39173,#39174,#39175,#39176,#39177,#39178,#39179,#39180,
#39181,#39182,#39183,#39184,#39185,#39186,#39187,#39188,#39189,#39190,#39191,
#39192,#39193,#39194,#39195,#39196,#39197,#39198,#39199,#39200,#39201,#39202,
#39203,#39204,#39205,#39206,#39207,#39208,#39209,#39210,#39211,#39212,#39213,
#39214,#39215,#39216,#39217,#39218,#39219,#39220),.UNSPECIFIED.,.F.,.F.,
(4,3,3,3,3,3,3,3,3,3,3,3,3,3,3,3,3,3,3,3,3,3,3,3,3,3,3,3,3,3,3,3,3,4),(-0.965990216419489,
-0.927769800274492,-0.884036457391411,-0.859296340292785,-0.841593944822978,
-0.834687190942105,-0.791436271578584,-0.748447260876285,-0.715784640354957,
-0.71037803066556,-0.686115520602401,-0.643612953198282,-0.600900815509313,
-0.56335340930662,-0.5351928546546,-0.529195526613789,-0.487304945489095,
-0.450711190698541,-0.408716440645001,-0.366944220009338,-0.350749948869511,
-0.345333544484853,-0.304097381748682,-0.263026243379112,-0.221955105009542,
-0.19421071688335,-0.181344115531761,-0.173002718621388,-0.167235292303527,
-0.125426469227645,-0.0849353464330531,-0.0447936733152677,-0.00549740928954664,
0.),.UNSPECIFIED.);
#681=B_SPLINE_CURVE_WITH_KNOTS('',3,(#39221,#39222,#39223,#39224,#39225,
#39226,#39227,#39228,#39229,#39230,#39231,#39232,#39233,#39234,#39235,#39236,
#39237,#39238,#39239,#39240,#39241,#39242),.UNSPECIFIED.,.F.,.F.,(4,3,3,
3,3,3,3,4),(76.5146171948413,76.6246633999996,77.1222261493502,77.6197888987009,
78.1173516480515,78.6149143974022,79.1124771467528,79.5325596182791),
 .UNSPECIFIED.);
#682=B_SPLINE_CURVE_WITH_KNOTS('',3,(#39244,#39245,#39246,#39247,#39248,
#39249,#39250,#39251,#39252,#39253,#39254,#39255,#39256,#39257,#39258,#39259,
#39260,#39261,#39262,#39263,#39264,#39265,#39266,#39267,#39268,#39269,#39270,
#39271,#39272,#39273,#39274,#39275,#39276,#39277,#39278,#39279,#39280,#39281,
#39282,#39283,#39284,#39285,#39286,#39287,#39288,#39289,#39290,#39291,#39292,
#39293,#39294,#39295,#39296,#39297,#39298,#39299,#39300,#39301,#39302,#39303,
#39304,#39305,#39306,#39307,#39308,#39309,#39310,#39311,#39312,#39313,#39314,
#39315,#39316,#39317,#39318,#39319,#39320,#39321,#39322,#39323,#39324,#39325,
#39326,#39327,#39328,#39329,#39330,#39331,#39332,#39333,#39334,#39335,#39336,
#39337,#39338,#39339,#39340,#39341,#39342,#39343,#39344,#39345,#39346),
 .UNSPECIFIED.,.F.,.F.,(4,3,3,3,3,3,3,3,3,3,3,3,3,3,3,3,3,3,3,3,3,3,3,3,
3,3,3,3,3,3,3,3,3,3,4),(-0.968477696161936,-0.934343797368491,-0.894226277483961,
-0.871339551305548,-0.855822539845121,-0.849949261747619,-0.809088844038457,
-0.768077284767626,-0.751532687618365,-0.742536577619449,-0.734141406691584,
-0.711132468056658,-0.670310088690189,-0.628911606809814,-0.591876013787433,
-0.564099319020647,-0.556019424396184,-0.51377696547059,-0.48076923472029,
-0.438727307185997,-0.396438608516356,-0.380090389242943,-0.373382824706804,
-0.330696753861742,-0.287182914486212,-0.243669075110682,-0.213210440721847,
-0.199884788176731,-0.191537541849349,-0.185963421418205,-0.14306631876944,
-0.0993786244214358,-0.0556350222056884,-0.0124004253203635,0.),
 .UNSPECIFIED.);
#683=B_SPLINE_CURVE_WITH_KNOTS('',3,(#39347,#39348,#39349,#39350,#39351,
#39352,#39353,#39354,#39355,#39356,#39357,#39358,#39359,#39360),
 .UNSPECIFIED.,.F.,.F.,(4,1,1,1,1,1,1,1,1,1,1,4),(10.3761157273099,10.7961981988362,
11.2937609481868,11.7913236975375,12.2888864468881,12.7864491962387,13.2840119455894,
13.78157469494,14.2791374442907,14.7767001936413,15.274262942992,15.707963267949),
 .UNSPECIFIED.);
#684=B_SPLINE_CURVE_WITH_KNOTS('',3,(#39366,#39367,#39368,#39369,#39370,
#39371,#39372,#39373,#39374,#39375,#39376,#39377,#39378,#39379,#39380,#39381,
#39382,#39383,#39384,#39385,#39386,#39387,#39388,#39389,#39390,#39391,#39392,
#39393,#39394,#39395,#39396,#39397,#39398,#39399,#39400,#39401,#39402,#39403,
#39404,#39405,#39406,#39407,#39408,#39409,#39410,#39411,#39412,#39413,#39414,
#39415,#39416,#39417,#39418,#39419,#39420,#39421,#39422,#39423,#39424,#39425,
#39426,#39427,#39428,#39429,#39430,#39431,#39432,#39433,#39434,#39435,#39436,
#39437,#39438,#39439,#39440,#39441,#39442,#39443,#39444,#39445,#39446,#39447,
#39448,#39449,#39450,#39451,#39452,#39453,#39454,#39455,#39456,#39457,#39458,
#39459,#39460,#39461,#39462,#39463,#39464,#39465),.UNSPECIFIED.,.F.,.F.,
(4,3,3,3,3,3,3,3,3,3,3,3,3,3,3,3,3,3,3,3,3,3,3,3,3,3,3,3,3,3,3,3,3,4),(-0.965990216419325,
-0.927769800274406,-0.884036457390911,-0.85929634029234,-0.841593944851099,
-0.834687190844098,-0.791436271424871,-0.74844726071717,-0.715784639906417,
-0.710378030072974,-0.686115520602341,-0.643612953183401,-0.600900815160043,
-0.563353409044655,-0.535192854458115,-0.529195526619761,-0.487304944852415,
-0.450711190698493,-0.408716441214337,-0.366944223277963,-0.350749948031817,
-0.345333543994406,-0.304097381804349,-0.263026243406926,-0.221955105009502,
-0.194210716883314,-0.181344115695033,-0.1730027188061,-0.167235292295272,
-0.125426469221454,-0.0849353441299271,-0.0447936662663009,-0.00549739522862838,
0.),.UNSPECIFIED.);
#685=B_SPLINE_CURVE_WITH_KNOTS('',3,(#39468,#39469,#39470,#39471,#39472,
#39473,#39474,#39475,#39476,#39477,#39478,#39479),.UNSPECIFIED.,.F.,.F.,
(4,1,1,1,1,1,1,1,1,4),(11.6150328478181,12.1125955971687,12.6101583465194,
13.10772109587,13.6052838452207,14.1028465945713,14.600409343922,15.0979720932726,
15.5955348426233,15.707963267949),.UNSPECIFIED.);
#686=B_SPLINE_CURVE_WITH_KNOTS('',3,(#40149,#40150,#40151,#40152,#40153,
#40154,#40155,#40156,#40157,#40158,#40159,#40160,#40161,#40162,#40163,#40164,
#40165,#40166,#40167,#40168,#40169,#40170,#40171,#40172,#40173,#40174,#40175,
#40176,#40177,#40178,#40179,#40180,#40181,#40182,#40183,#40184,#40185,#40186,
#40187,#40188,#40189,#40190,#40191,#40192,#40193,#40194,#40195,#40196,#40197,
#40198,#40199,#40200,#40201,#40202,#40203,#40204,#40205,#40206,#40207,#40208,
#40209,#40210,#40211,#40212,#40213,#40214,#40215,#40216,#40217,#40218,#40219,
#40220,#40221,#40222,#40223,#40224,#40225,#40226,#40227,#40228,#40229,#40230,
#40231,#40232,#40233,#40234,#40235,#40236,#40237,#40238,#40239,#40240,#40241,
#40242,#40243,#40244,#40245,#40246,#40247,#40248,#40249,#40250,#40251),
 .UNSPECIFIED.,.F.,.F.,(4,3,3,3,3,3,3,3,3,3,3,3,3,3,3,3,3,3,3,3,3,3,3,3,
3,3,3,3,3,3,3,3,3,3,4),(-0.968477696161912,-0.934343797368481,-0.894226277807462,
-0.871339551588618,-0.85582253996102,-0.849949261921466,-0.80908884435452,
-0.768077285019809,-0.751532687806619,-0.742536577935966,-0.734141406720873,
-0.711132468056709,-0.670310088248261,-0.628911606247961,-0.591876013366052,
-0.564099318704621,-0.556019424467619,-0.51377696546797,-0.480769234720327,
-0.438727306412881,-0.39643860794713,-0.380090388267127,-0.373382824556077,
-0.330696752907007,-0.287182914008866,-0.243669075110725,-0.213210440721885,
-0.199884788176767,-0.191537541538495,-0.185963421107643,-0.143066322667477,
-0.099378629805352,-0.0556350264235498,-0.0124004243521518,0.),
 .UNSPECIFIED.);
#687=B_SPLINE_CURVE_WITH_KNOTS('',3,(#40252,#40253,#40254,#40255,#40256,
#40257,#40258,#40259,#40260,#40261,#40262,#40263,#40264,#40265,#40266,#40267),
 .UNSPECIFIED.,.F.,.F.,(4,3,3,3,3,4),(-81.6002908935061,-81.1027281441555,
-80.6051653948048,-80.1076026454542,-79.6100398961035,-79.4911541062858),
 .UNSPECIFIED.);
#688=B_SPLINE_CURVE_WITH_KNOTS('',3,(#40645,#40646,#40647,#40648,#40649,
#40650,#40651,#40652,#40653,#40654),.UNSPECIFIED.,.F.,.F.,(4,3,3,4),(-4.09293042013065,
-3.99861591915004,-2.99896193936253,-2.06773127522702),.UNSPECIFIED.);
#689=B_SPLINE_CURVE_WITH_KNOTS('',3,(#40657,#40658,#40659,#40660,#40661,
#40662,#40663,#40664,#40665,#40666),.UNSPECIFIED.,.F.,.F.,(4,3,3,4),(0.,
0.499826989893744,0.999653979787498,1.11639350868611),.UNSPECIFIED.);
#690=B_SPLINE_CURVE_WITH_KNOTS('',3,(#40671,#40672,#40673,#40674,#40675,
#40676,#40677,#40678,#40679,#40680,#40681,#40682,#40683,#40684,#40685,#40686,
#40687,#40688,#40689,#40690,#40691,#40692),.UNSPECIFIED.,.F.,.F.,(4,3,3,
3,3,3,3,4),(-10.3761157273102,-9.99653979787509,-8.99688581808759,-7.99723183830008,
-6.99757785851257,-5.99792387872506,-4.99826989893755,-4.09293042013065),
 .UNSPECIFIED.);
#691=B_SPLINE_CURVE_WITH_KNOTS('',3,(#40693,#40694,#40695,#40696,#40697,
#40698,#40699,#40700,#40701,#40702,#40703,#40704,#40705,#40706,#40707,#40708,
#40709,#40710,#40711,#40712,#40713,#40714),.UNSPECIFIED.,.F.,.F.,(4,3,3,
3,3,3,3,4),(1.11639350868611,1.99930795957501,2.99896193936252,3.99861591915003,
4.99826989893754,5.99792387872506,6.99757785851257,7.39957881586569),
 .UNSPECIFIED.);
#692=B_SPLINE_CURVE_WITH_KNOTS('',3,(#40719,#40720,#40721,#40722,#40723,
#40724,#40725,#40726,#40727,#40728,#40729,#40730,#40731,#40732,#40733,#40734,
#40735,#40736,#40737,#40738,#40739,#40740),.UNSPECIFIED.,.F.,.F.,(4,3,3,
3,3,3,3,4),(-16.6593010344898,-15.9944636766002,-14.9948096968126,-13.9951557170251,
-12.9955017372376,-11.9958477574501,-10.9961937776626,-10.3761157273102),
 .UNSPECIFIED.);
#693=B_SPLINE_CURVE_WITH_KNOTS('',3,(#40741,#40742,#40743,#40744,#40745,
#40746,#40747,#40748,#40749,#40750,#40751,#40752,#40753,#40754,#40755,#40756,
#40757,#40758,#40759,#40760,#40761,#40762),.UNSPECIFIED.,.F.,.F.,(4,3,3,
3,3,3,3,4),(7.39957881586569,7.99723183830008,8.99688581808759,9.9965397978751,
10.9961937776626,11.9958477574501,12.9955017372376,13.6827641230453),
 .UNSPECIFIED.);
#694=B_SPLINE_CURVE_WITH_KNOTS('',3,(#40767,#40768,#40769,#40770,#40771,
#40772,#40773,#40774,#40775,#40776,#40777,#40778,#40779,#40780,#40781,#40782,
#40783,#40784,#40785,#40786,#40787,#40788),.UNSPECIFIED.,.F.,.F.,(4,3,3,
3,3,3,3,4),(-22.9424863416694,-21.9923875553252,-20.9927335755377,-19.9930795957502,
-18.9934256159627,-17.9937716361752,-16.9941176563877,-16.6593010344898),
 .UNSPECIFIED.);
#695=B_SPLINE_CURVE_WITH_KNOTS('',3,(#40789,#40790,#40791,#40792,#40793,
#40794,#40795,#40796,#40797,#40798,#40799,#40800,#40801,#40802,#40803,#40804,
#40805,#40806,#40807,#40808,#40809,#40810),.UNSPECIFIED.,.F.,.F.,(4,3,3,
3,3,3,3,4),(13.6827641230453,13.9951557170251,14.9948096968126,15.9944636766002,
16.9941176563877,17.9937716361752,18.9934256159627,19.9659494302249),
 .UNSPECIFIED.);
#696=B_SPLINE_CURVE_WITH_KNOTS('',3,(#40815,#40816,#40817,#40818,#40819,
#40820,#40821,#40822,#40823,#40824,#40825,#40826,#40827,#40828,#40829,#40830,
#40831,#40832,#40833,#40834,#40835,#40836,#40837,#40838,#40839),
 .UNSPECIFIED.,.F.,.F.,(4,3,3,3,3,3,3,3,4),(-29.225671648849,-28.9899654138378,
-27.9903114340503,-26.9906574542627,-25.9910034744752,-24.9913494946877,
-23.9916955149002,-22.9920415351127,-22.9424863416694),.UNSPECIFIED.);
#697=B_SPLINE_CURVE_WITH_KNOTS('',3,(#40840,#40841,#40842,#40843,#40844,
#40845,#40846,#40847,#40848,#40849,#40850,#40851,#40852,#40853,#40854,#40855,
#40856,#40857,#40858,#40859,#40860,#40861,#40862,#40863,#40864),
 .UNSPECIFIED.,.F.,.F.,(4,3,3,3,3,3,3,3,4),(19.9659494302249,19.9930795957502,
20.9927335755377,21.9923875553252,22.9920415351127,23.9916955149002,24.9913494946877,
25.9910034744752,26.2491347374045),.UNSPECIFIED.);
#698=B_SPLINE_CURVE_WITH_KNOTS('',3,(#40869,#40870,#40871,#40872,#40873,
#40874,#40875,#40876,#40877,#40878,#40879,#40880,#40881,#40882,#40883,#40884,
#40885,#40886,#40887,#40888,#40889,#40890),.UNSPECIFIED.,.F.,.F.,(4,3,3,
3,3,3,3,4),(-35.5088569560286,-34.9878892925628,-33.9882353127753,-32.9885813329878,
-31.9889273532003,-30.9892733734128,-29.9896193936253,-29.225671648849),
 .UNSPECIFIED.);
#699=B_SPLINE_CURVE_WITH_KNOTS('',3,(#40891,#40892,#40893,#40894,#40895,
#40896,#40897,#40898,#40899,#40900,#40901,#40902,#40903,#40904,#40905,#40906,
#40907,#40908,#40909,#40910,#40911,#40912),.UNSPECIFIED.,.F.,.F.,(4,3,3,
3,3,3,3,4),(26.2491347374045,26.9906574542628,27.9903114340503,28.9899654138378,
29.9896193936253,30.9892733734128,31.9889273532003,32.532320044584),
 .UNSPECIFIED.);
#700=B_SPLINE_CURVE_WITH_KNOTS('',3,(#40917,#40918,#40919,#40920,#40921,
#40922,#40923,#40924,#40925,#40926,#40927,#40928,#40929,#40930,#40931,#40932,
#40933,#40934,#40935,#40936,#40937,#40938),.UNSPECIFIED.,.F.,.F.,(4,3,3,
3,3,3,3,4),(-41.7920422632082,-40.9858131712879,-39.9861591915004,-38.9865052117129,
-37.9868512319254,-36.9871972521378,-35.9875432723503,-35.5088569560286),
 .UNSPECIFIED.);
#701=B_SPLINE_CURVE_WITH_KNOTS('',3,(#40939,#40940,#40941,#40942,#40943,
#40944,#40945,#40946,#40947,#40948,#40949,#40950,#40951,#40952,#40953,#40954,
#40955,#40956,#40957,#40958,#40959,#40960),.UNSPECIFIED.,.F.,.F.,(4,3,3,
3,3,3,3,4),(32.532320044584,32.9885813329878,33.9882353127753,34.9878892925628,
35.9875432723503,36.9871972521378,37.9868512319253,38.8155053517636),
 .UNSPECIFIED.);
#702=B_SPLINE_CURVE_WITH_KNOTS('',3,(#40965,#40966,#40967,#40968,#40969,
#40970,#40971,#40972,#40973,#40974,#40975,#40976,#40977,#40978,#40979,#40980,
#40981,#40982,#40983,#40984,#40985,#40986,#40987,#40988,#40989),
 .UNSPECIFIED.,.F.,.F.,(4,3,3,3,3,3,3,3,4),(-48.0752275703878,-47.9833910298005,
-46.9837370500129,-45.9840830702254,-44.9844290904379,-43.9847751106504,
-42.9851211308629,-41.9854671510754,-41.7920422632082),.UNSPECIFIED.);
#703=B_SPLINE_CURVE_WITH_KNOTS('',3,(#40990,#40991,#40992,#40993,#40994,
#40995,#40996,#40997,#40998,#40999,#41000,#41001,#41002,#41003,#41004,#41005,
#41006,#41007,#41008,#41009,#41010,#41011,#41012,#41013,#41014),
 .UNSPECIFIED.,.F.,.F.,(4,3,3,3,3,3,3,3,4),(38.8155053517636,38.9865052117129,
39.9861591915004,40.9858131712879,41.9854671510754,42.9851211308629,43.9847751106504,
44.9844290904379,45.0986906589432),.UNSPECIFIED.);
#704=B_SPLINE_CURVE_WITH_KNOTS('',3,(#41019,#41020,#41021,#41022,#41023,
#41024,#41025,#41026,#41027,#41028,#41029,#41030,#41031,#41032,#41033,#41034,
#41035,#41036,#41037,#41038,#41039,#41040),.UNSPECIFIED.,.F.,.F.,(4,3,3,
3,3,3,3,4),(-54.3584128775673,-53.9813149085255,-52.981660928738,-51.9820069489505,
-50.982352969163,-49.9826989893755,-48.983045009588,-48.0752275703878),
 .UNSPECIFIED.);
#705=B_SPLINE_CURVE_WITH_KNOTS('',3,(#41041,#41042,#41043,#41044,#41045,
#41046,#41047,#41048,#41049,#41050,#41051,#41052,#41053,#41054,#41055,#41056,
#41057,#41058,#41059,#41060,#41061,#41062),.UNSPECIFIED.,.F.,.F.,(4,3,3,
3,3,3,3,4),(45.0986906589432,45.9840830702254,46.9837370500129,47.9833910298004,
48.9830450095879,49.9826989893755,50.982352969163,51.3818759661228),
 .UNSPECIFIED.);
#706=B_SPLINE_CURVE_WITH_KNOTS('',3,(#41067,#41068,#41069,#41070,#41071,
#41072,#41073,#41074,#41075,#41076,#41077,#41078,#41079,#41080,#41081,#41082,
#41083,#41084,#41085,#41086,#41087,#41088),.UNSPECIFIED.,.F.,.F.,(4,3,3,
3,3,3,3,4),(-60.641598184747,-59.9792387872506,-58.979584807463,-57.9799308276755,
-56.980276847888,-55.9806228681005,-54.980968888313,-54.3584128775673),
 .UNSPECIFIED.);
#707=B_SPLINE_CURVE_WITH_KNOTS('',3,(#41089,#41090,#41091,#41092,#41093,
#41094,#41095,#41096,#41097,#41098,#41099,#41100,#41101,#41102,#41103,#41104,
#41105,#41106,#41107,#41108,#41109,#41110),.UNSPECIFIED.,.F.,.F.,(4,3,3,
3,3,3,3,4),(51.3818759661228,51.9820069489505,52.981660928738,53.9813149085255,
54.980968888313,55.9806228681005,56.980276847888,57.6650612733024),
 .UNSPECIFIED.);
#708=B_SPLINE_CURVE_WITH_KNOTS('',3,(#41115,#41116,#41117,#41118,#41119,
#41120,#41121,#41122,#41123,#41124,#41125,#41126,#41127,#41128,#41129,#41130,
#41131,#41132,#41133,#41134,#41135,#41136),.UNSPECIFIED.,.F.,.F.,(4,3,3,
3,3,3,3,4),(-66.9247834919265,-65.9771626659756,-64.9775086861881,-63.9778547064006,
-62.9782007266131,-61.9785467468256,-60.9788927670381,-60.641598184747),
 .UNSPECIFIED.);
#709=B_SPLINE_CURVE_WITH_KNOTS('',3,(#41137,#41138,#41139,#41140,#41141,
#41142,#41143,#41144,#41145,#41146,#41147,#41148,#41149,#41150,#41151,#41152,
#41153,#41154,#41155,#41156,#41157,#41158),.UNSPECIFIED.,.F.,.F.,(4,3,3,
3,3,3,3,4),(57.6650612733024,57.9799308276755,58.9795848074631,59.9792387872506,
60.9788927670381,61.9785467468256,62.9782007266131,63.948246580482),
 .UNSPECIFIED.);
#710=B_SPLINE_CURVE_WITH_KNOTS('',3,(#41163,#41164,#41165,#41166,#41167,
#41168,#41169,#41170,#41171,#41172,#41173,#41174,#41175,#41176,#41177,#41178,
#41179,#41180,#41181,#41182,#41183,#41184,#41185,#41186,#41187),
 .UNSPECIFIED.,.F.,.F.,(4,3,3,3,3,3,3,3,4),(-73.2079687991061,-72.9747405244882,
-71.9750865447007,-70.9754325649132,-69.9757785851257,-68.9761246053381,
-67.9764706255506,-66.9768166457631,-66.9247834919265),.UNSPECIFIED.);
#711=B_SPLINE_CURVE_WITH_KNOTS('',3,(#41188,#41189,#41190,#41191,#41192,
#41193,#41194,#41195,#41196,#41197,#41198,#41199,#41200,#41201,#41202,#41203,
#41204,#41205,#41206,#41207,#41208,#41209,#41210,#41211,#41212),
 .UNSPECIFIED.,.F.,.F.,(4,3,3,3,3,3,3,3,4),(63.948246580482,63.9778547064006,
64.9775086861881,65.9771626659756,66.9768166457631,67.9764706255506,68.9761246053382,
69.9757785851257,70.2314318876616),.UNSPECIFIED.);
#712=B_SPLINE_CURVE_WITH_KNOTS('',3,(#41217,#41218,#41219,#41220,#41221,
#41222,#41223,#41224,#41225,#41226,#41227,#41228,#41229,#41230,#41231,#41232,
#41233,#41234,#41235,#41236,#41237,#41238),.UNSPECIFIED.,.F.,.F.,(4,3,3,
3,3,3,3,4),(-79.4911541062857,-78.9726644032132,-77.9730104234257,-76.9733564436382,
-75.9737024638507,-74.9740484840632,-73.9743945042757,-73.2079687991061),
 .UNSPECIFIED.);
#713=B_SPLINE_CURVE_WITH_KNOTS('',3,(#41239,#41240,#41241,#41242,#41243,
#41244,#41245,#41246,#41247,#41248,#41249,#41250,#41251,#41252,#41253,#41254,
#41255,#41256,#41257,#41258,#41259,#41260),.UNSPECIFIED.,.F.,.F.,(4,3,3,
3,3,3,3,4),(70.2314318876616,70.9754325649132,71.9750865447007,72.9747405244882,
73.9743945042757,74.9740484840632,75.9737024638507,76.5146171948412),
 .UNSPECIFIED.);
#714=B_SPLINE_CURVE_WITH_KNOTS('',3,(#41266,#41267,#41268,#41269,#41270,
#41271,#41272,#41273,#41274),.UNSPECIFIED.,.F.,.F.,(4,1,1,1,1,1,4),(84.8230016469244,
85.5894273520939,86.5890813318814,87.588735311669,88.5883892914565,89.588043271244,
90.5192739353795),.UNSPECIFIED.);
#715=B_SPLINE_CURVE_WITH_KNOTS('',3,(#41277,#41278,#41279,#41280,#41281,
#41282,#41283,#41284,#41285),.UNSPECIFIED.,.F.,.F.,(4,1,1,1,1,1,4),(84.8230016469244,
85.2817408957214,86.2813948755089,87.2810488552964,88.2807028350839,88.7805298249777,
89.2803568148714),.UNSPECIFIED.);
#716=B_SPLINE_CURVE_WITH_KNOTS('',3,(#41290,#41291,#41292,#41293,#41294,
#41295,#41296,#41297,#41298,#41299,#41300),.UNSPECIFIED.,.F.,.F.,(4,1,1,
1,1,1,1,1,4),(78.5398163397448,78.5918494935814,79.5915034733689,80.5911574531564,
81.5908114329439,82.5904654127314,83.5901193925189,84.5897733723064,84.8230016469244),
 .UNSPECIFIED.);
#717=B_SPLINE_CURVE_WITH_KNOTS('',3,(#41301,#41302,#41303,#41304,#41305,
#41306,#41307,#41308,#41309,#41310),.UNSPECIFIED.,.F.,.F.,(4,1,1,1,1,1,
1,4),(78.5398163397448,79.2838170169963,80.2834709967838,81.2831249765713,
82.2827789563588,83.2824329361463,84.2820869159339,84.8230016469244),
 .UNSPECIFIED.);
#718=B_SPLINE_CURVE_WITH_KNOTS('',3,(#41315,#41316,#41317,#41318,#41319,
#41320,#41321,#41322,#41323,#41324),.UNSPECIFIED.,.F.,.F.,(4,1,1,1,1,1,
1,4),(72.2566310325652,72.5939256148563,73.5935795946438,74.5932335744313,
75.5928875542188,76.5925415340064,77.5921955137939,78.5398163397448),
 .UNSPECIFIED.);
#719=B_SPLINE_CURVE_WITH_KNOTS('',3,(#41325,#41326,#41327,#41328,#41329,
#41330,#41331,#41332,#41333,#41334,#41335),.UNSPECIFIED.,.F.,.F.,(4,1,1,
1,1,1,1,1,4),(72.2566310325652,72.2862391584838,73.2858931382713,74.2855471180588,
75.2852010978463,76.2848550776338,77.2845090574213,78.2841630372088,78.5398163397448),
 .UNSPECIFIED.);
#720=B_SPLINE_CURVE_WITH_KNOTS('',3,(#41340,#41341,#41342,#41343,#41344,
#41345,#41346,#41347,#41348,#41349),.UNSPECIFIED.,.F.,.F.,(4,1,1,1,1,1,
1,4),(65.9734457253856,66.5960017361313,67.5956557159188,68.5953096957063,
69.5949636754938,70.5946176552813,71.5942716350688,72.2566310325652),
 .UNSPECIFIED.);
#721=B_SPLINE_CURVE_WITH_KNOTS('',3,(#41350,#41351,#41352,#41353,#41354,
#41355,#41356,#41357,#41358,#41359),.UNSPECIFIED.,.F.,.F.,(4,1,1,1,1,1,
1,4),(65.9734457253856,66.2883152797587,67.2879692595462,68.2876232393337,
69.2872772191212,70.2869311989087,71.2865851786962,72.2566310325652),
 .UNSPECIFIED.);
#722=B_SPLINE_CURVE_WITH_KNOTS('',3,(#41364,#41365,#41366,#41367,#41368,
#41369,#41370,#41371,#41372,#41373),.UNSPECIFIED.,.F.,.F.,(4,1,1,1,1,1,
1,4),(59.690260418206,60.5980778574062,61.5977318371937,62.5973858169812,
63.5970397967687,64.5966937765562,65.5963477563437,65.9734457253856),
 .UNSPECIFIED.);
#723=B_SPLINE_CURVE_WITH_KNOTS('',3,(#41374,#41375,#41376,#41377,#41378,
#41379,#41380,#41381,#41382,#41383),.UNSPECIFIED.,.F.,.F.,(4,1,1,1,1,1,
1,4),(59.690260418206,60.2903914010336,61.2900453808211,62.2896993606087,
63.2893533403962,64.2890073201837,65.2886612999712,65.9734457253856),
 .UNSPECIFIED.);
#724=B_SPLINE_CURVE_WITH_KNOTS('',3,(#41388,#41389,#41390,#41391,#41392,
#41393,#41394,#41395,#41396,#41397,#41398),.UNSPECIFIED.,.F.,.F.,(4,1,1,
1,1,1,1,1,4),(53.4070751110265,53.6004999988936,54.6001539786812,55.5998079584687,
56.5994619382562,57.5991159180437,58.5987698978312,59.5984238776187,59.690260418206),
 .UNSPECIFIED.);
#725=B_SPLINE_CURVE_WITH_KNOTS('',3,(#41399,#41400,#41401,#41402,#41403,
#41404,#41405,#41406,#41407,#41408),.UNSPECIFIED.,.F.,.F.,(4,1,1,1,1,1,
1,4),(53.4070751110264,54.2924675223086,55.2921215020961,56.2917754818836,
57.2914294616711,58.2910834414586,59.2907374212461,59.690260418206),
 .UNSPECIFIED.);
#726=B_SPLINE_CURVE_WITH_KNOTS('',3,(#41413,#41414,#41415,#41416,#41417,
#41418,#41419,#41420,#41421,#41422),.UNSPECIFIED.,.F.,.F.,(4,1,1,1,1,1,
1,4),(47.1238898038469,47.6025761201686,48.6022300999561,49.6018840797436,
50.6015380595311,51.6011920393186,52.6008460191061,53.4070751110265),
 .UNSPECIFIED.);
#727=B_SPLINE_CURVE_WITH_KNOTS('',3,(#41423,#41424,#41425,#41426,#41427,
#41428,#41429,#41430,#41431,#41432,#41433),.UNSPECIFIED.,.F.,.F.,(4,1,1,
1,1,1,1,1,4),(47.1238898038468,47.294889663796,48.2945436435835,49.294197623371,
50.2938516031585,51.2935055829461,52.2931595627336,53.2928135425211,53.4070751110264),
 .UNSPECIFIED.);
#728=B_SPLINE_CURVE_WITH_KNOTS('',3,(#41438,#41439,#41440,#41441,#41442,
#41443,#41444,#41445,#41446,#41447),.UNSPECIFIED.,.F.,.F.,(4,1,1,1,1,1,
1,4),(40.8407044966673,41.6046522414435,42.604306221231,43.6039602010186,
44.6036141808061,45.6032681605936,46.6029221403811,47.1238898038469),
 .UNSPECIFIED.);
#729=B_SPLINE_CURVE_WITH_KNOTS('',3,(#41448,#41449,#41450,#41451,#41452,
#41453,#41454,#41455,#41456,#41457),.UNSPECIFIED.,.F.,.F.,(4,1,1,1,1,1,
1,4),(40.8407044966673,41.296965785071,42.2966197648585,43.296273744646,
44.2959277244335,45.295581704221,46.2952356840085,47.1238898038468),
 .UNSPECIFIED.);
#730=B_SPLINE_CURVE_WITH_KNOTS('',3,(#41462,#41463,#41464,#41465,#41466,
#41467,#41468,#41469,#41470,#41471,#41472),.UNSPECIFIED.,.F.,.F.,(4,1,1,
1,1,1,1,1,4),(34.5575191894877,34.607074382931,35.6067283627185,36.606382342506,
37.6060363222935,38.605690302081,39.6053442818685,40.604998261656,40.8407044966673),
 .UNSPECIFIED.);
#731=B_SPLINE_CURVE_WITH_KNOTS('',3,(#41473,#41474,#41475,#41476,#41477,
#41478,#41479,#41480,#41481,#41482),.UNSPECIFIED.,.F.,.F.,(4,1,1,1,1,1,
1,4),(34.5575191894877,35.2990419063459,36.2986958861334,37.2983498659209,
38.2980038457084,39.2976578254959,40.2973118052834,40.8407044966673),
 .UNSPECIFIED.);
#732=B_SPLINE_CURVE_WITH_KNOTS('',3,(#41487,#41488,#41489,#41490,#41491,
#41492,#41493,#41494,#41495,#41496),.UNSPECIFIED.,.F.,.F.,(4,1,1,1,1,1,
1,4),(28.2743338823081,28.6091505042059,29.6088044839934,30.6084584637809,
31.6081124435684,32.6077664233559,33.6074204031435,34.5575191894877),
 .UNSPECIFIED.);
#733=B_SPLINE_CURVE_WITH_KNOTS('',3,(#41497,#41498,#41499,#41500,#41501,
#41502,#41503,#41504,#41505,#41506,#41507),.UNSPECIFIED.,.F.,.F.,(4,1,1,
1,1,1,1,1,4),(28.2743338823081,28.3014640478333,29.3011180276209,30.3007720074084,
31.3004259871959,32.3000799669834,33.2997339467709,34.2993879265584,34.5575191894877),
 .UNSPECIFIED.);
#734=B_SPLINE_CURVE_WITH_KNOTS('',3,(#41512,#41513,#41514,#41515,#41516,
#41517,#41518,#41519,#41520,#41521),.UNSPECIFIED.,.F.,.F.,(4,1,1,1,1,1,
1,4),(21.9911485751285,22.6112266254809,23.6108806052684,24.6105345850559,
25.6101885648434,26.6098425446309,27.6094965244184,28.2743338823081),
 .UNSPECIFIED.);
#735=B_SPLINE_CURVE_WITH_KNOTS('',3,(#41522,#41523,#41524,#41525,#41526,
#41527,#41528,#41529,#41530,#41531),.UNSPECIFIED.,.F.,.F.,(4,1,1,1,1,1,
1,4),(21.9911485751285,22.3035401691083,23.3031941488958,24.3028481286833,
25.3025021084708,26.3021560882583,27.3018100680458,28.2743338823081),
 .UNSPECIFIED.);
#736=B_SPLINE_CURVE_WITH_KNOTS('',3,(#41536,#41537,#41538,#41539,#41540,
#41541,#41542,#41543,#41544,#41545),.UNSPECIFIED.,.F.,.F.,(4,1,1,1,1,1,
1,4),(15.7079632679489,16.6133027467558,17.6129567265433,18.6126107063308,
19.6122646861183,20.6119186659058,21.6115726456933,21.9911485751285),
 .UNSPECIFIED.);
#737=B_SPLINE_CURVE_WITH_KNOTS('',3,(#41546,#41547,#41548,#41549,#41550,
#41551,#41552,#41553,#41554,#41555),.UNSPECIFIED.,.F.,.F.,(4,1,1,1,1,1,
1,4),(15.7079632679489,16.3056162903832,17.3052702701707,18.3049242499582,
19.3045782297458,20.3042322095333,21.3038861893208,21.9911485751285),
 .UNSPECIFIED.);
#738=B_SPLINE_CURVE_WITH_KNOTS('',3,(#41901,#41902,#41903,#41904,#41905,
#41906,#41907,#41908,#41909,#41910,#41911,#41912,#41913,#41914,#41915,#41916,
#41917,#41918,#41919,#41920,#41921,#41922,#41923,#41924,#41925,#41926,#41927,
#41928,#41929,#41930,#41931,#41932,#41933,#41934,#41935,#41936,#41937,#41938,
#41939,#41940,#41941,#41942,#41943,#41944,#41945,#41946,#41947,#41948,#41949,
#41950,#41951,#41952,#41953,#41954,#41955,#41956,#41957,#41958,#41959,#41960,
#41961,#41962,#41963,#41964,#41965,#41966,#41967,#41968,#41969,#41970,#41971,
#41972,#41973,#41974,#41975,#41976,#41977,#41978,#41979,#41980,#41981,#41982,
#41983,#41984,#41985,#41986,#41987,#41988,#41989,#41990,#41991,#41992,#41993,
#41994,#41995,#41996,#41997,#41998,#41999,#42000,#42001,#42002,#42003,#42004,
#42005,#42006),.UNSPECIFIED.,.F.,.F.,(4,3,3,3,3,3,3,3,3,3,3,3,3,3,3,3,3,
3,3,3,3,3,3,3,3,3,3,3,3,3,3,3,3,3,3,4),(0.,0.0338555796810951,0.0769233841266441,
0.120787014647652,0.164925431151007,0.18768890800956,0.194695307248219,
0.238000863207828,0.281439200502724,0.324499409932901,0.366791407667859,
0.3748100813225,0.380721434265749,0.423140467769373,0.465072972528112,0.506007047124889,
0.514994378647384,0.543782123537011,0.559160795079789,0.5652443143728,0.606242278680173,
0.647897807448946,0.68940569438575,0.717351016075074,0.73199453794532,0.73810671067074,
0.744081074726445,0.745296337764399,0.786338138284623,0.827324070719474,
0.844968273899783,0.854029216944208,0.860905275211015,0.901330989685579,
0.941119121741644,0.968477696161942),.UNSPECIFIED.);
#739=B_SPLINE_CURVE_WITH_KNOTS('',3,(#42007,#42008,#42009,#42010,#42011,
#42012,#42013,#42014,#42015,#42016),.UNSPECIFIED.,.F.,.F.,(4,3,3,4),(76.5146171948412,
76.9733564436382,77.9730104234257,78.9042410875612),.UNSPECIFIED.);
#740=B_SPLINE_CURVE_WITH_KNOTS('',3,(#42018,#42019,#42020,#42021,#42022,
#42023,#42024,#42025,#42026,#42027,#42028,#42029,#42030,#42031,#42032,#42033,
#42034,#42035,#42036,#42037,#42038,#42039,#42040,#42041,#42042,#42043,#42044,
#42045,#42046,#42047,#42048,#42049,#42050,#42051,#42052,#42053,#42054,#42055,
#42056,#42057,#42058,#42059,#42060,#42061,#42062,#42063,#42064,#42065,#42066,
#42067,#42068,#42069,#42070,#42071,#42072,#42073,#42074,#42075,#42076,#42077,
#42078,#42079,#42080,#42081,#42082,#42083,#42084,#42085,#42086,#42087,#42088,
#42089,#42090,#42091,#42092,#42093,#42094,#42095,#42096,#42097,#42098,#42099,
#42100,#42101,#42102,#42103,#42104,#42105,#42106,#42107,#42108,#42109,#42110,
#42111,#42112,#42113,#42114,#42115,#42116,#42117,#42118,#42119,#42120,#42121,
#42122,#42123),.UNSPECIFIED.,.F.,.F.,(4,3,3,3,3,3,3,3,3,3,3,3,3,3,3,3,3,
3,3,3,3,3,3,3,3,3,3,3,3,3,3,3,3,3,3,4),(-0.968477696161962,-0.93834507440756,
-0.898946379179402,-0.87294341376282,-0.858683439823016,-0.849690155368511,
-0.809511368983842,-0.768684814425123,-0.750823196805684,-0.741908901548402,
-0.734140763767536,-0.692650400513915,-0.650694074697968,-0.608745289151999,
-0.577283699992522,-0.564269250932409,-0.556001088558624,-0.513396717295649,
-0.482898932514091,-0.441404470015905,-0.399314127094565,-0.388144431730235,
-0.378349906522554,-0.373280079897934,-0.331122936037102,-0.287943314322124,
-0.244763692607147,-0.214168231031253,-0.200545763543443,-0.193054146419399,
-0.187017976020424,-0.143637415837001,-0.0997905213121978,-0.0560615532128227,
-0.0129908569656951,0.),.UNSPECIFIED.);
#741=B_SPLINE_CURVE_WITH_KNOTS('',3,(#42124,#42125,#42126,#42127,#42128,
#42129,#42130,#42131,#42132),.UNSPECIFIED.,.F.,.F.,(4,1,1,1,1,1,4),(10.3761157273102,
11.3073463914457,12.3070003712332,13.3066543510207,14.3063083308082,15.3059623105957,
15.7079632679489),.UNSPECIFIED.);
#742=B_SPLINE_CURVE_WITH_KNOTS('',3,(#42138,#42139,#42140,#42141,#42142,
#42143,#42144,#42145,#42146,#42147,#42148,#42149,#42150,#42151,#42152,#42153,
#42154,#42155,#42156,#42157,#42158,#42159,#42160,#42161,#42162,#42163,#42164,
#42165,#42166,#42167,#42168,#42169,#42170,#42171,#42172,#42173,#42174,#42175,
#42176,#42177,#42178,#42179,#42180,#42181,#42182,#42183,#42184,#42185,#42186,
#42187,#42188,#42189,#42190,#42191,#42192,#42193,#42194,#42195,#42196,#42197,
#42198,#42199,#42200,#42201,#42202,#42203,#42204,#42205,#42206,#42207,#42208,
#42209,#42210,#42211,#42212,#42213,#42214,#42215,#42216,#42217,#42218,#42219,
#42220,#42221,#42222,#42223,#42224,#42225,#42226,#42227,#42228,#42229,#42230,
#42231,#42232,#42233,#42234,#42235,#42236,#42237,#42238,#42239,#42240,#42241,
#42242,#42243,#42244,#42245,#42246,#42247,#42248,#42249),.UNSPECIFIED.,
 .F.,.F.,(4,3,3,3,3,3,3,3,3,3,3,3,3,3,3,3,3,3,3,3,3,3,3,3,3,3,3,3,3,3,3,
3,3,3,3,3,3,4),(-0.965990216419493,-0.932232205964582,-0.888725512381132,
-0.86148182111266,-0.845752215774746,-0.838628962985686,-0.795398770998977,
-0.752577231134802,-0.732526991421503,-0.722290315506079,-0.715478178658122,
-0.709647482806995,-0.666593990274609,-0.623625418609477,-0.580925676978502,
-0.54890087075527,-0.536423601193463,-0.530582682015647,-0.525159930165745,
-0.483534316458395,-0.452826452085574,-0.410953138863345,-0.368980079811334,
-0.356959708801849,-0.350330796437256,-0.345496631210951,-0.304366782550378,
-0.263166867623492,-0.222981343541229,-0.195108675598575,-0.181421822833585,
-0.173192140728228,-0.16726444049677,-0.125448330372578,-0.0850057436766688,
-0.0449541457505024,-0.00571652159400748,0.),.UNSPECIFIED.);
#743=B_SPLINE_CURVE_WITH_KNOTS('',3,(#42252,#42253,#42254,#42255,#42256,
#42257,#42258,#42259,#42260),.UNSPECIFIED.,.F.,.F.,(4,1,1,1,1,1,4),(11.6150328478183,
12.114859837712,12.6146868276058,13.6143408073933,14.6139947871808,15.6136487669683,
15.7079632679489),.UNSPECIFIED.);
#744=B_SPLINE_CURVE_WITH_KNOTS('',3,(#42606,#42607,#42608,#42609,#42610,
#42611,#42612,#42613,#42614,#42615,#42616,#42617,#42618,#42619,#42620,#42621,
#42622,#42623,#42624,#42625,#42626,#42627,#42628,#42629,#42630,#42631,#42632,
#42633,#42634,#42635,#42636,#42637,#42638,#42639,#42640,#42641,#42642,#42643,
#42644,#42645,#42646,#42647,#42648,#42649,#42650,#42651,#42652,#42653,#42654,
#42655,#42656,#42657,#42658,#42659,#42660,#42661,#42662,#42663,#42664,#42665,
#42666,#42667,#42668,#42669,#42670,#42671,#42672,#42673,#42674,#42675,#42676,
#42677,#42678,#42679,#42680,#42681,#42682,#42683,#42684,#42685,#42686,#42687,
#42688,#42689,#42690,#42691,#42692,#42693,#42694,#42695,#42696,#42697,#42698,
#42699,#42700,#42701,#42702,#42703,#42704,#42705,#42706,#42707,#42708,#42709,
#42710,#42711,#42712,#42713,#42714),.UNSPECIFIED.,.F.,.F.,(4,3,3,3,3,3,
3,3,3,3,3,3,3,3,3,3,3,3,3,3,3,3,3,3,3,3,3,3,3,3,3,3,3,3,3,3,4),(0.,0.0300808882250601,
0.0690837691274257,0.108977971558979,0.149535303300715,0.161775980247188,
0.169677926634296,0.176345077737452,0.217218238973177,0.258694872125898,
0.300344044967144,0.341653389143491,0.347771209594167,0.352609284959025,
0.39494049143562,0.437189104774325,0.478722267806855,0.48483985412653,0.51451003945568,
0.524490292215405,0.530274299792254,0.571233373520478,0.613481573281312,
0.656140144392953,0.689170740576341,0.705686038668035,0.714536893087061,
0.720494023679387,0.722201336759729,0.765231119221639,0.808568534613332,
0.828246244839095,0.838610463895481,0.846178719169224,0.890004704789425,
0.933557298850571,0.965990216419437),.UNSPECIFIED.);
#745=B_SPLINE_CURVE_WITH_KNOTS('',3,(#42715,#42716,#42717,#42718,#42719,
#42720,#42721,#42722,#42723,#42724),.UNSPECIFIED.,.F.,.F.,(4,3,3,4),(-80.9719723627883,
-80.4721453728945,-79.9723183830007,-79.4911541062857),.UNSPECIFIED.);
#746=B_SPLINE_CURVE_WITH_KNOTS('',2,(#42737,#42738,#42739),
 .UNSPECIFIED.,.F.,.F.,(3,3),(0.,1.),.UNSPECIFIED.);
#747=B_SPLINE_CURVE_WITH_KNOTS('',2,(#42743,#42744,#42745),
 .UNSPECIFIED.,.F.,.F.,(3,3),(0.,1.),.UNSPECIFIED.);
#748=B_SPLINE_CURVE_WITH_KNOTS('',2,(#42754,#42755,#42756),
 .UNSPECIFIED.,.F.,.F.,(3,3),(0.,1.),.UNSPECIFIED.);
#749=B_SPLINE_CURVE_WITH_KNOTS('',2,(#42759,#42760,#42761),
 .UNSPECIFIED.,.F.,.F.,(3,3),(0.,1.),.UNSPECIFIED.);
#750=B_SPLINE_CURVE_WITH_KNOTS('',2,(#42769,#42770,#42771),
 .UNSPECIFIED.,.F.,.F.,(3,3),(0.,1.),.UNSPECIFIED.);
#751=B_SPLINE_CURVE_WITH_KNOTS('',2,(#42774,#42775,#42776),
 .UNSPECIFIED.,.F.,.F.,(3,3),(0.,1.),.UNSPECIFIED.);
#752=B_SPLINE_CURVE_WITH_KNOTS('',2,(#42784,#42785,#42786),
 .UNSPECIFIED.,.F.,.F.,(3,3),(0.,1.),.UNSPECIFIED.);
#753=B_SPLINE_CURVE_WITH_KNOTS('',2,(#42789,#42790,#42791),
 .UNSPECIFIED.,.F.,.F.,(3,3),(0.,1.),.UNSPECIFIED.);
#754=B_SPLINE_CURVE_WITH_KNOTS('',2,(#42799,#42800,#42801),
 .UNSPECIFIED.,.F.,.F.,(3,3),(0.,1.),.UNSPECIFIED.);
#755=B_SPLINE_CURVE_WITH_KNOTS('',2,(#42804,#42805,#42806),
 .UNSPECIFIED.,.F.,.F.,(3,3),(0.,1.),.UNSPECIFIED.);
#756=B_SPLINE_CURVE_WITH_KNOTS('',2,(#42814,#42815,#42816),
 .UNSPECIFIED.,.F.,.F.,(3,3),(0.,1.),.UNSPECIFIED.);
#757=B_SPLINE_CURVE_WITH_KNOTS('',2,(#42819,#42820,#42821),
 .UNSPECIFIED.,.F.,.F.,(3,3),(0.,1.),.UNSPECIFIED.);
#758=B_SPLINE_CURVE_WITH_KNOTS('',2,(#42829,#42830,#42831),
 .UNSPECIFIED.,.F.,.F.,(3,3),(0.,1.),.UNSPECIFIED.);
#759=B_SPLINE_CURVE_WITH_KNOTS('',2,(#42834,#42835,#42836),
 .UNSPECIFIED.,.F.,.F.,(3,3),(0.,1.),.UNSPECIFIED.);
#760=B_SPLINE_CURVE_WITH_KNOTS('',2,(#42844,#42845,#42846),
 .UNSPECIFIED.,.F.,.F.,(3,3),(0.,1.),.UNSPECIFIED.);
#761=B_SPLINE_CURVE_WITH_KNOTS('',2,(#42849,#42850,#42851),
 .UNSPECIFIED.,.F.,.F.,(3,3),(0.,1.),.UNSPECIFIED.);
#762=B_SPLINE_CURVE_WITH_KNOTS('',2,(#42859,#42860,#42861),
 .UNSPECIFIED.,.F.,.F.,(3,3),(0.,1.),.UNSPECIFIED.);
#763=B_SPLINE_CURVE_WITH_KNOTS('',2,(#42864,#42865,#42866),
 .UNSPECIFIED.,.F.,.F.,(3,3),(0.,1.),.UNSPECIFIED.);
#764=B_SPLINE_CURVE_WITH_KNOTS('',2,(#42874,#42875,#42876),
 .UNSPECIFIED.,.F.,.F.,(3,3),(0.,1.),.UNSPECIFIED.);
#765=B_SPLINE_CURVE_WITH_KNOTS('',2,(#42879,#42880,#42881),
 .UNSPECIFIED.,.F.,.F.,(3,3),(0.,1.),.UNSPECIFIED.);
#766=B_SPLINE_CURVE_WITH_KNOTS('',2,(#42888,#42889,#42890),
 .UNSPECIFIED.,.F.,.F.,(3,3),(0.,1.),.UNSPECIFIED.);
#767=B_SPLINE_CURVE_WITH_KNOTS('',2,(#42891,#42892,#42893),
 .UNSPECIFIED.,.F.,.F.,(3,3),(0.,1.),.UNSPECIFIED.);
#768=B_SPLINE_CURVE_WITH_KNOTS('',2,(#42964,#42965,#42966),
 .UNSPECIFIED.,.F.,.F.,(3,3),(0.,1.),.UNSPECIFIED.);
#769=B_SPLINE_CURVE_WITH_KNOTS('',2,(#42970,#42971,#42972),
 .UNSPECIFIED.,.F.,.F.,(3,3),(0.,1.),.UNSPECIFIED.);
#770=B_SPLINE_CURVE_WITH_KNOTS('',2,(#42981,#42982,#42983),
 .UNSPECIFIED.,.F.,.F.,(3,3),(0.,1.),.UNSPECIFIED.);
#771=B_SPLINE_CURVE_WITH_KNOTS('',2,(#42986,#42987,#42988),
 .UNSPECIFIED.,.F.,.F.,(3,3),(0.,1.),.UNSPECIFIED.);
#772=B_SPLINE_CURVE_WITH_KNOTS('',2,(#42996,#42997,#42998),
 .UNSPECIFIED.,.F.,.F.,(3,3),(0.,1.),.UNSPECIFIED.);
#773=B_SPLINE_CURVE_WITH_KNOTS('',2,(#43001,#43002,#43003),
 .UNSPECIFIED.,.F.,.F.,(3,3),(0.,1.),.UNSPECIFIED.);
#774=B_SPLINE_CURVE_WITH_KNOTS('',2,(#43011,#43012,#43013),
 .UNSPECIFIED.,.F.,.F.,(3,3),(0.,1.),.UNSPECIFIED.);
#775=B_SPLINE_CURVE_WITH_KNOTS('',2,(#43016,#43017,#43018),
 .UNSPECIFIED.,.F.,.F.,(3,3),(0.,1.),.UNSPECIFIED.);
#776=B_SPLINE_CURVE_WITH_KNOTS('',2,(#43026,#43027,#43028),
 .UNSPECIFIED.,.F.,.F.,(3,3),(0.,1.),.UNSPECIFIED.);
#777=B_SPLINE_CURVE_WITH_KNOTS('',2,(#43031,#43032,#43033),
 .UNSPECIFIED.,.F.,.F.,(3,3),(0.,1.),.UNSPECIFIED.);
#778=B_SPLINE_CURVE_WITH_KNOTS('',2,(#43041,#43042,#43043),
 .UNSPECIFIED.,.F.,.F.,(3,3),(0.,1.),.UNSPECIFIED.);
#779=B_SPLINE_CURVE_WITH_KNOTS('',2,(#43046,#43047,#43048),
 .UNSPECIFIED.,.F.,.F.,(3,3),(0.,1.),.UNSPECIFIED.);
#780=B_SPLINE_CURVE_WITH_KNOTS('',2,(#43056,#43057,#43058),
 .UNSPECIFIED.,.F.,.F.,(3,3),(0.,1.),.UNSPECIFIED.);
#781=B_SPLINE_CURVE_WITH_KNOTS('',2,(#43061,#43062,#43063),
 .UNSPECIFIED.,.F.,.F.,(3,3),(0.,1.),.UNSPECIFIED.);
#782=B_SPLINE_CURVE_WITH_KNOTS('',2,(#43071,#43072,#43073),
 .UNSPECIFIED.,.F.,.F.,(3,3),(0.,1.),.UNSPECIFIED.);
#783=B_SPLINE_CURVE_WITH_KNOTS('',2,(#43076,#43077,#43078),
 .UNSPECIFIED.,.F.,.F.,(3,3),(0.,1.),.UNSPECIFIED.);
#784=B_SPLINE_CURVE_WITH_KNOTS('',2,(#43086,#43087,#43088),
 .UNSPECIFIED.,.F.,.F.,(3,3),(0.,1.),.UNSPECIFIED.);
#785=B_SPLINE_CURVE_WITH_KNOTS('',2,(#43091,#43092,#43093),
 .UNSPECIFIED.,.F.,.F.,(3,3),(0.,1.),.UNSPECIFIED.);
#786=B_SPLINE_CURVE_WITH_KNOTS('',2,(#43101,#43102,#43103),
 .UNSPECIFIED.,.F.,.F.,(3,3),(0.,1.),.UNSPECIFIED.);
#787=B_SPLINE_CURVE_WITH_KNOTS('',2,(#43106,#43107,#43108),
 .UNSPECIFIED.,.F.,.F.,(3,3),(0.,1.),.UNSPECIFIED.);
#788=B_SPLINE_CURVE_WITH_KNOTS('',2,(#43115,#43116,#43117),
 .UNSPECIFIED.,.F.,.F.,(3,3),(0.,1.),.UNSPECIFIED.);
#789=B_SPLINE_CURVE_WITH_KNOTS('',2,(#43118,#43119,#43120),
 .UNSPECIFIED.,.F.,.F.,(3,3),(0.,1.),.UNSPECIFIED.);
#790=B_SPLINE_CURVE_WITH_KNOTS('',3,(#44019,#44020,#44021,#44022,#44023,
#44024,#44025,#44026,#44027,#44028,#44029,#44030,#44031,#44032,#44033,#44034,
#44035,#44036,#44037,#44038,#44039,#44040,#44041,#44042,#44043,#44044,#44045,
#44046,#44047,#44048,#44049,#44050,#44051,#44052,#44053,#44054,#44055,#44056,
#44057,#44058,#44059,#44060,#44061,#44062,#44063,#44064,#44065,#44066,#44067,
#44068,#44069,#44070,#44071,#44072,#44073),.UNSPECIFIED.,.F.,.F.,(4,3,3,
3,3,3,3,3,3,3,3,3,3,3,3,3,3,3,4),(0.,0.0457286896420428,0.093735766404543,
0.144908104483403,0.201496379478659,0.273083254680907,0.346956864852629,
0.403665327235726,0.454892838429364,0.50491934325277,0.554438098871657,
0.607768246203659,0.669007112544933,0.7517553344087,0.813816500806525,0.866510270075527,
0.916070793074055,0.962308549660881,1.),.UNSPECIFIED.);
#791=B_SPLINE_CURVE_WITH_KNOTS('',3,(#44075,#44076,#44077,#44078),
 .UNSPECIFIED.,.F.,.F.,(4,4),(0.,1.),.UNSPECIFIED.);
#792=B_SPLINE_CURVE_WITH_KNOTS('',3,(#44080,#44081,#44082,#44083,#44084,
#44085,#44086,#44087,#44088,#44089,#44090,#44091,#44092,#44093,#44094,#44095,
#44096,#44097,#44098,#44099,#44100,#44101,#44102,#44103,#44104,#44105,#44106,
#44107,#44108,#44109,#44110,#44111,#44112,#44113,#44114,#44115,#44116,#44117,
#44118,#44119,#44120,#44121,#44122,#44123,#44124,#44125,#44126,#44127,#44128,
#44129,#44130,#44131,#44132,#44133,#44134),.UNSPECIFIED.,.F.,.F.,(4,3,3,
3,3,3,3,3,3,3,3,3,3,3,3,3,3,3,4),(0.,0.0457354346940703,0.0937501435458722,
0.144931624161072,0.20153359300957,0.273162634682721,0.347001992162202,
0.403710204556331,0.454939815804421,0.505015264674136,0.55453467353116,
0.607869111005662,0.669124504105853,0.75184337807939,0.813882533559542,
0.866563287605176,0.916113481178306,0.962343356347582,1.),.UNSPECIFIED.);
#793=B_SPLINE_CURVE_WITH_KNOTS('',3,(#44161,#44162,#44163,#44164,#44165,
#44166),.UNSPECIFIED.,.F.,.F.,(4,1,1,4),(-1.83137755752329,-1.04650146144188,
-0.52325073072094,-1.12036785251785E-15),.UNSPECIFIED.);
#794=B_SPLINE_CURVE_WITH_KNOTS('',3,(#44169,#44170,#44171,#44172,#44173,
#44174),.UNSPECIFIED.,.F.,.F.,(4,1,1,4),(1.12036785251785E-15,0.52325073072094,
1.04650146144188,1.83137755752329),.UNSPECIFIED.);
#795=B_SPLINE_CURVE_WITH_KNOTS('',3,(#44202,#44203,#44204,#44205,#44206,
#44207,#44208),.UNSPECIFIED.,.F.,.F.,(4,1,1,1,4),(-1.84798528578773,-1.0559915918787,
-0.527995795939349,-0.263997897969673,2.22044604925035E-15),
 .UNSPECIFIED.);
#796=B_SPLINE_CURVE_WITH_KNOTS('',3,(#44209,#44210,#44211,#44212,#44213,
#44214,#44215,#44216,#44217,#44218,#44219,#44220,#44221,#44222,#44223,#44224,
#44225,#44226,#44227,#44228,#44229,#44230,#44231,#44232,#44233,#44234,#44235,
#44236,#44237,#44238,#44239,#44240,#44241,#44242,#44243,#44244,#44245,#44246,
#44247,#44248,#44249,#44250,#44251,#44252,#44253,#44254,#44255,#44256,#44257,
#44258,#44259,#44260,#44261,#44262,#44263),.UNSPECIFIED.,.F.,.F.,(4,3,3,
3,3,3,3,3,3,3,3,3,3,3,3,3,3,3,4),(0.,0.0457132863749496,0.0937034140726246,
0.144856244328766,0.201417245857591,0.272937663581204,0.346860860114579,
0.403562222955401,0.454780120675855,0.503694405033869,0.553118113908822,
0.606292311523956,0.667190059273958,0.750392544455468,0.812794408341601,
0.865541001719504,0.91513380035021,0.961377819679936,1.),.UNSPECIFIED.);
#797=B_SPLINE_CURVE_WITH_KNOTS('',3,(#44305,#44306,#44307,#44308,#44309,
#44310,#44311,#44312,#44313,#44314,#44315,#44316,#44317,#44318,#44319,#44320,
#44321,#44322,#44323,#44324,#44325,#44326,#44327,#44328,#44329,#44330,#44331,
#44332,#44333,#44334,#44335,#44336,#44337,#44338,#44339,#44340,#44341,#44342,
#44343,#44344,#44345,#44346,#44347,#44348,#44349,#44350,#44351,#44352,#44353,
#44354,#44355,#44356,#44357,#44358,#44359),.UNSPECIFIED.,.F.,.F.,(4,3,3,
3,3,3,3,3,3,3,3,3,3,3,3,3,3,3,4),(0.,0.0457286896420497,0.0937357664051448,
0.144908104483507,0.201496379477572,0.273083254679073,0.34695686485381,
0.403665327236825,0.454892838430446,0.504919343256333,0.554438098874351,
0.607768246204756,0.669007112545538,0.751755334409154,0.813816500806865,
0.866510270075756,0.916070793073951,0.962308549660669,1.),.UNSPECIFIED.);
#798=B_SPLINE_CURVE_WITH_KNOTS('',3,(#44361,#44362,#44363,#44364),
 .UNSPECIFIED.,.F.,.F.,(4,4),(0.,1.),.UNSPECIFIED.);
#799=B_SPLINE_CURVE_WITH_KNOTS('',3,(#44366,#44367,#44368,#44369,#44370,
#44371,#44372,#44373,#44374,#44375,#44376,#44377,#44378,#44379,#44380,#44381,
#44382,#44383,#44384,#44385,#44386,#44387,#44388,#44389,#44390,#44391,#44392,
#44393,#44394,#44395,#44396,#44397,#44398,#44399,#44400,#44401,#44402,#44403,
#44404,#44405,#44406,#44407,#44408,#44409,#44410,#44411,#44412,#44413,#44414,
#44415,#44416,#44417,#44418,#44419,#44420),.UNSPECIFIED.,.F.,.F.,(4,3,3,
3,3,3,3,3,3,3,3,3,3,3,3,3,3,3,4),(0.,0.0457354346944535,0.0937501435463771,
0.144931624161605,0.201533593009091,0.273162634682324,0.347001992161254,
0.40371020455566,0.454939815803727,0.505015264672052,0.554534673528658,
0.607869111002009,0.669124504101831,0.751843378076374,0.81388253355728,
0.866563287602945,0.916113481176235,0.962343356345523,1.),.UNSPECIFIED.);
#800=B_SPLINE_CURVE_WITH_KNOTS('',3,(#44446,#44447,#44448,#44449,#44450,
#44451),.UNSPECIFIED.,.F.,.F.,(4,1,1,4),(-1.83137755752328,-1.04650146144188,
-0.523250730720938,-1.19348975147204E-15),.UNSPECIFIED.);
#801=B_SPLINE_CURVE_WITH_KNOTS('',3,(#44452,#44453,#44454,#44455,#44456,
#44457),.UNSPECIFIED.,.F.,.F.,(4,1,1,4),(1.19348975147204E-15,0.523250730720938,
1.04650146144188,1.83137755752328),.UNSPECIFIED.);
#802=B_SPLINE_CURVE_WITH_KNOTS('',3,(#44508,#44509,#44510,#44511),
 .UNSPECIFIED.,.F.,.F.,(4,4),(0.,1.),.UNSPECIFIED.);
#803=B_SPLINE_CURVE_WITH_KNOTS('',3,(#44512,#44513,#44514,#44515,#44516,
#44517,#44518,#44519,#44520,#44521,#44522,#44523,#44524,#44525,#44526,#44527,
#44528,#44529,#44530,#44531,#44532,#44533,#44534,#44535,#44536,#44537,#44538,
#44539,#44540,#44541,#44542,#44543,#44544,#44545,#44546,#44547,#44548,#44549,
#44550,#44551,#44552,#44553,#44554,#44555,#44556,#44557,#44558,#44559,#44560,
#44561,#44562,#44563,#44564,#44565,#44566),.UNSPECIFIED.,.F.,.F.,(4,3,3,
3,3,3,3,3,3,3,3,3,3,3,3,3,3,3,4),(0.,0.0457192684189794,0.0937161650457905,
0.144877103812885,0.201450247057813,0.273008005410247,0.346900713129524,
0.403601873101028,0.454821643624999,0.503755854254589,0.553178607570083,
0.606353906221449,0.667259789018953,0.750444841764215,0.812833631323161,
0.865569987859207,0.915154528460697,0.961391964978838,1.),.UNSPECIFIED.);
#804=B_SPLINE_CURVE_WITH_KNOTS('',3,(#44601,#44602,#44603,#44604,#44605,
#44606,#44607,#44608,#44609,#44610,#44611,#44612,#44613,#44614,#44615,#44616,
#44617,#44618,#44619,#44620,#44621,#44622,#44623,#44624,#44625,#44626,#44627,
#44628,#44629,#44630,#44631,#44632,#44633,#44634,#44635,#44636,#44637,#44638,
#44639,#44640,#44641,#44642,#44643,#44644,#44645,#44646,#44647,#44648,#44649,
#44650,#44651,#44652,#44653,#44654,#44655),.UNSPECIFIED.,.F.,.F.,(4,3,3,
3,3,3,3,3,3,3,3,3,3,3,3,3,3,3,4),(0.,0.0457132863751776,0.093703414073713,
0.144856244329965,0.201417245862007,0.272937663588709,0.346860860113243,
0.403562222954799,0.454780120675612,0.503694405126385,0.553118114005435,
0.60629231162977,0.667190059400792,0.750392544550594,0.812794408412946,
0.865541001786358,0.915133800413365,0.961377819741294,1.),.UNSPECIFIED.);
#805=B_SPLINE_CURVE_WITH_KNOTS('',3,(#44657,#44658,#44659,#44660),
 .UNSPECIFIED.,.F.,.F.,(4,4),(0.,1.),.UNSPECIFIED.);
#806=B_SPLINE_CURVE_WITH_KNOTS('',3,(#44662,#44663,#44664,#44665,#44666,
#44667,#44668,#44669,#44670,#44671,#44672,#44673,#44674,#44675,#44676,#44677,
#44678,#44679,#44680,#44681,#44682,#44683,#44684,#44685,#44686,#44687,#44688,
#44689,#44690,#44691,#44692,#44693,#44694,#44695,#44696,#44697,#44698,#44699,
#44700,#44701,#44702,#44703,#44704,#44705,#44706,#44707,#44708,#44709,#44710,
#44711,#44712,#44713,#44714,#44715,#44716),.UNSPECIFIED.,.F.,.F.,(4,3,3,
3,3,3,3,3,3,3,3,3,3,3,3,3,3,3,4),(0.,0.04571926841842,0.093716165045645,
0.144877103812341,0.201450247056974,0.273008005409813,0.346900713129314,
0.403601873101765,0.454821643626316,0.503755854294485,0.553178607611452,
0.606353906267959,0.667259789075755,0.750444841806816,0.812833631355112,
0.865569987889283,0.915154528488622,0.961391965006156,1.),.UNSPECIFIED.);
#807=B_SPLINE_CURVE_WITH_KNOTS('',3,(#44746,#44747,#44748,#44749,#44750,
#44751,#44752),.UNSPECIFIED.,.F.,.F.,(4,1,1,1,4),(-1.84798528578773,-1.0559915918787,
-0.527995795939349,-0.263997897969672,4.44089209850066E-15),
 .UNSPECIFIED.);
#808=B_SPLINE_CURVE_WITH_KNOTS('',3,(#44754,#44755,#44756,#44757,#44758,
#44759,#44760),.UNSPECIFIED.,.F.,.F.,(4,1,1,1,4),(-4.44089209850066E-15,
0.263997897969672,0.527995795939349,1.0559915918787,1.84798528578773),
 .UNSPECIFIED.);
#809=B_SPLINE_CURVE_WITH_KNOTS('',3,(#44791,#44792,#44793,#44794,#44795,
#44796,#44797),.UNSPECIFIED.,.F.,.F.,(4,1,1,1,4),(-2.22044604925035E-15,
0.263997897969673,0.527995795939349,1.0559915918787,1.84798528578773),
 .UNSPECIFIED.);
#810=B_SPLINE_CURVE_WITH_KNOTS('',3,(#45054,#45055,#45056,#45057),
 .UNSPECIFIED.,.F.,.F.,(4,4),(-0.0573534079505418,0.),.UNSPECIFIED.);
#811=B_SPLINE_CURVE_WITH_KNOTS('',3,(#45060,#45061,#45062,#45063),
 .UNSPECIFIED.,.F.,.F.,(4,4),(-0.0573534079505118,0.),.UNSPECIFIED.);
#812=B_SPLINE_CURVE_WITH_KNOTS('',3,(#45094,#45095,#45096,#45097),
 .UNSPECIFIED.,.F.,.F.,(4,4),(-0.0573537350950076,0.),.UNSPECIFIED.);
#813=B_SPLINE_CURVE_WITH_KNOTS('',3,(#45100,#45101,#45102,#45103),
 .UNSPECIFIED.,.F.,.F.,(4,4),(-0.0573534079504966,0.),.UNSPECIFIED.);
#814=B_SPLINE_SURFACE_WITH_KNOTS('',3,3,((#22206,#22207,#22208,#22209,#22210,
#22211),(#22212,#22213,#22214,#22215,#22216,#22217),(#22218,#22219,#22220,
#22221,#22222,#22223),(#22224,#22225,#22226,#22227,#22228,#22229)),
 .UNSPECIFIED.,.F.,.F.,.F.,(4,4),(4,1,1,4),(0.,1.),(0.,0.571428571428571,
0.857142857142857,1.),.UNSPECIFIED.);
#815=B_SPLINE_SURFACE_WITH_KNOTS('',3,3,((#22349,#22350,#22351,#22352,#22353),
(#22354,#22355,#22356,#22357,#22358),(#22359,#22360,#22361,#22362,#22363),
(#22364,#22365,#22366,#22367,#22368)),.UNSPECIFIED.,.F.,.F.,.F.,(4,4),(4,
1,4),(0.,1.),(-1.66265780683826,-0.950090175336147,8.76618254786689E-34),
 .UNSPECIFIED.);
#816=B_SPLINE_SURFACE_WITH_KNOTS('',3,3,((#22426,#22427,#22428,#22429,#22430,
#22431),(#22432,#22433,#22434,#22435,#22436,#22437),(#22438,#22439,#22440,
#22441,#22442,#22443),(#22444,#22445,#22446,#22447,#22448,#22449)),
 .UNSPECIFIED.,.F.,.F.,.F.,(4,4),(4,1,1,4),(0.,1.),(0.,0.571428571428571,
0.857142857142857,1.),.UNSPECIFIED.);
#817=B_SPLINE_SURFACE_WITH_KNOTS('',3,3,((#22569,#22570,#22571,#22572,#22573,
#22574),(#22575,#22576,#22577,#22578,#22579,#22580),(#22581,#22582,#22583,
#22584,#22585,#22586),(#22587,#22588,#22589,#22590,#22591,#22592)),
 .UNSPECIFIED.,.F.,.F.,.F.,(4,4),(4,1,1,4),(0.,1.),(0.,0.571428571428571,
0.857142857142857,1.),.UNSPECIFIED.);
#818=B_SPLINE_SURFACE_WITH_KNOTS('',3,3,((#22712,#22713,#22714,#22715),
(#22716,#22717,#22718,#22719),(#22720,#22721,#22722,#22723),(#22724,#22725,
#22726,#22727)),.UNSPECIFIED.,.F.,.F.,.F.,(4,4),(4,4),(0.,1.),(1.38548660592135,
2.14032342811115),.UNSPECIFIED.);
#819=B_SPLINE_SURFACE_WITH_KNOTS('',3,3,((#22739,#22740,#22741,#22742),
(#22743,#22744,#22745,#22746),(#22747,#22748,#22749,#22750),(#22751,#22752,
#22753,#22754)),.UNSPECIFIED.,.F.,.F.,.F.,(4,4),(4,4),(0.,1.),(-1.33701776267244,
-0.785398163397445),.UNSPECIFIED.);
#820=B_SPLINE_SURFACE_WITH_KNOTS('',3,3,((#22769,#22770,#22771,#22772),
(#22773,#22774,#22775,#22776),(#22777,#22778,#22779,#22780),(#22781,#22782,
#22783,#22784)),.UNSPECIFIED.,.F.,.F.,.F.,(4,4),(4,4),(0.,1.),(2.14032342811107,
2.35619449019235),.UNSPECIFIED.);
#821=B_SPLINE_SURFACE_WITH_KNOTS('',3,3,((#22802,#22803,#22804,#22805),
(#22806,#22807,#22808,#22809),(#22810,#22811,#22812,#22813),(#22814,#22815,
#22816,#22817)),.UNSPECIFIED.,.F.,.F.,.F.,(4,4),(4,4),(0.,1.),(1.33701776267243,
1.5707963267949),.UNSPECIFIED.);
#822=B_SPLINE_SURFACE_WITH_KNOTS('',3,3,((#22826,#22827,#22828,#22829),
(#22830,#22831,#22832,#22833),(#22834,#22835,#22836,#22837),(#22838,#22839,
#22840,#22841)),.UNSPECIFIED.,.F.,.F.,.F.,(4,4),(4,4),(0.,1.),(0.785398163397449,
1.33701776267244),.UNSPECIFIED.);
#823=B_SPLINE_SURFACE_WITH_KNOTS('',3,3,((#22856,#22857,#22858,#22859),
(#22860,#22861,#22862,#22863),(#22864,#22865,#22866,#22867),(#22868,#22869,
#22870,#22871)),.UNSPECIFIED.,.F.,.F.,.F.,(4,4),(4,4),(0.,1.),(-1.5707963267949,
-1.33701776267244),.UNSPECIFIED.);
#824=B_SPLINE_SURFACE_WITH_KNOTS('',3,3,((#22880,#22881,#22882,#22883),
(#22884,#22885,#22886,#22887),(#22888,#22889,#22890,#22891),(#22892,#22893,
#22894,#22895)),.UNSPECIFIED.,.F.,.F.,.F.,(4,4),(4,4),(0.,1.),(-2.14032342811115,
-1.38548660592135),.UNSPECIFIED.);
#825=B_SPLINE_SURFACE_WITH_KNOTS('',3,3,((#22907,#22908,#22909,#22910),
(#22911,#22912,#22913,#22914),(#22915,#22916,#22917,#22918),(#22919,#22920,
#22921,#22922)),.UNSPECIFIED.,.F.,.F.,.F.,(4,4),(4,4),(0.,1.),(-2.35619449019234,
-2.14032342811108),.UNSPECIFIED.);
#826=B_SPLINE_SURFACE_WITH_KNOTS('',2,1,((#23522,#23523),(#23524,#23525),
(#23526,#23527)),.UNSPECIFIED.,.F.,.F.,.F.,(3,3),(2,2),(0.,1.),(0.,0.0300000000000002),
 .UNSPECIFIED.);
#827=B_SPLINE_SURFACE_WITH_KNOTS('',2,1,((#23535,#23536),(#23537,#23538),
(#23539,#23540)),.UNSPECIFIED.,.F.,.F.,.F.,(3,3),(2,2),(0.,1.),(0.,0.0300000000000002),
 .UNSPECIFIED.);
#828=B_SPLINE_SURFACE_WITH_KNOTS('',2,1,((#23546,#23547),(#23548,#23549),
(#23550,#23551)),.UNSPECIFIED.,.F.,.F.,.F.,(3,3),(2,2),(0.,1.),(0.,0.0300000000000002),
 .UNSPECIFIED.);
#829=B_SPLINE_SURFACE_WITH_KNOTS('',2,1,((#23557,#23558),(#23559,#23560),
(#23561,#23562)),.UNSPECIFIED.,.F.,.F.,.F.,(3,3),(2,2),(0.,1.),(0.,0.0300000000000002),
 .UNSPECIFIED.);
#830=B_SPLINE_SURFACE_WITH_KNOTS('',2,1,((#23568,#23569),(#23570,#23571),
(#23572,#23573)),.UNSPECIFIED.,.F.,.F.,.F.,(3,3),(2,2),(0.,1.),(0.,0.0300000000000002),
 .UNSPECIFIED.);
#831=B_SPLINE_SURFACE_WITH_KNOTS('',2,1,((#23579,#23580),(#23581,#23582),
(#23583,#23584)),.UNSPECIFIED.,.F.,.F.,.F.,(3,3),(2,2),(0.,1.),(0.,0.0300000000000002),
 .UNSPECIFIED.);
#832=B_SPLINE_SURFACE_WITH_KNOTS('',2,1,((#23590,#23591),(#23592,#23593),
(#23594,#23595)),.UNSPECIFIED.,.F.,.F.,.F.,(3,3),(2,2),(0.,1.),(0.,0.0300000000000002),
 .UNSPECIFIED.);
#833=B_SPLINE_SURFACE_WITH_KNOTS('',2,1,((#23601,#23602),(#23603,#23604),
(#23605,#23606)),.UNSPECIFIED.,.F.,.F.,.F.,(3,3),(2,2),(0.,1.),(0.,0.0300000000000002),
 .UNSPECIFIED.);
#834=B_SPLINE_SURFACE_WITH_KNOTS('',2,1,((#23612,#23613),(#23614,#23615),
(#23616,#23617)),.UNSPECIFIED.,.F.,.F.,.F.,(3,3),(2,2),(0.,1.),(0.,0.0300000000000002),
 .UNSPECIFIED.);
#835=B_SPLINE_SURFACE_WITH_KNOTS('',2,1,((#23623,#23624),(#23625,#23626),
(#23627,#23628)),.UNSPECIFIED.,.F.,.F.,.F.,(3,3),(2,2),(0.,1.),(0.,0.0300000000000002),
 .UNSPECIFIED.);
#836=B_SPLINE_SURFACE_WITH_KNOTS('',2,1,((#23634,#23635),(#23636,#23637),
(#23638,#23639)),.UNSPECIFIED.,.F.,.F.,.F.,(3,3),(2,2),(0.,1.),(0.,0.0300000000000002),
 .UNSPECIFIED.);
#837=B_SPLINE_SURFACE_WITH_KNOTS('',2,1,((#23677,#23678),(#23679,#23680),
(#23681,#23682)),.UNSPECIFIED.,.F.,.F.,.F.,(3,3),(2,2),(0.,1.),(0.,0.0300000000000002),
 .UNSPECIFIED.);
#838=B_SPLINE_SURFACE_WITH_KNOTS('',2,1,((#23690,#23691),(#23692,#23693),
(#23694,#23695)),.UNSPECIFIED.,.F.,.F.,.F.,(3,3),(2,2),(0.,1.),(0.,0.0300000000000002),
 .UNSPECIFIED.);
#839=B_SPLINE_SURFACE_WITH_KNOTS('',2,1,((#23701,#23702),(#23703,#23704),
(#23705,#23706)),.UNSPECIFIED.,.F.,.F.,.F.,(3,3),(2,2),(0.,1.),(0.,0.0300000000000002),
 .UNSPECIFIED.);
#840=B_SPLINE_SURFACE_WITH_KNOTS('',2,1,((#23712,#23713),(#23714,#23715),
(#23716,#23717)),.UNSPECIFIED.,.F.,.F.,.F.,(3,3),(2,2),(0.,1.),(0.,0.0300000000000002),
 .UNSPECIFIED.);
#841=B_SPLINE_SURFACE_WITH_KNOTS('',2,1,((#23723,#23724),(#23725,#23726),
(#23727,#23728)),.UNSPECIFIED.,.F.,.F.,.F.,(3,3),(2,2),(0.,1.),(0.,0.0300000000000002),
 .UNSPECIFIED.);
#842=B_SPLINE_SURFACE_WITH_KNOTS('',2,1,((#23734,#23735),(#23736,#23737),
(#23738,#23739)),.UNSPECIFIED.,.F.,.F.,.F.,(3,3),(2,2),(0.,1.),(0.,0.0300000000000002),
 .UNSPECIFIED.);
#843=B_SPLINE_SURFACE_WITH_KNOTS('',2,1,((#23745,#23746),(#23747,#23748),
(#23749,#23750)),.UNSPECIFIED.,.F.,.F.,.F.,(3,3),(2,2),(0.,1.),(0.,0.0300000000000002),
 .UNSPECIFIED.);
#844=B_SPLINE_SURFACE_WITH_KNOTS('',2,1,((#23756,#23757),(#23758,#23759),
(#23760,#23761)),.UNSPECIFIED.,.F.,.F.,.F.,(3,3),(2,2),(0.,1.),(0.,0.0300000000000002),
 .UNSPECIFIED.);
#845=B_SPLINE_SURFACE_WITH_KNOTS('',2,1,((#23767,#23768),(#23769,#23770),
(#23771,#23772)),.UNSPECIFIED.,.F.,.F.,.F.,(3,3),(2,2),(0.,1.),(0.,0.0300000000000002),
 .UNSPECIFIED.);
#846=B_SPLINE_SURFACE_WITH_KNOTS('',2,1,((#23778,#23779),(#23780,#23781),
(#23782,#23783)),.UNSPECIFIED.,.F.,.F.,.F.,(3,3),(2,2),(0.,1.),(0.,0.0300000000000002),
 .UNSPECIFIED.);
#847=B_SPLINE_SURFACE_WITH_KNOTS('',2,1,((#23789,#23790),(#23791,#23792),
(#23793,#23794)),.UNSPECIFIED.,.F.,.F.,.F.,(3,3),(2,2),(0.,1.),(0.,0.0300000000000002),
 .UNSPECIFIED.);
#848=B_SPLINE_SURFACE_WITH_KNOTS('',2,1,((#23800,#23801),(#23802,#23803),
(#23804,#23805)),.UNSPECIFIED.,.F.,.F.,.F.,(3,3),(2,2),(0.,1.),(0.,0.0300000000000002),
 .UNSPECIFIED.);
#849=B_SPLINE_SURFACE_WITH_KNOTS('',2,1,((#23811,#23812),(#23813,#23814),
(#23815,#23816)),.UNSPECIFIED.,.F.,.F.,.F.,(3,3),(2,2),(0.,1.),(0.,0.0300000000000002),
 .UNSPECIFIED.);
#850=B_SPLINE_SURFACE_WITH_KNOTS('',2,1,((#23822,#23823),(#23824,#23825),
(#23826,#23827)),.UNSPECIFIED.,.F.,.F.,.F.,(3,3),(2,2),(0.,1.),(0.,0.0300000000000002),
 .UNSPECIFIED.);
#851=B_SPLINE_SURFACE_WITH_KNOTS('',2,1,((#23833,#23834),(#23835,#23836),
(#23837,#23838)),.UNSPECIFIED.,.F.,.F.,.F.,(3,3),(2,2),(0.,1.),(0.,0.0300000000000002),
 .UNSPECIFIED.);
#852=B_SPLINE_SURFACE_WITH_KNOTS('',2,1,((#23844,#23845),(#23846,#23847),
(#23848,#23849)),.UNSPECIFIED.,.F.,.F.,.F.,(3,3),(2,2),(0.,1.),(0.,0.0300000000000002),
 .UNSPECIFIED.);
#853=B_SPLINE_SURFACE_WITH_KNOTS('',3,3,((#27715,#27716,#27717,#27718,#27719,
#27720,#27721,#27722,#27723,#27724,#27725,#27726,#27727,#27728,#27729,#27730,
#27731,#27732,#27733,#27734,#27735,#27736,#27737,#27738,#27739,#27740,#27741,
#27742,#27743,#27744,#27745,#27746,#27747,#27748,#27749,#27750,#27751,#27752,
#27753,#27754,#27755,#27756,#27757,#27758,#27759,#27760,#27761,#27762,#27763,
#27764,#27765,#27766,#27767,#27768,#27769,#27770,#27771,#27772,#27773,#27774,
#27775,#27776,#27777,#27778,#27779,#27780,#27781,#27782,#27783,#27784,#27785,
#27786,#27787,#27788,#27789,#27790,#27791,#27792,#27793,#27794,#27795,#27796,
#27797,#27798,#27799,#27800,#27801,#27802,#27803,#27804,#27805,#27806,#27807,
#27808,#27809,#27810,#27811,#27812,#27813,#27814,#27815,#27816,#27817,#27818,
#27819,#27820,#27821,#27822,#27823,#27824,#27825,#27826,#27827,#27828,#27829,
#27830,#27831,#27832,#27833,#27834,#27835,#27836,#27837,#27838,#27839,#27840,
#27841,#27842,#27843,#27844,#27845,#27846,#27847,#27848,#27849,#27850,#27851),
(#27852,#27853,#27854,#27855,#27856,#27857,#27858,#27859,#27860,#27861,
#27862,#27863,#27864,#27865,#27866,#27867,#27868,#27869,#27870,#27871,#27872,
#27873,#27874,#27875,#27876,#27877,#27878,#27879,#27880,#27881,#27882,#27883,
#27884,#27885,#27886,#27887,#27888,#27889,#27890,#27891,#27892,#27893,#27894,
#27895,#27896,#27897,#27898,#27899,#27900,#27901,#27902,#27903,#27904,#27905,
#27906,#27907,#27908,#27909,#27910,#27911,#27912,#27913,#27914,#27915,#27916,
#27917,#27918,#27919,#27920,#27921,#27922,#27923,#27924,#27925,#27926,#27927,
#27928,#27929,#27930,#27931,#27932,#27933,#27934,#27935,#27936,#27937,#27938,
#27939,#27940,#27941,#27942,#27943,#27944,#27945,#27946,#27947,#27948,#27949,
#27950,#27951,#27952,#27953,#27954,#27955,#27956,#27957,#27958,#27959,#27960,
#27961,#27962,#27963,#27964,#27965,#27966,#27967,#27968,#27969,#27970,#27971,
#27972,#27973,#27974,#27975,#27976,#27977,#27978,#27979,#27980,#27981,#27982,
#27983,#27984,#27985,#27986,#27987,#27988),(#27989,#27990,#27991,#27992,
#27993,#27994,#27995,#27996,#27997,#27998,#27999,#28000,#28001,#28002,#28003,
#28004,#28005,#28006,#28007,#28008,#28009,#28010,#28011,#28012,#28013,#28014,
#28015,#28016,#28017,#28018,#28019,#28020,#28021,#28022,#28023,#28024,#28025,
#28026,#28027,#28028,#28029,#28030,#28031,#28032,#28033,#28034,#28035,#28036,
#28037,#28038,#28039,#28040,#28041,#28042,#28043,#28044,#28045,#28046,#28047,
#28048,#28049,#28050,#28051,#28052,#28053,#28054,#28055,#28056,#28057,#28058,
#28059,#28060,#28061,#28062,#28063,#28064,#28065,#28066,#28067,#28068,#28069,
#28070,#28071,#28072,#28073,#28074,#28075,#28076,#28077,#28078,#28079,#28080,
#28081,#28082,#28083,#28084,#28085,#28086,#28087,#28088,#28089,#28090,#28091,
#28092,#28093,#28094,#28095,#28096,#28097,#28098,#28099,#28100,#28101,#28102,
#28103,#28104,#28105,#28106,#28107,#28108,#28109,#28110,#28111,#28112,#28113,
#28114,#28115,#28116,#28117,#28118,#28119,#28120,#28121,#28122,#28123,#28124,
#28125),(#28126,#28127,#28128,#28129,#28130,#28131,#28132,#28133,#28134,
#28135,#28136,#28137,#28138,#28139,#28140,#28141,#28142,#28143,#28144,#28145,
#28146,#28147,#28148,#28149,#28150,#28151,#28152,#28153,#28154,#28155,#28156,
#28157,#28158,#28159,#28160,#28161,#28162,#28163,#28164,#28165,#28166,#28167,
#28168,#28169,#28170,#28171,#28172,#28173,#28174,#28175,#28176,#28177,#28178,
#28179,#28180,#28181,#28182,#28183,#28184,#28185,#28186,#28187,#28188,#28189,
#28190,#28191,#28192,#28193,#28194,#28195,#28196,#28197,#28198,#28199,#28200,
#28201,#28202,#28203,#28204,#28205,#28206,#28207,#28208,#28209,#28210,#28211,
#28212,#28213,#28214,#28215,#28216,#28217,#28218,#28219,#28220,#28221,#28222,
#28223,#28224,#28225,#28226,#28227,#28228,#28229,#28230,#28231,#28232,#28233,
#28234,#28235,#28236,#28237,#28238,#28239,#28240,#28241,#28242,#28243,#28244,
#28245,#28246,#28247,#28248,#28249,#28250,#28251,#28252,#28253,#28254,#28255,
#28256,#28257,#28258,#28259,#28260,#28261,#28262)),.UNSPECIFIED.,.F.,.F.,
 .F.,(4,4),(4,1,1,1,1,1,1,1,1,1,1,1,1,1,1,1,1,1,1,1,1,1,1,1,1,1,1,1,1,1,
1,1,1,1,1,1,1,1,1,1,1,1,1,1,1,1,1,1,1,1,1,1,1,1,1,1,1,1,1,1,1,1,1,1,1,1,
1,1,1,1,1,1,1,1,1,1,1,1,1,1,1,1,1,1,1,1,1,1,1,1,1,1,1,1,1,1,1,1,1,1,1,1,
1,1,1,1,1,1,1,1,1,1,1,1,1,1,1,1,1,1,1,1,1,1,1,1,1,1,1,1,1,1,1,1,4),(0.,
0.0991945497494695),(8.29865039549515,8.79164514303176,9.28463989056837,
9.77763463810498,10.2706293856416,10.7636241331782,11.2566188807148,11.7496136282514,
12.242608375788,12.7356031233247,13.2285978708613,13.7215926183979,14.2145873659345,
14.7075821134711,15.2005768610077,15.6935716085443,16.1865663560809,16.6795611036176,
17.1725558511542,17.6655505986908,18.1585453462274,18.651540093764,19.1445348413006,
19.6375295888372,20.1305243363738,20.6235190839104,21.1165138314471,21.6095085789837,
22.1025033265203,22.5954980740569,23.0884928215935,23.5814875691301,24.0744823166667,
24.5674770642033,25.06047181174,25.5534665592766,26.0464613068132,26.5394560543498,
27.0324508018864,27.525445549423,28.0184402969596,28.5114350444962,29.0044297920328,
29.4974245395695,29.9904192871061,30.4834140346427,30.9764087821793,31.4694035297159,
31.9623982772525,32.4553930247891,32.9483877723257,33.4413825198624,33.934377267399,
34.4273720149356,34.9203667624722,35.4133615100088,35.9063562575454,36.399351005082,
36.8923457526186,37.3853405001553,37.8783352476919,38.3713299952285,38.8643247427651,
39.3573194903017,39.8503142378383,40.3433089853749,40.8363037329115,41.3292984804481,
41.8222932279848,42.3152879755214,42.808282723058,43.3012774705946,43.7942722181312,
44.2872669656678,44.7802617132044,45.273256460741,45.7662512082777,46.2592459558143,
46.7522407033509,47.2452354508875,47.7382301984241,48.2312249459607,48.7242196934973,
49.2172144410339,49.7102091885705,50.2032039361072,50.6961986836438,51.1891934311804,
51.682188178717,52.1751829262536,52.6681776737902,53.1611724213268,53.6541671688635,
54.1471619164001,54.6401566639367,55.1331514114733,55.6261461590099,56.1191409065465,
56.6121356540831,57.1051304016197,57.5981251491563,58.091119896693,58.5841146442296,
59.0771093917662,59.5701041393028,60.0630988868394,60.556093634376,61.0490883819126,
61.5420831294492,62.0350778769859,62.5280726245225,63.0210673720591,63.5140621195957,
64.0070568671323,64.5000516146689,64.9930463622055,65.4860411097421,65.9790358572787,
66.4720306048154,66.965025352352,67.4580200998886,67.9510148474252,68.4440095949618,
68.9370043424984,69.429999090035,69.9229938375716,70.4159885851083,70.9089833326449,
71.4019780801815,71.8949728277181,72.3879675752547,72.8809623227913,73.3739570703279,
73.8669518178645,74.3599465654011),.UNSPECIFIED.);
#854=B_SPLINE_SURFACE_WITH_KNOTS('',3,3,((#28295,#28296,#28297,#28298,#28299,
#28300,#28301,#28302,#28303,#28304,#28305,#28306,#28307,#28308,#28309,#28310,
#28311,#28312,#28313,#28314,#28315,#28316,#28317,#28318,#28319,#28320,#28321,
#28322,#28323,#28324,#28325,#28326,#28327,#28328,#28329,#28330,#28331,#28332,
#28333,#28334,#28335,#28336,#28337,#28338,#28339,#28340,#28341,#28342,#28343,
#28344,#28345,#28346,#28347,#28348,#28349,#28350,#28351,#28352,#28353,#28354,
#28355,#28356,#28357,#28358,#28359,#28360,#28361,#28362,#28363,#28364,#28365,
#28366,#28367,#28368,#28369,#28370,#28371,#28372,#28373,#28374,#28375,#28376,
#28377,#28378,#28379,#28380,#28381,#28382,#28383,#28384,#28385,#28386,#28387,
#28388,#28389,#28390,#28391,#28392,#28393,#28394,#28395,#28396,#28397,#28398,
#28399,#28400,#28401,#28402,#28403,#28404,#28405,#28406,#28407,#28408,#28409,
#28410,#28411,#28412,#28413,#28414,#28415,#28416,#28417,#28418,#28419,#28420,
#28421,#28422,#28423,#28424,#28425,#28426,#28427,#28428,#28429,#28430,#28431),
(#28432,#28433,#28434,#28435,#28436,#28437,#28438,#28439,#28440,#28441,
#28442,#28443,#28444,#28445,#28446,#28447,#28448,#28449,#28450,#28451,#28452,
#28453,#28454,#28455,#28456,#28457,#28458,#28459,#28460,#28461,#28462,#28463,
#28464,#28465,#28466,#28467,#28468,#28469,#28470,#28471,#28472,#28473,#28474,
#28475,#28476,#28477,#28478,#28479,#28480,#28481,#28482,#28483,#28484,#28485,
#28486,#28487,#28488,#28489,#28490,#28491,#28492,#28493,#28494,#28495,#28496,
#28497,#28498,#28499,#28500,#28501,#28502,#28503,#28504,#28505,#28506,#28507,
#28508,#28509,#28510,#28511,#28512,#28513,#28514,#28515,#28516,#28517,#28518,
#28519,#28520,#28521,#28522,#28523,#28524,#28525,#28526,#28527,#28528,#28529,
#28530,#28531,#28532,#28533,#28534,#28535,#28536,#28537,#28538,#28539,#28540,
#28541,#28542,#28543,#28544,#28545,#28546,#28547,#28548,#28549,#28550,#28551,
#28552,#28553,#28554,#28555,#28556,#28557,#28558,#28559,#28560,#28561,#28562,
#28563,#28564,#28565,#28566,#28567,#28568),(#28569,#28570,#28571,#28572,
#28573,#28574,#28575,#28576,#28577,#28578,#28579,#28580,#28581,#28582,#28583,
#28584,#28585,#28586,#28587,#28588,#28589,#28590,#28591,#28592,#28593,#28594,
#28595,#28596,#28597,#28598,#28599,#28600,#28601,#28602,#28603,#28604,#28605,
#28606,#28607,#28608,#28609,#28610,#28611,#28612,#28613,#28614,#28615,#28616,
#28617,#28618,#28619,#28620,#28621,#28622,#28623,#28624,#28625,#28626,#28627,
#28628,#28629,#28630,#28631,#28632,#28633,#28634,#28635,#28636,#28637,#28638,
#28639,#28640,#28641,#28642,#28643,#28644,#28645,#28646,#28647,#28648,#28649,
#28650,#28651,#28652,#28653,#28654,#28655,#28656,#28657,#28658,#28659,#28660,
#28661,#28662,#28663,#28664,#28665,#28666,#28667,#28668,#28669,#28670,#28671,
#28672,#28673,#28674,#28675,#28676,#28677,#28678,#28679,#28680,#28681,#28682,
#28683,#28684,#28685,#28686,#28687,#28688,#28689,#28690,#28691,#28692,#28693,
#28694,#28695,#28696,#28697,#28698,#28699,#28700,#28701,#28702,#28703,#28704,
#28705),(#28706,#28707,#28708,#28709,#28710,#28711,#28712,#28713,#28714,
#28715,#28716,#28717,#28718,#28719,#28720,#28721,#28722,#28723,#28724,#28725,
#28726,#28727,#28728,#28729,#28730,#28731,#28732,#28733,#28734,#28735,#28736,
#28737,#28738,#28739,#28740,#28741,#28742,#28743,#28744,#28745,#28746,#28747,
#28748,#28749,#28750,#28751,#28752,#28753,#28754,#28755,#28756,#28757,#28758,
#28759,#28760,#28761,#28762,#28763,#28764,#28765,#28766,#28767,#28768,#28769,
#28770,#28771,#28772,#28773,#28774,#28775,#28776,#28777,#28778,#28779,#28780,
#28781,#28782,#28783,#28784,#28785,#28786,#28787,#28788,#28789,#28790,#28791,
#28792,#28793,#28794,#28795,#28796,#28797,#28798,#28799,#28800,#28801,#28802,
#28803,#28804,#28805,#28806,#28807,#28808,#28809,#28810,#28811,#28812,#28813,
#28814,#28815,#28816,#28817,#28818,#28819,#28820,#28821,#28822,#28823,#28824,
#28825,#28826,#28827,#28828,#28829,#28830,#28831,#28832,#28833,#28834,#28835,
#28836,#28837,#28838,#28839,#28840,#28841,#28842)),.UNSPECIFIED.,.F.,.F.,
 .F.,(4,4),(4,1,1,1,1,1,1,1,1,1,1,1,1,1,1,1,1,1,1,1,1,1,1,1,1,1,1,1,1,1,
1,1,1,1,1,1,1,1,1,1,1,1,1,1,1,1,1,1,1,1,1,1,1,1,1,1,1,1,1,1,1,1,1,1,1,1,
1,1,1,1,1,1,1,1,1,1,1,1,1,1,1,1,1,1,1,1,1,1,1,1,1,1,1,1,1,1,1,1,1,1,1,1,
1,1,1,1,1,1,1,1,1,1,1,1,1,1,1,1,1,1,1,1,1,1,1,1,1,1,1,1,1,1,1,1,4),(0.,
0.0991945497494695),(11.6149723878394,12.107967135376,12.6009618829127,
13.0939566304493,13.5869513779859,14.0799461255225,14.5729408730591,15.0659356205957,
15.5589303681323,16.0519251156689,16.5449198632055,17.0379146107422,17.5309093582788,
18.0239041058154,18.516898853352,19.0098936008886,19.5028883484252,19.9958830959618,
20.4888778434984,20.9818725910351,21.4748673385717,21.9678620861083,22.4608568336449,
22.9538515811815,23.4468463287181,23.9398410762547,24.4328358237913,24.925830571328,
25.4188253188646,25.9118200664012,26.4048148139378,26.8978095614744,27.390804309011,
27.8837990565476,28.3767938040842,28.8697885516209,29.3627832991575,29.8557780466941,
30.3487727942307,30.8417675417673,31.3347622893039,31.8277570368405,32.3207517843771,
32.8137465319137,33.3067412794504,33.799736026987,34.2927307745236,34.7857255220602,
35.2787202695968,35.7717150171334,36.26470976467,36.7577045122066,37.2506992597433,
37.7436940072799,38.2366887548165,38.7296835023531,39.2226782498897,39.7156729974263,
40.2086677449629,40.7016624924995,41.1946572400362,41.6876519875728,42.1806467351094,
42.673641482646,43.1666362301826,43.6596309777192,44.1526257252558,44.6456204727924,
45.138615220329,45.6316099678657,46.1246047154023,46.6175994629389,47.1105942104755,
47.6035889580121,48.0965837055487,48.5895784530853,49.0825732006219,49.5755679481586,
50.0685626956952,50.5615574432318,51.0545521907684,51.547546938305,52.0405416858416,
52.5335364333782,53.0265311809148,53.5195259284514,54.0125206759881,54.5055154235247,
54.9985101710613,55.4915049185979,55.9844996661345,56.4774944136711,56.9704891612077,
57.4634839087443,57.956478656281,58.4494734038176,58.9424681513542,59.4354628988908,
59.9284576464274,60.421452393964,60.9144471415006,61.4074418890372,61.9004366365738,
62.3934313841105,62.8864261316471,63.3794208791837,63.8724156267203,64.3654103742569,
64.8584051217935,65.3513998693301,65.8443946168668,66.3373893644034,66.83038411194,
67.3233788594766,67.8163736070132,68.3093683545498,68.8023631020864,69.295357849623,
69.7883525971596,70.2813473446963,70.7743420922329,71.2673368397695,71.7603315873061,
72.2533263348427,72.7463210823793,73.2393158299159,73.7323105774525,74.2253053249892,
74.7183000725258,75.2112948200624,75.704289567599,76.1972843151356,76.6902790626722,
77.1832738102088,77.6762685577454),.UNSPECIFIED.);
#855=B_SPLINE_SURFACE_WITH_KNOTS('',3,3,((#28845,#28846,#28847,#28848,#28849,
#28850,#28851,#28852,#28853,#28854,#28855,#28856,#28857,#28858,#28859,#28860,
#28861,#28862,#28863,#28864,#28865,#28866,#28867,#28868,#28869,#28870,#28871,
#28872,#28873,#28874,#28875,#28876,#28877,#28878,#28879,#28880,#28881,#28882,
#28883,#28884,#28885,#28886,#28887,#28888,#28889,#28890,#28891,#28892,#28893,
#28894,#28895,#28896,#28897,#28898,#28899,#28900,#28901,#28902,#28903,#28904,
#28905,#28906,#28907,#28908,#28909,#28910,#28911,#28912,#28913,#28914,#28915,
#28916,#28917,#28918,#28919,#28920,#28921,#28922,#28923,#28924,#28925,#28926,
#28927,#28928,#28929,#28930,#28931,#28932,#28933,#28934,#28935,#28936,#28937,
#28938,#28939,#28940,#28941,#28942,#28943,#28944,#28945,#28946,#28947,#28948,
#28949,#28950,#28951,#28952,#28953,#28954,#28955,#28956,#28957,#28958,#28959,
#28960,#28961,#28962,#28963,#28964,#28965,#28966,#28967,#28968,#28969,#28970,
#28971,#28972,#28973,#28974,#28975,#28976,#28977,#28978,#28979,#28980,#28981,
#28982,#28983,#28984,#28985,#28986,#28987,#28988,#28989,#28990,#28991,#28992,
#28993,#28994,#28995,#28996,#28997,#28998,#28999,#29000,#29001,#29002,#29003,
#29004,#29005,#29006,#29007,#29008,#29009,#29010,#29011,#29012,#29013,#29014,
#29015,#29016,#29017,#29018,#29019,#29020,#29021,#29022,#29023,#29024,#29025,
#29026,#29027,#29028,#29029,#29030,#29031,#29032,#29033,#29034,#29035,#29036,
#29037,#29038,#29039,#29040,#29041,#29042,#29043,#29044,#29045,#29046,#29047),
(#29048,#29049,#29050,#29051,#29052,#29053,#29054,#29055,#29056,#29057,
#29058,#29059,#29060,#29061,#29062,#29063,#29064,#29065,#29066,#29067,#29068,
#29069,#29070,#29071,#29072,#29073,#29074,#29075,#29076,#29077,#29078,#29079,
#29080,#29081,#29082,#29083,#29084,#29085,#29086,#29087,#29088,#29089,#29090,
#29091,#29092,#29093,#29094,#29095,#29096,#29097,#29098,#29099,#29100,#29101,
#29102,#29103,#29104,#29105,#29106,#29107,#29108,#29109,#29110,#29111,#29112,
#29113,#29114,#29115,#29116,#29117,#29118,#29119,#29120,#29121,#29122,#29123,
#29124,#29125,#29126,#29127,#29128,#29129,#29130,#29131,#29132,#29133,#29134,
#29135,#29136,#29137,#29138,#29139,#29140,#29141,#29142,#29143,#29144,#29145,
#29146,#29147,#29148,#29149,#29150,#29151,#29152,#29153,#29154,#29155,#29156,
#29157,#29158,#29159,#29160,#29161,#29162,#29163,#29164,#29165,#29166,#29167,
#29168,#29169,#29170,#29171,#29172,#29173,#29174,#29175,#29176,#29177,#29178,
#29179,#29180,#29181,#29182,#29183,#29184,#29185,#29186,#29187,#29188,#29189,
#29190,#29191,#29192,#29193,#29194,#29195,#29196,#29197,#29198,#29199,#29200,
#29201,#29202,#29203,#29204,#29205,#29206,#29207,#29208,#29209,#29210,#29211,
#29212,#29213,#29214,#29215,#29216,#29217,#29218,#29219,#29220,#29221,#29222,
#29223,#29224,#29225,#29226,#29227,#29228,#29229,#29230,#29231,#29232,#29233,
#29234,#29235,#29236,#29237,#29238,#29239,#29240,#29241,#29242,#29243,#29244,
#29245,#29246,#29247,#29248,#29249,#29250),(#29251,#29252,#29253,#29254,
#29255,#29256,#29257,#29258,#29259,#29260,#29261,#29262,#29263,#29264,#29265,
#29266,#29267,#29268,#29269,#29270,#29271,#29272,#29273,#29274,#29275,#29276,
#29277,#29278,#29279,#29280,#29281,#29282,#29283,#29284,#29285,#29286,#29287,
#29288,#29289,#29290,#29291,#29292,#29293,#29294,#29295,#29296,#29297,#29298,
#29299,#29300,#29301,#29302,#29303,#29304,#29305,#29306,#29307,#29308,#29309,
#29310,#29311,#29312,#29313,#29314,#29315,#29316,#29317,#29318,#29319,#29320,
#29321,#29322,#29323,#29324,#29325,#29326,#29327,#29328,#29329,#29330,#29331,
#29332,#29333,#29334,#29335,#29336,#29337,#29338,#29339,#29340,#29341,#29342,
#29343,#29344,#29345,#29346,#29347,#29348,#29349,#29350,#29351,#29352,#29353,
#29354,#29355,#29356,#29357,#29358,#29359,#29360,#29361,#29362,#29363,#29364,
#29365,#29366,#29367,#29368,#29369,#29370,#29371,#29372,#29373,#29374,#29375,
#29376,#29377,#29378,#29379,#29380,#29381,#29382,#29383,#29384,#29385,#29386,
#29387,#29388,#29389,#29390,#29391,#29392,#29393,#29394,#29395,#29396,#29397,
#29398,#29399,#29400,#29401,#29402,#29403,#29404,#29405,#29406,#29407,#29408,
#29409,#29410,#29411,#29412,#29413,#29414,#29415,#29416,#29417,#29418,#29419,
#29420,#29421,#29422,#29423,#29424,#29425,#29426,#29427,#29428,#29429,#29430,
#29431,#29432,#29433,#29434,#29435,#29436,#29437,#29438,#29439,#29440,#29441,
#29442,#29443,#29444,#29445,#29446,#29447,#29448,#29449,#29450,#29451,#29452,
#29453),(#29454,#29455,#29456,#29457,#29458,#29459,#29460,#29461,#29462,
#29463,#29464,#29465,#29466,#29467,#29468,#29469,#29470,#29471,#29472,#29473,
#29474,#29475,#29476,#29477,#29478,#29479,#29480,#29481,#29482,#29483,#29484,
#29485,#29486,#29487,#29488,#29489,#29490,#29491,#29492,#29493,#29494,#29495,
#29496,#29497,#29498,#29499,#29500,#29501,#29502,#29503,#29504,#29505,#29506,
#29507,#29508,#29509,#29510,#29511,#29512,#29513,#29514,#29515,#29516,#29517,
#29518,#29519,#29520,#29521,#29522,#29523,#29524,#29525,#29526,#29527,#29528,
#29529,#29530,#29531,#29532,#29533,#29534,#29535,#29536,#29537,#29538,#29539,
#29540,#29541,#29542,#29543,#29544,#29545,#29546,#29547,#29548,#29549,#29550,
#29551,#29552,#29553,#29554,#29555,#29556,#29557,#29558,#29559,#29560,#29561,
#29562,#29563,#29564,#29565,#29566,#29567,#29568,#29569,#29570,#29571,#29572,
#29573,#29574,#29575,#29576,#29577,#29578,#29579,#29580,#29581,#29582,#29583,
#29584,#29585,#29586,#29587,#29588,#29589,#29590,#29591,#29592,#29593,#29594,
#29595,#29596,#29597,#29598,#29599,#29600,#29601,#29602,#29603,#29604,#29605,
#29606,#29607,#29608,#29609,#29610,#29611,#29612,#29613,#29614,#29615,#29616,
#29617,#29618,#29619,#29620,#29621,#29622,#29623,#29624,#29625,#29626,#29627,
#29628,#29629,#29630,#29631,#29632,#29633,#29634,#29635,#29636,#29637,#29638,
#29639,#29640,#29641,#29642,#29643,#29644,#29645,#29646,#29647,#29648,#29649,
#29650,#29651,#29652,#29653,#29654,#29655,#29656)),.UNSPECIFIED.,.F.,.F.,
 .F.,(4,4),(4,1,1,1,1,1,1,1,1,1,1,1,1,1,1,1,1,1,1,1,1,1,1,1,1,1,1,1,1,1,
1,1,1,1,1,1,1,1,1,1,1,1,1,1,1,1,1,1,1,1,1,1,1,1,1,1,1,1,1,1,1,1,1,1,1,1,
1,1,1,1,1,1,1,1,1,1,1,1,1,1,1,1,1,1,1,1,1,1,1,1,1,1,1,1,1,1,1,1,1,1,1,1,
1,1,1,1,1,1,1,1,1,1,1,1,1,1,1,1,1,1,1,1,1,1,1,1,1,1,1,1,1,1,1,1,1,1,1,1,
1,1,1,1,1,1,1,1,1,1,1,1,1,1,1,1,1,1,1,1,1,1,1,1,1,1,1,1,1,1,1,1,1,1,1,1,
1,1,1,1,1,1,1,1,1,1,1,1,1,1,1,1,1,1,1,1,1,1,1,1,1,1,4),(0.,0.0991945497494695),
(8.2986503954951,8.79650848453609,9.29436657357707,9.79222466261806,10.290082751659,
10.7879408407,11.285798929741,11.783657018782,12.281515107823,12.779373196864,
13.277231285905,13.7750893749459,14.2729474639869,14.7708055530279,15.2686636420689,
15.7665217311099,16.2643798201509,16.7622379091919,17.2600959982328,17.7579540872738,
18.2558121763148,18.7536702653558,19.2515283543968,19.7493864434378,20.2472445324787,
20.7451026215197,21.2429607105607,21.7408187996017,22.2386768886427,22.7365349776837,
23.2343930667247,23.7322511557656,24.2301092448066,24.7279673338476,25.2258254228886,
25.7236835119296,26.2215416009706,26.7193996900116,27.2172577790525,27.7151158680935,
28.2129739571345,28.7108320461755,29.2086901352165,29.7065482242575,30.2044063132985,
30.7022644023394,31.2001224913804,31.6979805804214,32.1958386694624,32.6936967585034,
33.1915548475444,33.6894129365854,34.1872710256263,34.6851291146673,35.1829872037083,
35.6808452927493,36.1787033817903,36.6765614708313,37.1744195598722,37.6722776489132,
38.1701357379542,38.6679938269952,39.1658519160362,39.6637100050772,40.1615680941182,
40.6594261831592,41.1572842722001,41.6551423612411,42.1530004502821,42.6508585393231,
43.1487166283641,43.6465747174051,44.144432806446,44.642290895487,45.140148984528,
45.638007073569,46.13586516261,46.633723251651,47.131581340692,47.6294394297329,
48.1272975187739,48.6251556078149,49.1230136968559,49.6208717858969,50.1187298749379,
50.6165879639789,51.1144460530198,51.6123041420608,52.1101622311018,52.6080203201428,
53.1058784091838,53.6037364982248,54.1015945872658,54.5994526763067,55.0973107653477,
55.5951688543887,56.0930269434297,56.5908850324707,57.0887431215117,57.5866012105526,
58.0844592995936,58.5823173886346,59.0801754776756,59.5780335667166,60.0758916557576,
60.5737497447986,61.0716078338395,61.5694659228805,62.0673240119215,62.5651821009625,
63.0630401900035,63.5608982790445,64.0587563680855,64.5566144571264,65.0544725461674,
65.5523306352084,66.0501887242494,66.5480468132904,67.0459049023314,67.5437629913723,
68.0416210804133,68.5394791694543,69.0373372584953,69.5351953475363,70.0330534365773,
70.5309115256183,71.0287696146593,71.5266277037002,72.0244857927412,72.5223438817822,
73.0202019708232,73.5180600598642,74.0159181489052,74.5137762379462,75.0116343269871,
75.5094924160281,76.0073505050691,76.5052085941101,77.0030666831511,77.5009247721921,
77.9987828612331,78.496640950274,78.994499039315,79.492357128356,79.990215217397,
80.488073306438,80.985931395479,81.4837894845199,81.9816475735609,82.4795056626019,
82.9773637516429,83.4752218406839,83.9730799297249,84.4709380187658,84.9687961078068,
85.4666541968478,85.9645122858888,86.4623703749298,86.9602284639708,87.4580865530118,
87.9559446420528,88.4538027310937,88.9516608201347,89.4495189091757,89.9473769982167,
90.4452350872577,90.9430931762987,91.4409512653396,91.9388093543806,92.4366674434216,
92.9345255324626,93.4323836215036,93.9302417105446,94.4280997995856,94.9259578886266,
95.4238159776675,95.9216740667085,96.4195321557495,96.9173902447905,97.4152483338315,
97.9131064228725,98.4109645119134,98.9088226009544,99.4066806899954,99.9045387790364,
100.402396868077,100.900254957118,101.398113046159,101.8959711352,102.393829224241,
102.891687313282,103.389545402323,103.887403491364,104.385261580405,104.883119669446,
105.380977758487,105.878835847528,106.376693936569,106.87455202561,107.372410114651,
107.870268203692),.UNSPECIFIED.);
#856=B_SPLINE_SURFACE_WITH_KNOTS('',3,3,((#30110,#30111,#30112,#30113,#30114,
#30115,#30116,#30117,#30118,#30119,#30120,#30121,#30122,#30123,#30124,#30125,
#30126,#30127,#30128,#30129,#30130,#30131,#30132,#30133,#30134,#30135,#30136,
#30137,#30138,#30139,#30140,#30141,#30142,#30143,#30144,#30145,#30146,#30147,
#30148,#30149,#30150,#30151,#30152,#30153,#30154,#30155,#30156,#30157,#30158,
#30159,#30160,#30161,#30162,#30163,#30164,#30165,#30166,#30167,#30168,#30169,
#30170,#30171,#30172,#30173,#30174,#30175,#30176,#30177,#30178,#30179,#30180,
#30181,#30182,#30183,#30184,#30185,#30186,#30187,#30188,#30189,#30190,#30191,
#30192,#30193,#30194,#30195,#30196,#30197,#30198,#30199,#30200,#30201,#30202,
#30203,#30204,#30205,#30206,#30207,#30208,#30209,#30210,#30211,#30212,#30213,
#30214,#30215,#30216,#30217,#30218,#30219,#30220,#30221,#30222,#30223,#30224,
#30225,#30226,#30227,#30228,#30229,#30230,#30231,#30232,#30233,#30234,#30235,
#30236,#30237,#30238,#30239,#30240,#30241,#30242,#30243,#30244,#30245,#30246,
#30247,#30248,#30249,#30250,#30251,#30252,#30253,#30254,#30255,#30256,#30257,
#30258,#30259,#30260,#30261,#30262,#30263,#30264,#30265,#30266,#30267,#30268,
#30269,#30270,#30271,#30272,#30273,#30274,#30275,#30276,#30277,#30278,#30279,
#30280,#30281,#30282,#30283,#30284,#30285,#30286,#30287,#30288,#30289,#30290,
#30291,#30292,#30293,#30294,#30295,#30296,#30297,#30298,#30299,#30300,#30301,
#30302,#30303,#30304,#30305,#30306,#30307,#30308,#30309,#30310,#30311,#30312),
(#30313,#30314,#30315,#30316,#30317,#30318,#30319,#30320,#30321,#30322,
#30323,#30324,#30325,#30326,#30327,#30328,#30329,#30330,#30331,#30332,#30333,
#30334,#30335,#30336,#30337,#30338,#30339,#30340,#30341,#30342,#30343,#30344,
#30345,#30346,#30347,#30348,#30349,#30350,#30351,#30352,#30353,#30354,#30355,
#30356,#30357,#30358,#30359,#30360,#30361,#30362,#30363,#30364,#30365,#30366,
#30367,#30368,#30369,#30370,#30371,#30372,#30373,#30374,#30375,#30376,#30377,
#30378,#30379,#30380,#30381,#30382,#30383,#30384,#30385,#30386,#30387,#30388,
#30389,#30390,#30391,#30392,#30393,#30394,#30395,#30396,#30397,#30398,#30399,
#30400,#30401,#30402,#30403,#30404,#30405,#30406,#30407,#30408,#30409,#30410,
#30411,#30412,#30413,#30414,#30415,#30416,#30417,#30418,#30419,#30420,#30421,
#30422,#30423,#30424,#30425,#30426,#30427,#30428,#30429,#30430,#30431,#30432,
#30433,#30434,#30435,#30436,#30437,#30438,#30439,#30440,#30441,#30442,#30443,
#30444,#30445,#30446,#30447,#30448,#30449,#30450,#30451,#30452,#30453,#30454,
#30455,#30456,#30457,#30458,#30459,#30460,#30461,#30462,#30463,#30464,#30465,
#30466,#30467,#30468,#30469,#30470,#30471,#30472,#30473,#30474,#30475,#30476,
#30477,#30478,#30479,#30480,#30481,#30482,#30483,#30484,#30485,#30486,#30487,
#30488,#30489,#30490,#30491,#30492,#30493,#30494,#30495,#30496,#30497,#30498,
#30499,#30500,#30501,#30502,#30503,#30504,#30505,#30506,#30507,#30508,#30509,
#30510,#30511,#30512,#30513,#30514,#30515),(#30516,#30517,#30518,#30519,
#30520,#30521,#30522,#30523,#30524,#30525,#30526,#30527,#30528,#30529,#30530,
#30531,#30532,#30533,#30534,#30535,#30536,#30537,#30538,#30539,#30540,#30541,
#30542,#30543,#30544,#30545,#30546,#30547,#30548,#30549,#30550,#30551,#30552,
#30553,#30554,#30555,#30556,#30557,#30558,#30559,#30560,#30561,#30562,#30563,
#30564,#30565,#30566,#30567,#30568,#30569,#30570,#30571,#30572,#30573,#30574,
#30575,#30576,#30577,#30578,#30579,#30580,#30581,#30582,#30583,#30584,#30585,
#30586,#30587,#30588,#30589,#30590,#30591,#30592,#30593,#30594,#30595,#30596,
#30597,#30598,#30599,#30600,#30601,#30602,#30603,#30604,#30605,#30606,#30607,
#30608,#30609,#30610,#30611,#30612,#30613,#30614,#30615,#30616,#30617,#30618,
#30619,#30620,#30621,#30622,#30623,#30624,#30625,#30626,#30627,#30628,#30629,
#30630,#30631,#30632,#30633,#30634,#30635,#30636,#30637,#30638,#30639,#30640,
#30641,#30642,#30643,#30644,#30645,#30646,#30647,#30648,#30649,#30650,#30651,
#30652,#30653,#30654,#30655,#30656,#30657,#30658,#30659,#30660,#30661,#30662,
#30663,#30664,#30665,#30666,#30667,#30668,#30669,#30670,#30671,#30672,#30673,
#30674,#30675,#30676,#30677,#30678,#30679,#30680,#30681,#30682,#30683,#30684,
#30685,#30686,#30687,#30688,#30689,#30690,#30691,#30692,#30693,#30694,#30695,
#30696,#30697,#30698,#30699,#30700,#30701,#30702,#30703,#30704,#30705,#30706,
#30707,#30708,#30709,#30710,#30711,#30712,#30713,#30714,#30715,#30716,#30717,
#30718),(#30719,#30720,#30721,#30722,#30723,#30724,#30725,#30726,#30727,
#30728,#30729,#30730,#30731,#30732,#30733,#30734,#30735,#30736,#30737,#30738,
#30739,#30740,#30741,#30742,#30743,#30744,#30745,#30746,#30747,#30748,#30749,
#30750,#30751,#30752,#30753,#30754,#30755,#30756,#30757,#30758,#30759,#30760,
#30761,#30762,#30763,#30764,#30765,#30766,#30767,#30768,#30769,#30770,#30771,
#30772,#30773,#30774,#30775,#30776,#30777,#30778,#30779,#30780,#30781,#30782,
#30783,#30784,#30785,#30786,#30787,#30788,#30789,#30790,#30791,#30792,#30793,
#30794,#30795,#30796,#30797,#30798,#30799,#30800,#30801,#30802,#30803,#30804,
#30805,#30806,#30807,#30808,#30809,#30810,#30811,#30812,#30813,#30814,#30815,
#30816,#30817,#30818,#30819,#30820,#30821,#30822,#30823,#30824,#30825,#30826,
#30827,#30828,#30829,#30830,#30831,#30832,#30833,#30834,#30835,#30836,#30837,
#30838,#30839,#30840,#30841,#30842,#30843,#30844,#30845,#30846,#30847,#30848,
#30849,#30850,#30851,#30852,#30853,#30854,#30855,#30856,#30857,#30858,#30859,
#30860,#30861,#30862,#30863,#30864,#30865,#30866,#30867,#30868,#30869,#30870,
#30871,#30872,#30873,#30874,#30875,#30876,#30877,#30878,#30879,#30880,#30881,
#30882,#30883,#30884,#30885,#30886,#30887,#30888,#30889,#30890,#30891,#30892,
#30893,#30894,#30895,#30896,#30897,#30898,#30899,#30900,#30901,#30902,#30903,
#30904,#30905,#30906,#30907,#30908,#30909,#30910,#30911,#30912,#30913,#30914,
#30915,#30916,#30917,#30918,#30919,#30920,#30921)),.UNSPECIFIED.,.F.,.F.,
 .F.,(4,4),(4,1,1,1,1,1,1,1,1,1,1,1,1,1,1,1,1,1,1,1,1,1,1,1,1,1,1,1,1,1,
1,1,1,1,1,1,1,1,1,1,1,1,1,1,1,1,1,1,1,1,1,1,1,1,1,1,1,1,1,1,1,1,1,1,1,1,
1,1,1,1,1,1,1,1,1,1,1,1,1,1,1,1,1,1,1,1,1,1,1,1,1,1,1,1,1,1,1,1,1,1,1,1,
1,1,1,1,1,1,1,1,1,1,1,1,1,1,1,1,1,1,1,1,1,1,1,1,1,1,1,1,1,1,1,1,1,1,1,1,
1,1,1,1,1,1,1,1,1,1,1,1,1,1,1,1,1,1,1,1,1,1,1,1,1,1,1,1,1,1,1,1,1,1,1,1,
1,1,1,1,1,1,1,1,1,1,1,1,1,1,1,1,1,1,1,1,1,1,1,1,1,1,4),(0.,0.0991945497494695),
(11.6149723878395,12.1128304768804,12.6106885659214,13.1085466549624,13.6064047440034,
14.1042628330444,14.6021209220854,15.0999790111264,15.5978371001673,16.0956951892083,
16.5935532782493,17.0914113672903,17.5892694563313,18.0871275453723,18.5849856344133,
19.0828437234542,19.5807018124952,20.0785599015362,20.5764179905772,21.0742760796182,
21.5721341686592,22.0699922577002,22.5678503467411,23.0657084357821,23.5635665248231,
24.0614246138641,24.5592827029051,25.0571407919461,25.554998880987,26.052856970028,
26.550715059069,27.04857314811,27.546431237151,28.044289326192,28.542147415233,
29.0400055042739,29.5378635933149,30.0357216823559,30.5335797713969,31.0314378604379,
31.5292959494789,32.0271540385199,32.5250121275608,33.0228702166018,33.5207283056428,
34.0185863946838,34.5164444837248,35.0143025727658,35.5121606618068,36.0100187508477,
36.5078768398887,37.0057349289297,37.5035930179707,38.0014511070117,38.4993091960527,
38.9971672850937,39.4950253741346,39.9928834631756,40.4907415522166,40.9885996412576,
41.4864577302986,41.9843158193396,42.4821739083806,42.9800319974215,43.4778900864625,
43.9757481755035,44.4736062645445,44.9714643535855,45.4693224426265,45.9671805316675,
46.4650386207084,46.9628967097494,47.4607547987904,47.9586128878314,48.4564709768724,
48.9543290659134,49.4521871549543,49.9500452439953,50.4479033330363,50.9457614220773,
51.4436195111183,51.9414776001593,52.4393356892003,52.9371937782412,53.4350518672822,
53.9329099563232,54.4307680453642,54.9286261344052,55.4264842234462,55.9243423124872,
56.4222004015281,56.9200584905691,57.4179165796101,57.9157746686511,58.4136327576921,
58.9114908467331,59.409348935774,59.907207024815,60.405065113856,60.902923202897,
61.400781291938,61.898639380979,62.39649747002,62.8943555590609,63.3922136481019,
63.8900717371429,64.3879298261839,64.8857879152249,65.3836460042659,65.8815040933069,
66.3793621823478,66.8772202713888,67.3750783604298,67.8729364494708,68.3707945385118,
68.8686526275528,69.3665107165938,69.8643688056347,70.3622268946757,70.8600849837167,
71.3579430727577,71.8558011617987,72.3536592508397,72.8515173398807,73.3493754289216,
73.8472335179626,74.3450916070036,74.8429496960446,75.3408077850856,75.8386658741266,
76.3365239631676,76.8343820522085,77.3322401412495,77.8300982302905,78.3279563193315,
78.8258144083725,79.3236724974135,79.8215305864545,80.3193886754954,80.8172467645364,
81.3151048535774,81.8129629426184,82.3108210316594,82.8086791207004,83.3065372097414,
83.8043952987823,84.3022533878233,84.8001114768643,85.2979695659053,85.7958276549463,
86.2936857439873,86.7915438330282,87.2894019220692,87.7872600111102,88.2851181001512,
88.7829761891922,89.2808342782332,89.7786923672741,90.2765504563151,90.7744085453561,
91.2722666343971,91.7701247234381,92.2679828124791,92.7658409015201,93.2636989905611,
93.761557079602,94.259415168643,94.757273257684,95.255131346725,95.752989435766,
96.250847524807,96.7487056138479,97.2465637028889,97.7444217919299,98.2422798809709,
98.7401379700119,99.2379960590529,99.7358541480939,100.233712237135,100.731570326176,
101.229428415217,101.727286504258,102.225144593299,102.72300268234,103.220860771381,
103.718718860422,104.216576949463,104.714435038504,105.212293127545,105.710151216586,
106.208009305627,106.705867394668,107.203725483709,107.70158357275,108.199441661791,
108.697299750832,109.195157839873,109.693015928914,110.190874017955,110.688732106996,
111.186590196037),.UNSPECIFIED.);
#857=B_SPLINE_SURFACE_WITH_KNOTS('',3,3,((#31396,#31397,#31398,#31399,#31400,
#31401,#31402,#31403,#31404,#31405,#31406,#31407,#31408,#31409,#31410,#31411,
#31412,#31413,#31414,#31415,#31416,#31417,#31418,#31419,#31420,#31421,#31422,
#31423,#31424,#31425,#31426,#31427,#31428,#31429,#31430,#31431,#31432,#31433,
#31434,#31435,#31436,#31437,#31438,#31439,#31440,#31441,#31442,#31443,#31444,
#31445,#31446,#31447,#31448,#31449,#31450,#31451,#31452,#31453,#31454,#31455,
#31456,#31457,#31458,#31459,#31460,#31461,#31462,#31463,#31464,#31465,#31466,
#31467,#31468,#31469,#31470),(#31471,#31472,#31473,#31474,#31475,#31476,
#31477,#31478,#31479,#31480,#31481,#31482,#31483,#31484,#31485,#31486,#31487,
#31488,#31489,#31490,#31491,#31492,#31493,#31494,#31495,#31496,#31497,#31498,
#31499,#31500,#31501,#31502,#31503,#31504,#31505,#31506,#31507,#31508,#31509,
#31510,#31511,#31512,#31513,#31514,#31515,#31516,#31517,#31518,#31519,#31520,
#31521,#31522,#31523,#31524,#31525,#31526,#31527,#31528,#31529,#31530,#31531,
#31532,#31533,#31534,#31535,#31536,#31537,#31538,#31539,#31540,#31541,#31542,
#31543,#31544,#31545),(#31546,#31547,#31548,#31549,#31550,#31551,#31552,
#31553,#31554,#31555,#31556,#31557,#31558,#31559,#31560,#31561,#31562,#31563,
#31564,#31565,#31566,#31567,#31568,#31569,#31570,#31571,#31572,#31573,#31574,
#31575,#31576,#31577,#31578,#31579,#31580,#31581,#31582,#31583,#31584,#31585,
#31586,#31587,#31588,#31589,#31590,#31591,#31592,#31593,#31594,#31595,#31596,
#31597,#31598,#31599,#31600,#31601,#31602,#31603,#31604,#31605,#31606,#31607,
#31608,#31609,#31610,#31611,#31612,#31613,#31614,#31615,#31616,#31617,#31618,
#31619,#31620),(#31621,#31622,#31623,#31624,#31625,#31626,#31627,#31628,
#31629,#31630,#31631,#31632,#31633,#31634,#31635,#31636,#31637,#31638,#31639,
#31640,#31641,#31642,#31643,#31644,#31645,#31646,#31647,#31648,#31649,#31650,
#31651,#31652,#31653,#31654,#31655,#31656,#31657,#31658,#31659,#31660,#31661,
#31662,#31663,#31664,#31665,#31666,#31667,#31668,#31669,#31670,#31671,#31672,
#31673,#31674,#31675,#31676,#31677,#31678,#31679,#31680,#31681,#31682,#31683,
#31684,#31685,#31686,#31687,#31688,#31689,#31690,#31691,#31692,#31693,#31694,
#31695),(#31696,#31697,#31698,#31699,#31700,#31701,#31702,#31703,#31704,
#31705,#31706,#31707,#31708,#31709,#31710,#31711,#31712,#31713,#31714,#31715,
#31716,#31717,#31718,#31719,#31720,#31721,#31722,#31723,#31724,#31725,#31726,
#31727,#31728,#31729,#31730,#31731,#31732,#31733,#31734,#31735,#31736,#31737,
#31738,#31739,#31740,#31741,#31742,#31743,#31744,#31745,#31746,#31747,#31748,
#31749,#31750,#31751,#31752,#31753,#31754,#31755,#31756,#31757,#31758,#31759,
#31760,#31761,#31762,#31763,#31764,#31765,#31766,#31767,#31768,#31769,#31770),
(#31771,#31772,#31773,#31774,#31775,#31776,#31777,#31778,#31779,#31780,
#31781,#31782,#31783,#31784,#31785,#31786,#31787,#31788,#31789,#31790,#31791,
#31792,#31793,#31794,#31795,#31796,#31797,#31798,#31799,#31800,#31801,#31802,
#31803,#31804,#31805,#31806,#31807,#31808,#31809,#31810,#31811,#31812,#31813,
#31814,#31815,#31816,#31817,#31818,#31819,#31820,#31821,#31822,#31823,#31824,
#31825,#31826,#31827,#31828,#31829,#31830,#31831,#31832,#31833,#31834,#31835,
#31836,#31837,#31838,#31839,#31840,#31841,#31842,#31843,#31844,#31845),
(#31846,#31847,#31848,#31849,#31850,#31851,#31852,#31853,#31854,#31855,
#31856,#31857,#31858,#31859,#31860,#31861,#31862,#31863,#31864,#31865,#31866,
#31867,#31868,#31869,#31870,#31871,#31872,#31873,#31874,#31875,#31876,#31877,
#31878,#31879,#31880,#31881,#31882,#31883,#31884,#31885,#31886,#31887,#31888,
#31889,#31890,#31891,#31892,#31893,#31894,#31895,#31896,#31897,#31898,#31899,
#31900,#31901,#31902,#31903,#31904,#31905,#31906,#31907,#31908,#31909,#31910,
#31911,#31912,#31913,#31914,#31915,#31916,#31917,#31918,#31919,#31920),
(#31921,#31922,#31923,#31924,#31925,#31926,#31927,#31928,#31929,#31930,
#31931,#31932,#31933,#31934,#31935,#31936,#31937,#31938,#31939,#31940,#31941,
#31942,#31943,#31944,#31945,#31946,#31947,#31948,#31949,#31950,#31951,#31952,
#31953,#31954,#31955,#31956,#31957,#31958,#31959,#31960,#31961,#31962,#31963,
#31964,#31965,#31966,#31967,#31968,#31969,#31970,#31971,#31972,#31973,#31974,
#31975,#31976,#31977,#31978,#31979,#31980,#31981,#31982,#31983,#31984,#31985,
#31986,#31987,#31988,#31989,#31990,#31991,#31992,#31993,#31994,#31995),
(#31996,#31997,#31998,#31999,#32000,#32001,#32002,#32003,#32004,#32005,
#32006,#32007,#32008,#32009,#32010,#32011,#32012,#32013,#32014,#32015,#32016,
#32017,#32018,#32019,#32020,#32021,#32022,#32023,#32024,#32025,#32026,#32027,
#32028,#32029,#32030,#32031,#32032,#32033,#32034,#32035,#32036,#32037,#32038,
#32039,#32040,#32041,#32042,#32043,#32044,#32045,#32046,#32047,#32048,#32049,
#32050,#32051,#32052,#32053,#32054,#32055,#32056,#32057,#32058,#32059,#32060,
#32061,#32062,#32063,#32064,#32065,#32066,#32067,#32068,#32069,#32070),
(#32071,#32072,#32073,#32074,#32075,#32076,#32077,#32078,#32079,#32080,
#32081,#32082,#32083,#32084,#32085,#32086,#32087,#32088,#32089,#32090,#32091,
#32092,#32093,#32094,#32095,#32096,#32097,#32098,#32099,#32100,#32101,#32102,
#32103,#32104,#32105,#32106,#32107,#32108,#32109,#32110,#32111,#32112,#32113,
#32114,#32115,#32116,#32117,#32118,#32119,#32120,#32121,#32122,#32123,#32124,
#32125,#32126,#32127,#32128,#32129,#32130,#32131,#32132,#32133,#32134,#32135,
#32136,#32137,#32138,#32139,#32140,#32141,#32142,#32143,#32144,#32145)),
 .UNSPECIFIED.,.T.,.F.,.F.,(4,1,1,1,1,1,1,4),(4,1,1,1,1,1,1,1,1,1,1,1,1,
1,1,1,1,1,1,1,1,1,1,1,1,1,1,1,1,1,1,1,1,1,1,1,1,1,1,1,1,1,1,1,1,1,1,1,1,
1,1,1,1,1,1,1,1,1,1,1,1,1,1,1,1,1,1,1,1,1,1,1,4),(-3.14159265358979,-2.24399475256414,
-1.34639685153848,-0.448798950512828,0.448798950512828,1.34639685153848,
2.24399475256414,3.14159265358979),(0.,0.00892857142857143,0.0178571428571429,
0.0357142857142857,0.0535714285714286,0.0714285714285714,0.0892857142857143,
0.107142857142857,0.116071428571429,0.125,0.133928571428571,0.142857142857143,
0.154761904761905,0.166666666666667,0.178571428571429,0.19047619047619,
0.202380952380952,0.214285714285714,0.232142857142857,0.25,0.267857142857143,
0.285714285714286,0.303571428571429,0.321428571428571,0.339285714285714,
0.357142857142857,0.376984126984127,0.380952380952381,0.392857142857143,
0.404761904761905,0.416666666666667,0.428571428571429,0.44047619047619,
0.452380952380952,0.464285714285714,0.476190476190476,0.492063492063492,
0.5,0.517857142857143,0.535714285714286,0.553571428571429,0.571428571428571,
0.589285714285714,0.607142857142857,0.625,0.642857142857143,0.654761904761905,
0.666666666666667,0.678571428571428,0.69047619047619,0.702380952380952,
0.714285714285714,0.726190476190476,0.738095238095238,0.75,0.761904761904762,
0.773809523809524,0.785714285714286,0.797619047619047,0.809523809523809,
0.821428571428571,0.833333333333333,0.845238095238095,0.857142857142857,
0.875,0.892857142857143,0.910714285714286,0.928571428571429,0.946428571428571,
0.964285714285714,0.982142857142857,0.991071428571429,1.),.UNSPECIFIED.);
#858=B_SPLINE_SURFACE_WITH_KNOTS('',2,1,((#32703,#32704),(#32705,#32706),
(#32707,#32708)),.UNSPECIFIED.,.F.,.F.,.F.,(3,3),(2,2),(0.,1.),(0.,0.0249999999999999),
 .UNSPECIFIED.);
#859=B_SPLINE_SURFACE_WITH_KNOTS('',2,1,((#32716,#32717),(#32718,#32719),
(#32720,#32721)),.UNSPECIFIED.,.F.,.F.,.F.,(3,3),(2,2),(0.,1.),(0.,0.0249999999999999),
 .UNSPECIFIED.);
#860=B_SPLINE_SURFACE_WITH_KNOTS('',2,1,((#32747,#32748),(#32749,#32750),
(#32751,#32752)),.UNSPECIFIED.,.F.,.F.,.F.,(3,3),(2,2),(0.,1.),(0.,0.0249999999999999),
 .UNSPECIFIED.);
#861=B_SPLINE_SURFACE_WITH_KNOTS('',2,1,((#32758,#32759),(#32760,#32761),
(#32762,#32763)),.UNSPECIFIED.,.F.,.F.,.F.,(3,3),(2,2),(0.,1.),(0.,0.0249999999999999),
 .UNSPECIFIED.);
#862=B_SPLINE_SURFACE_WITH_KNOTS('',2,1,((#32781,#32782),(#32783,#32784),
(#32785,#32786)),.UNSPECIFIED.,.F.,.F.,.F.,(3,3),(2,2),(0.,1.),(0.,0.0249999999999999),
 .UNSPECIFIED.);
#863=B_SPLINE_SURFACE_WITH_KNOTS('',2,1,((#32792,#32793),(#32794,#32795),
(#32796,#32797)),.UNSPECIFIED.,.F.,.F.,.F.,(3,3),(2,2),(0.,1.),(0.,0.0249999999999999),
 .UNSPECIFIED.);
#864=B_SPLINE_SURFACE_WITH_KNOTS('',2,1,((#32855,#32856),(#32857,#32858),
(#32859,#32860)),.UNSPECIFIED.,.F.,.F.,.F.,(3,3),(2,2),(0.,1.),(0.,0.0249999999999999),
 .UNSPECIFIED.);
#865=B_SPLINE_SURFACE_WITH_KNOTS('',2,1,((#32868,#32869),(#32870,#32871),
(#32872,#32873)),.UNSPECIFIED.,.F.,.F.,.F.,(3,3),(2,2),(0.,1.),(0.,0.0249999999999999),
 .UNSPECIFIED.);
#866=B_SPLINE_SURFACE_WITH_KNOTS('',2,1,((#32879,#32880),(#32881,#32882),
(#32883,#32884)),.UNSPECIFIED.,.F.,.F.,.F.,(3,3),(2,2),(0.,1.),(0.,0.0249999999999999),
 .UNSPECIFIED.);
#867=B_SPLINE_SURFACE_WITH_KNOTS('',2,1,((#32890,#32891),(#32892,#32893),
(#32894,#32895)),.UNSPECIFIED.,.F.,.F.,.F.,(3,3),(2,2),(0.,1.),(0.,0.0249999999999999),
 .UNSPECIFIED.);
#868=B_SPLINE_SURFACE_WITH_KNOTS('',2,1,((#32901,#32902),(#32903,#32904),
(#32905,#32906)),.UNSPECIFIED.,.F.,.F.,.F.,(3,3),(2,2),(0.,1.),(0.,0.0249999999999999),
 .UNSPECIFIED.);
#869=B_SPLINE_SURFACE_WITH_KNOTS('',2,1,((#32912,#32913),(#32914,#32915),
(#32916,#32917)),.UNSPECIFIED.,.F.,.F.,.F.,(3,3),(2,2),(0.,1.),(0.,0.0249999999999999),
 .UNSPECIFIED.);
#870=B_SPLINE_SURFACE_WITH_KNOTS('',2,1,((#32923,#32924),(#32925,#32926),
(#32927,#32928)),.UNSPECIFIED.,.F.,.F.,.F.,(3,3),(2,2),(0.,1.),(0.,0.0249999999999999),
 .UNSPECIFIED.);
#871=B_SPLINE_SURFACE_WITH_KNOTS('',2,1,((#32934,#32935),(#32936,#32937),
(#32938,#32939)),.UNSPECIFIED.,.F.,.F.,.F.,(3,3),(2,2),(0.,1.),(0.,0.0249999999999999),
 .UNSPECIFIED.);
#872=B_SPLINE_SURFACE_WITH_KNOTS('',2,1,((#32945,#32946),(#32947,#32948),
(#32949,#32950)),.UNSPECIFIED.,.F.,.F.,.F.,(3,3),(2,2),(0.,1.),(0.,0.0249999999999999),
 .UNSPECIFIED.);
#873=B_SPLINE_SURFACE_WITH_KNOTS('',2,1,((#32956,#32957),(#32958,#32959),
(#32960,#32961)),.UNSPECIFIED.,.F.,.F.,.F.,(3,3),(2,2),(0.,1.),(0.,0.0249999999999999),
 .UNSPECIFIED.);
#874=B_SPLINE_SURFACE_WITH_KNOTS('',2,1,((#32967,#32968),(#32969,#32970),
(#32971,#32972)),.UNSPECIFIED.,.F.,.F.,.F.,(3,3),(2,2),(0.,1.),(0.,0.0249999999999999),
 .UNSPECIFIED.);
#875=B_SPLINE_SURFACE_WITH_KNOTS('',2,1,((#32978,#32979),(#32980,#32981),
(#32982,#32983)),.UNSPECIFIED.,.F.,.F.,.F.,(3,3),(2,2),(0.,1.),(0.,0.0249999999999999),
 .UNSPECIFIED.);
#876=B_SPLINE_SURFACE_WITH_KNOTS('',2,1,((#32988,#32989),(#32990,#32991),
(#32992,#32993)),.UNSPECIFIED.,.F.,.F.,.F.,(3,3),(2,2),(0.,1.),(0.,0.0249999999999999),
 .UNSPECIFIED.);
#877=B_SPLINE_SURFACE_WITH_KNOTS('',2,1,((#33001,#33002),(#33003,#33004),
(#33005,#33006)),.UNSPECIFIED.,.F.,.F.,.F.,(3,3),(2,2),(0.,1.),(0.,0.0249999999999999),
 .UNSPECIFIED.);
#878=B_SPLINE_SURFACE_WITH_KNOTS('',2,1,((#33016,#33017),(#33018,#33019),
(#33020,#33021)),.UNSPECIFIED.,.F.,.F.,.F.,(3,3),(2,2),(0.,1.),(0.,0.0249999999999999),
 .UNSPECIFIED.);
#879=B_SPLINE_SURFACE_WITH_KNOTS('',2,1,((#33027,#33028),(#33029,#33030),
(#33031,#33032)),.UNSPECIFIED.,.F.,.F.,.F.,(3,3),(2,2),(0.,1.),(0.,0.0249999999999999),
 .UNSPECIFIED.);
#880=B_SPLINE_SURFACE_WITH_KNOTS('',2,1,((#33053,#33054),(#33055,#33056),
(#33057,#33058)),.UNSPECIFIED.,.F.,.F.,.F.,(3,3),(2,2),(0.,1.),(0.,0.0249999999999999),
 .UNSPECIFIED.);
#881=B_SPLINE_SURFACE_WITH_KNOTS('',2,1,((#33066,#33067),(#33068,#33069),
(#33070,#33071)),.UNSPECIFIED.,.F.,.F.,.F.,(3,3),(2,2),(0.,1.),(0.,0.0249999999999999),
 .UNSPECIFIED.);
#882=B_SPLINE_SURFACE_WITH_KNOTS('',2,1,((#33077,#33078),(#33079,#33080),
(#33081,#33082)),.UNSPECIFIED.,.F.,.F.,.F.,(3,3),(2,2),(0.,1.),(0.,0.0249999999999999),
 .UNSPECIFIED.);
#883=B_SPLINE_SURFACE_WITH_KNOTS('',2,1,((#33088,#33089),(#33090,#33091),
(#33092,#33093)),.UNSPECIFIED.,.F.,.F.,.F.,(3,3),(2,2),(0.,1.),(0.,0.0249999999999999),
 .UNSPECIFIED.);
#884=B_SPLINE_SURFACE_WITH_KNOTS('',2,1,((#33099,#33100),(#33101,#33102),
(#33103,#33104)),.UNSPECIFIED.,.F.,.F.,.F.,(3,3),(2,2),(0.,1.),(0.,0.0249999999999999),
 .UNSPECIFIED.);
#885=B_SPLINE_SURFACE_WITH_KNOTS('',2,1,((#33110,#33111),(#33112,#33113),
(#33114,#33115)),.UNSPECIFIED.,.F.,.F.,.F.,(3,3),(2,2),(0.,1.),(0.,0.0249999999999999),
 .UNSPECIFIED.);
#886=B_SPLINE_SURFACE_WITH_KNOTS('',2,1,((#33121,#33122),(#33123,#33124),
(#33125,#33126)),.UNSPECIFIED.,.F.,.F.,.F.,(3,3),(2,2),(0.,1.),(0.,0.0249999999999999),
 .UNSPECIFIED.);
#887=B_SPLINE_SURFACE_WITH_KNOTS('',2,1,((#33132,#33133),(#33134,#33135),
(#33136,#33137)),.UNSPECIFIED.,.F.,.F.,.F.,(3,3),(2,2),(0.,1.),(0.,0.0249999999999999),
 .UNSPECIFIED.);
#888=B_SPLINE_SURFACE_WITH_KNOTS('',2,1,((#33143,#33144),(#33145,#33146),
(#33147,#33148)),.UNSPECIFIED.,.F.,.F.,.F.,(3,3),(2,2),(0.,1.),(0.,0.0249999999999999),
 .UNSPECIFIED.);
#889=B_SPLINE_SURFACE_WITH_KNOTS('',2,1,((#33154,#33155),(#33156,#33157),
(#33158,#33159)),.UNSPECIFIED.,.F.,.F.,.F.,(3,3),(2,2),(0.,1.),(0.,0.0249999999999999),
 .UNSPECIFIED.);
#890=B_SPLINE_SURFACE_WITH_KNOTS('',2,1,((#33165,#33166),(#33167,#33168),
(#33169,#33170)),.UNSPECIFIED.,.F.,.F.,.F.,(3,3),(2,2),(0.,1.),(0.,0.0249999999999999),
 .UNSPECIFIED.);
#891=B_SPLINE_SURFACE_WITH_KNOTS('',2,1,((#33176,#33177),(#33178,#33179),
(#33180,#33181)),.UNSPECIFIED.,.F.,.F.,.F.,(3,3),(2,2),(0.,1.),(0.,0.0249999999999999),
 .UNSPECIFIED.);
#892=B_SPLINE_SURFACE_WITH_KNOTS('',2,1,((#33191,#33192),(#33193,#33194),
(#33195,#33196)),.UNSPECIFIED.,.F.,.F.,.F.,(3,3),(2,2),(0.,1.),(0.,0.0249999999999999),
 .UNSPECIFIED.);
#893=B_SPLINE_SURFACE_WITH_KNOTS('',2,1,((#33202,#33203),(#33204,#33205),
(#33206,#33207)),.UNSPECIFIED.,.F.,.F.,.F.,(3,3),(2,2),(0.,1.),(0.,0.0249999999999999),
 .UNSPECIFIED.);
#894=B_SPLINE_SURFACE_WITH_KNOTS('',2,1,((#33213,#33214),(#33215,#33216),
(#33217,#33218)),.UNSPECIFIED.,.F.,.F.,.F.,(3,3),(2,2),(0.,1.),(0.,0.0249999999999999),
 .UNSPECIFIED.);
#895=B_SPLINE_SURFACE_WITH_KNOTS('',2,1,((#33224,#33225),(#33226,#33227),
(#33228,#33229)),.UNSPECIFIED.,.F.,.F.,.F.,(3,3),(2,2),(0.,1.),(0.,0.0249999999999999),
 .UNSPECIFIED.);
#896=B_SPLINE_SURFACE_WITH_KNOTS('',2,1,((#33235,#33236),(#33237,#33238),
(#33239,#33240)),.UNSPECIFIED.,.F.,.F.,.F.,(3,3),(2,2),(0.,1.),(0.,0.0249999999999999),
 .UNSPECIFIED.);
#897=B_SPLINE_SURFACE_WITH_KNOTS('',2,1,((#33246,#33247),(#33248,#33249),
(#33250,#33251)),.UNSPECIFIED.,.F.,.F.,.F.,(3,3),(2,2),(0.,1.),(0.,0.0249999999999999),
 .UNSPECIFIED.);
#898=B_SPLINE_SURFACE_WITH_KNOTS('',2,1,((#33257,#33258),(#33259,#33260),
(#33261,#33262)),.UNSPECIFIED.,.F.,.F.,.F.,(3,3),(2,2),(0.,1.),(0.,0.0249999999999999),
 .UNSPECIFIED.);
#899=B_SPLINE_SURFACE_WITH_KNOTS('',2,1,((#33268,#33269),(#33270,#33271),
(#33272,#33273)),.UNSPECIFIED.,.F.,.F.,.F.,(3,3),(2,2),(0.,1.),(0.,0.0249999999999999),
 .UNSPECIFIED.);
#900=B_SPLINE_SURFACE_WITH_KNOTS('',2,1,((#33279,#33280),(#33281,#33282),
(#33283,#33284)),.UNSPECIFIED.,.F.,.F.,.F.,(3,3),(2,2),(0.,1.),(0.,0.0249999999999999),
 .UNSPECIFIED.);
#901=B_SPLINE_SURFACE_WITH_KNOTS('',2,1,((#33290,#33291),(#33292,#33293),
(#33294,#33295)),.UNSPECIFIED.,.F.,.F.,.F.,(3,3),(2,2),(0.,1.),(0.,0.0249999999999999),
 .UNSPECIFIED.);
#902=B_SPLINE_SURFACE_WITH_KNOTS('',2,1,((#33301,#33302),(#33303,#33304),
(#33305,#33306)),.UNSPECIFIED.,.F.,.F.,.F.,(3,3),(2,2),(0.,1.),(0.,0.0249999999999999),
 .UNSPECIFIED.);
#903=B_SPLINE_SURFACE_WITH_KNOTS('',3,3,((#35349,#35350,#35351,#35352,#35353,
#35354,#35355,#35356,#35357,#35358,#35359,#35360,#35361,#35362,#35363,#35364,
#35365,#35366,#35367,#35368,#35369,#35370,#35371,#35372,#35373,#35374,#35375,
#35376,#35377,#35378,#35379,#35380,#35381,#35382,#35383,#35384,#35385,#35386,
#35387,#35388,#35389,#35390,#35391,#35392,#35393,#35394,#35395,#35396,#35397,
#35398,#35399,#35400,#35401,#35402,#35403,#35404,#35405,#35406,#35407,#35408,
#35409,#35410,#35411,#35412,#35413,#35414,#35415,#35416,#35417,#35418,#35419,
#35420,#35421,#35422,#35423,#35424,#35425,#35426,#35427,#35428,#35429,#35430,
#35431,#35432,#35433,#35434,#35435,#35436,#35437,#35438,#35439,#35440,#35441,
#35442,#35443,#35444,#35445,#35446,#35447,#35448,#35449,#35450,#35451,#35452,
#35453,#35454,#35455,#35456,#35457,#35458,#35459,#35460,#35461,#35462,#35463,
#35464,#35465,#35466,#35467,#35468,#35469,#35470,#35471,#35472,#35473,#35474,
#35475,#35476,#35477,#35478,#35479,#35480,#35481,#35482,#35483,#35484,#35485,
#35486,#35487,#35488,#35489,#35490,#35491,#35492,#35493,#35494,#35495,#35496,
#35497,#35498,#35499,#35500,#35501),(#35502,#35503,#35504,#35505,#35506,
#35507,#35508,#35509,#35510,#35511,#35512,#35513,#35514,#35515,#35516,#35517,
#35518,#35519,#35520,#35521,#35522,#35523,#35524,#35525,#35526,#35527,#35528,
#35529,#35530,#35531,#35532,#35533,#35534,#35535,#35536,#35537,#35538,#35539,
#35540,#35541,#35542,#35543,#35544,#35545,#35546,#35547,#35548,#35549,#35550,
#35551,#35552,#35553,#35554,#35555,#35556,#35557,#35558,#35559,#35560,#35561,
#35562,#35563,#35564,#35565,#35566,#35567,#35568,#35569,#35570,#35571,#35572,
#35573,#35574,#35575,#35576,#35577,#35578,#35579,#35580,#35581,#35582,#35583,
#35584,#35585,#35586,#35587,#35588,#35589,#35590,#35591,#35592,#35593,#35594,
#35595,#35596,#35597,#35598,#35599,#35600,#35601,#35602,#35603,#35604,#35605,
#35606,#35607,#35608,#35609,#35610,#35611,#35612,#35613,#35614,#35615,#35616,
#35617,#35618,#35619,#35620,#35621,#35622,#35623,#35624,#35625,#35626,#35627,
#35628,#35629,#35630,#35631,#35632,#35633,#35634,#35635,#35636,#35637,#35638,
#35639,#35640,#35641,#35642,#35643,#35644,#35645,#35646,#35647,#35648,#35649,
#35650,#35651,#35652,#35653,#35654),(#35655,#35656,#35657,#35658,#35659,
#35660,#35661,#35662,#35663,#35664,#35665,#35666,#35667,#35668,#35669,#35670,
#35671,#35672,#35673,#35674,#35675,#35676,#35677,#35678,#35679,#35680,#35681,
#35682,#35683,#35684,#35685,#35686,#35687,#35688,#35689,#35690,#35691,#35692,
#35693,#35694,#35695,#35696,#35697,#35698,#35699,#35700,#35701,#35702,#35703,
#35704,#35705,#35706,#35707,#35708,#35709,#35710,#35711,#35712,#35713,#35714,
#35715,#35716,#35717,#35718,#35719,#35720,#35721,#35722,#35723,#35724,#35725,
#35726,#35727,#35728,#35729,#35730,#35731,#35732,#35733,#35734,#35735,#35736,
#35737,#35738,#35739,#35740,#35741,#35742,#35743,#35744,#35745,#35746,#35747,
#35748,#35749,#35750,#35751,#35752,#35753,#35754,#35755,#35756,#35757,#35758,
#35759,#35760,#35761,#35762,#35763,#35764,#35765,#35766,#35767,#35768,#35769,
#35770,#35771,#35772,#35773,#35774,#35775,#35776,#35777,#35778,#35779,#35780,
#35781,#35782,#35783,#35784,#35785,#35786,#35787,#35788,#35789,#35790,#35791,
#35792,#35793,#35794,#35795,#35796,#35797,#35798,#35799,#35800,#35801,#35802,
#35803,#35804,#35805,#35806,#35807),(#35808,#35809,#35810,#35811,#35812,
#35813,#35814,#35815,#35816,#35817,#35818,#35819,#35820,#35821,#35822,#35823,
#35824,#35825,#35826,#35827,#35828,#35829,#35830,#35831,#35832,#35833,#35834,
#35835,#35836,#35837,#35838,#35839,#35840,#35841,#35842,#35843,#35844,#35845,
#35846,#35847,#35848,#35849,#35850,#35851,#35852,#35853,#35854,#35855,#35856,
#35857,#35858,#35859,#35860,#35861,#35862,#35863,#35864,#35865,#35866,#35867,
#35868,#35869,#35870,#35871,#35872,#35873,#35874,#35875,#35876,#35877,#35878,
#35879,#35880,#35881,#35882,#35883,#35884,#35885,#35886,#35887,#35888,#35889,
#35890,#35891,#35892,#35893,#35894,#35895,#35896,#35897,#35898,#35899,#35900,
#35901,#35902,#35903,#35904,#35905,#35906,#35907,#35908,#35909,#35910,#35911,
#35912,#35913,#35914,#35915,#35916,#35917,#35918,#35919,#35920,#35921,#35922,
#35923,#35924,#35925,#35926,#35927,#35928,#35929,#35930,#35931,#35932,#35933,
#35934,#35935,#35936,#35937,#35938,#35939,#35940,#35941,#35942,#35943,#35944,
#35945,#35946,#35947,#35948,#35949,#35950,#35951,#35952,#35953,#35954,#35955,
#35956,#35957,#35958,#35959,#35960)),.UNSPECIFIED.,.F.,.F.,.F.,(4,4),(4,
1,1,1,1,1,1,1,1,1,1,1,1,1,1,1,1,1,1,1,1,1,1,1,1,1,1,1,1,1,1,1,1,1,1,1,1,
1,1,1,1,1,1,1,1,1,1,1,1,1,1,1,1,1,1,1,1,1,1,1,1,1,1,1,1,1,1,1,1,1,1,1,1,
1,1,1,1,1,1,1,1,1,1,1,1,1,1,1,1,1,1,1,1,1,1,1,1,1,1,1,1,1,1,1,1,1,1,1,1,
1,1,1,1,1,1,1,1,1,1,1,1,1,1,1,1,1,1,1,1,1,1,1,1,1,1,1,1,1,1,1,1,1,1,1,1,
1,1,1,1,1,4),(0.,0.0991945497494695),(8.2986503954951,8.79490957269163,
9.29116874988815,9.78742792708467,10.2836871042812,10.7799462814777,11.2762054586742,
11.7724646358708,12.2687238130673,12.7649829902638,13.2612421674603,13.7575013446569,
14.2537605218534,14.7500196990499,15.2462788762464,15.742538053443,16.2387972306395,
16.735056407836,17.2313155850325,17.7275747622291,18.2238339394256,18.7200931166221,
19.2163522938186,19.7126114710152,20.2088706482117,20.7051298254082,21.2013890026047,
21.6976481798012,22.1939073569978,22.6901665341943,23.1864257113908,23.6826848885873,
24.1789440657839,24.6752032429804,25.1714624201769,25.6677215973734,26.16398077457,
26.6602399517665,27.156499128963,27.6527583061595,28.1490174833561,28.6452766605526,
29.1415358377491,29.6377950149456,30.1340541921422,30.6303133693387,31.1265725465352,
31.6228317237317,32.1190909009282,32.6153500781248,33.1116092553213,33.6078684325178,
34.1041276097143,34.6003867869109,35.0966459641074,35.5929051413039,36.0891643185004,
36.585423495697,37.0816826728935,37.57794185009,38.0742010272865,38.5704602044831,
39.0667193816796,39.5629785588761,40.0592377360726,40.5554969132692,41.0517560904657,
41.5480152676622,42.0442744448587,42.5405336220552,43.0367927992518,43.5330519764483,
44.0293111536448,44.5255703308413,45.0218295080379,45.5180886852344,46.0143478624309,
46.5106070396274,47.006866216824,47.5031253940205,47.999384571217,48.4956437484135,
48.9919029256101,49.4881621028066,49.9844212800031,50.4806804571996,50.9769396343962,
51.4731988115927,51.9694579887892,52.4657171659857,52.9619763431823,53.4582355203788,
53.9544946975753,54.4507538747718,54.9470130519683,55.4432722291649,55.9395314063614,
56.4357905835579,56.9320497607544,57.428308937951,57.9245681151475,58.420827292344,
58.9170864695405,59.4133456467371,59.9096048239336,60.4058640011301,60.9021231783266,
61.3983823555232,61.8946415327197,62.3909007099162,62.8871598871127,63.3834190643093,
63.8796782415058,64.3759374187023,64.8721965958988,65.3684557730953,65.8647149502919,
66.3609741274884,66.8572333046849,67.3534924818814,67.849751659078,68.3460108362745,
68.842270013471,69.3385291906675,69.8347883678641,70.3310475450606,70.8273067222571,
71.3235658994536,71.8198250766501,72.3160842538467,72.8123434310432,73.3086026082397,
73.8048617854362,74.3011209626328,74.7973801398293,75.2936393170258,75.7898984942223,
76.2861576714189,76.7824168486154,77.2786760258119,77.7749352030084,78.271194380205,
78.7674535574015,79.263712734598,79.7599719117945,80.2562310889911,80.7524902661876,
81.2487494433841,81.7450086205806,82.2412677977772,82.7375269749737),
 .UNSPECIFIED.);
#904=B_SPLINE_SURFACE_WITH_KNOTS('',3,3,((#36004,#36005,#36006,#36007,#36008,
#36009,#36010,#36011,#36012,#36013,#36014,#36015,#36016,#36017,#36018,#36019,
#36020,#36021,#36022,#36023,#36024,#36025,#36026,#36027,#36028,#36029,#36030,
#36031,#36032,#36033,#36034,#36035,#36036,#36037,#36038,#36039,#36040,#36041,
#36042,#36043,#36044,#36045,#36046,#36047,#36048,#36049,#36050,#36051,#36052,
#36053,#36054,#36055,#36056,#36057,#36058,#36059,#36060,#36061,#36062,#36063,
#36064,#36065,#36066,#36067,#36068,#36069,#36070,#36071,#36072,#36073,#36074,
#36075,#36076,#36077,#36078,#36079,#36080,#36081,#36082,#36083,#36084,#36085,
#36086,#36087,#36088,#36089,#36090,#36091,#36092,#36093,#36094,#36095,#36096,
#36097,#36098,#36099,#36100,#36101,#36102,#36103,#36104,#36105,#36106,#36107,
#36108,#36109,#36110,#36111,#36112,#36113,#36114,#36115,#36116,#36117,#36118,
#36119,#36120,#36121,#36122,#36123,#36124,#36125,#36126,#36127,#36128,#36129,
#36130,#36131,#36132,#36133,#36134,#36135,#36136,#36137,#36138,#36139,#36140,
#36141,#36142,#36143,#36144,#36145,#36146,#36147,#36148,#36149,#36150,#36151,
#36152,#36153,#36154,#36155,#36156),(#36157,#36158,#36159,#36160,#36161,
#36162,#36163,#36164,#36165,#36166,#36167,#36168,#36169,#36170,#36171,#36172,
#36173,#36174,#36175,#36176,#36177,#36178,#36179,#36180,#36181,#36182,#36183,
#36184,#36185,#36186,#36187,#36188,#36189,#36190,#36191,#36192,#36193,#36194,
#36195,#36196,#36197,#36198,#36199,#36200,#36201,#36202,#36203,#36204,#36205,
#36206,#36207,#36208,#36209,#36210,#36211,#36212,#36213,#36214,#36215,#36216,
#36217,#36218,#36219,#36220,#36221,#36222,#36223,#36224,#36225,#36226,#36227,
#36228,#36229,#36230,#36231,#36232,#36233,#36234,#36235,#36236,#36237,#36238,
#36239,#36240,#36241,#36242,#36243,#36244,#36245,#36246,#36247,#36248,#36249,
#36250,#36251,#36252,#36253,#36254,#36255,#36256,#36257,#36258,#36259,#36260,
#36261,#36262,#36263,#36264,#36265,#36266,#36267,#36268,#36269,#36270,#36271,
#36272,#36273,#36274,#36275,#36276,#36277,#36278,#36279,#36280,#36281,#36282,
#36283,#36284,#36285,#36286,#36287,#36288,#36289,#36290,#36291,#36292,#36293,
#36294,#36295,#36296,#36297,#36298,#36299,#36300,#36301,#36302,#36303,#36304,
#36305,#36306,#36307,#36308,#36309),(#36310,#36311,#36312,#36313,#36314,
#36315,#36316,#36317,#36318,#36319,#36320,#36321,#36322,#36323,#36324,#36325,
#36326,#36327,#36328,#36329,#36330,#36331,#36332,#36333,#36334,#36335,#36336,
#36337,#36338,#36339,#36340,#36341,#36342,#36343,#36344,#36345,#36346,#36347,
#36348,#36349,#36350,#36351,#36352,#36353,#36354,#36355,#36356,#36357,#36358,
#36359,#36360,#36361,#36362,#36363,#36364,#36365,#36366,#36367,#36368,#36369,
#36370,#36371,#36372,#36373,#36374,#36375,#36376,#36377,#36378,#36379,#36380,
#36381,#36382,#36383,#36384,#36385,#36386,#36387,#36388,#36389,#36390,#36391,
#36392,#36393,#36394,#36395,#36396,#36397,#36398,#36399,#36400,#36401,#36402,
#36403,#36404,#36405,#36406,#36407,#36408,#36409,#36410,#36411,#36412,#36413,
#36414,#36415,#36416,#36417,#36418,#36419,#36420,#36421,#36422,#36423,#36424,
#36425,#36426,#36427,#36428,#36429,#36430,#36431,#36432,#36433,#36434,#36435,
#36436,#36437,#36438,#36439,#36440,#36441,#36442,#36443,#36444,#36445,#36446,
#36447,#36448,#36449,#36450,#36451,#36452,#36453,#36454,#36455,#36456,#36457,
#36458,#36459,#36460,#36461,#36462),(#36463,#36464,#36465,#36466,#36467,
#36468,#36469,#36470,#36471,#36472,#36473,#36474,#36475,#36476,#36477,#36478,
#36479,#36480,#36481,#36482,#36483,#36484,#36485,#36486,#36487,#36488,#36489,
#36490,#36491,#36492,#36493,#36494,#36495,#36496,#36497,#36498,#36499,#36500,
#36501,#36502,#36503,#36504,#36505,#36506,#36507,#36508,#36509,#36510,#36511,
#36512,#36513,#36514,#36515,#36516,#36517,#36518,#36519,#36520,#36521,#36522,
#36523,#36524,#36525,#36526,#36527,#36528,#36529,#36530,#36531,#36532,#36533,
#36534,#36535,#36536,#36537,#36538,#36539,#36540,#36541,#36542,#36543,#36544,
#36545,#36546,#36547,#36548,#36549,#36550,#36551,#36552,#36553,#36554,#36555,
#36556,#36557,#36558,#36559,#36560,#36561,#36562,#36563,#36564,#36565,#36566,
#36567,#36568,#36569,#36570,#36571,#36572,#36573,#36574,#36575,#36576,#36577,
#36578,#36579,#36580,#36581,#36582,#36583,#36584,#36585,#36586,#36587,#36588,
#36589,#36590,#36591,#36592,#36593,#36594,#36595,#36596,#36597,#36598,#36599,
#36600,#36601,#36602,#36603,#36604,#36605,#36606,#36607,#36608,#36609,#36610,
#36611,#36612,#36613,#36614,#36615)),.UNSPECIFIED.,.F.,.F.,.F.,(4,4),(4,
1,1,1,1,1,1,1,1,1,1,1,1,1,1,1,1,1,1,1,1,1,1,1,1,1,1,1,1,1,1,1,1,1,1,1,1,
1,1,1,1,1,1,1,1,1,1,1,1,1,1,1,1,1,1,1,1,1,1,1,1,1,1,1,1,1,1,1,1,1,1,1,1,
1,1,1,1,1,1,1,1,1,1,1,1,1,1,1,1,1,1,1,1,1,1,1,1,1,1,1,1,1,1,1,1,1,1,1,1,
1,1,1,1,1,1,1,1,1,1,1,1,1,1,1,1,1,1,1,1,1,1,1,1,1,1,1,1,1,1,1,1,1,1,1,1,
1,1,1,1,1,4),(0.,0.0991945497494695),(11.6149723878393,12.1112315650359,
12.6074907422324,13.1037499194289,13.6000090966254,14.096268273822,14.5925274510185,
15.088786628215,15.5850458054115,16.0813049826081,16.5775641598046,17.0738233370011,
17.5700825141976,18.0663416913942,18.5626008685907,19.0588600457872,19.5551192229837,
20.0513784001803,20.5476375773768,21.0438967545733,21.5401559317698,22.0364151089663,
22.5326742861629,23.0289334633594,23.5251926405559,24.0214518177524,24.517710994949,
25.0139701721455,25.510229349342,26.0064885265385,26.5027477037351,26.9990068809316,
27.4952660581281,27.9915252353246,28.4877844125212,28.9840435897177,29.4803027669142,
29.9765619441107,30.4728211213073,30.9690802985038,31.4653394757003,31.9615986528968,
32.4578578300934,32.9541170072899,33.4503761844864,33.9466353616829,34.4428945388795,
34.939153716076,35.4354128932725,35.931672070469,36.4279312476656,36.9241904248621,
37.4204496020586,37.9167087792551,38.4129679564517,38.9092271336482,39.4054863108447,
39.9017454880412,40.3980046652377,40.8942638424343,41.3905230196308,41.8867821968273,
42.3830413740238,42.8793005512204,43.3755597284169,43.8718189056134,44.36807808281,
44.8643372600065,45.360596437203,45.8568556143995,46.353114791596,46.8493739687926,
47.3456331459891,47.8418923231856,48.3381515003821,48.8344106775787,49.3306698547752,
49.8269290319717,50.3231882091682,50.8194473863648,51.3157065635613,51.8119657407578,
52.3082249179543,52.8044840951509,53.3007432723474,53.7970024495439,54.2932616267404,
54.789520803937,55.2857799811335,55.78203915833,56.2782983355265,56.7745575127231,
57.2708166899196,57.7670758671161,58.2633350443126,58.7595942215092,59.2558533987057,
59.7521125759022,60.2483717530987,60.7446309302953,61.2408901074918,61.7371492846883,
62.2334084618848,62.7296676390814,63.2259268162779,63.7221859934744,64.2184451706709,
64.7147043478674,65.210963525064,65.7072227022605,66.203481879457,66.6997410566536,
67.1960002338501,67.6922594110466,68.1885185882431,68.6847777654396,69.1810369426362,
69.6772961198327,70.1735552970292,70.6698144742257,71.1660736514223,71.6623328286188,
72.1585920058153,72.6548511830118,73.1511103602084,73.6473695374049,74.1436287146014,
74.6398878917979,75.1361470689945,75.632406246191,76.1286654233875,76.624924600584,
77.1211837777806,77.6174429549771,78.1137021321736,78.6099613093701,79.1062204865667,
79.6024796637632,80.0987388409597,80.5949980181562,81.0912571953528,81.5875163725493,
82.0837755497458,82.5800347269423,83.0762939041389,83.5725530813354,84.0688122585319,
84.5650714357284,85.061330612925,85.5575897901215,86.053848967318),
 .UNSPECIFIED.);
#905=B_SPLINE_SURFACE_WITH_KNOTS('',3,3,((#38452,#38453,#38454,#38455,#38456,
#38457,#38458,#38459,#38460,#38461,#38462,#38463,#38464,#38465,#38466,#38467,
#38468,#38469,#38470,#38471,#38472,#38473,#38474,#38475,#38476,#38477,#38478,
#38479,#38480,#38481,#38482,#38483,#38484,#38485,#38486,#38487,#38488,#38489,
#38490,#38491,#38492,#38493,#38494,#38495,#38496,#38497,#38498,#38499,#38500,
#38501,#38502,#38503,#38504,#38505,#38506,#38507,#38508,#38509,#38510,#38511,
#38512,#38513,#38514,#38515,#38516,#38517,#38518,#38519,#38520,#38521,#38522,
#38523,#38524,#38525,#38526,#38527,#38528,#38529,#38530,#38531,#38532,#38533,
#38534,#38535,#38536,#38537,#38538,#38539,#38540,#38541,#38542,#38543,#38544,
#38545,#38546,#38547,#38548,#38549,#38550,#38551,#38552,#38553,#38554,#38555,
#38556,#38557,#38558,#38559,#38560,#38561,#38562,#38563,#38564,#38565,#38566,
#38567,#38568,#38569,#38570,#38571,#38572,#38573,#38574,#38575,#38576,#38577,
#38578,#38579,#38580,#38581,#38582,#38583,#38584,#38585,#38586,#38587,#38588,
#38589,#38590,#38591,#38592,#38593,#38594,#38595,#38596,#38597,#38598,#38599,
#38600,#38601,#38602,#38603,#38604,#38605,#38606,#38607,#38608,#38609,#38610,
#38611,#38612,#38613,#38614,#38615,#38616,#38617,#38618),(#38619,#38620,
#38621,#38622,#38623,#38624,#38625,#38626,#38627,#38628,#38629,#38630,#38631,
#38632,#38633,#38634,#38635,#38636,#38637,#38638,#38639,#38640,#38641,#38642,
#38643,#38644,#38645,#38646,#38647,#38648,#38649,#38650,#38651,#38652,#38653,
#38654,#38655,#38656,#38657,#38658,#38659,#38660,#38661,#38662,#38663,#38664,
#38665,#38666,#38667,#38668,#38669,#38670,#38671,#38672,#38673,#38674,#38675,
#38676,#38677,#38678,#38679,#38680,#38681,#38682,#38683,#38684,#38685,#38686,
#38687,#38688,#38689,#38690,#38691,#38692,#38693,#38694,#38695,#38696,#38697,
#38698,#38699,#38700,#38701,#38702,#38703,#38704,#38705,#38706,#38707,#38708,
#38709,#38710,#38711,#38712,#38713,#38714,#38715,#38716,#38717,#38718,#38719,
#38720,#38721,#38722,#38723,#38724,#38725,#38726,#38727,#38728,#38729,#38730,
#38731,#38732,#38733,#38734,#38735,#38736,#38737,#38738,#38739,#38740,#38741,
#38742,#38743,#38744,#38745,#38746,#38747,#38748,#38749,#38750,#38751,#38752,
#38753,#38754,#38755,#38756,#38757,#38758,#38759,#38760,#38761,#38762,#38763,
#38764,#38765,#38766,#38767,#38768,#38769,#38770,#38771,#38772,#38773,#38774,
#38775,#38776,#38777,#38778,#38779,#38780,#38781,#38782,#38783,#38784,#38785),
(#38786,#38787,#38788,#38789,#38790,#38791,#38792,#38793,#38794,#38795,
#38796,#38797,#38798,#38799,#38800,#38801,#38802,#38803,#38804,#38805,#38806,
#38807,#38808,#38809,#38810,#38811,#38812,#38813,#38814,#38815,#38816,#38817,
#38818,#38819,#38820,#38821,#38822,#38823,#38824,#38825,#38826,#38827,#38828,
#38829,#38830,#38831,#38832,#38833,#38834,#38835,#38836,#38837,#38838,#38839,
#38840,#38841,#38842,#38843,#38844,#38845,#38846,#38847,#38848,#38849,#38850,
#38851,#38852,#38853,#38854,#38855,#38856,#38857,#38858,#38859,#38860,#38861,
#38862,#38863,#38864,#38865,#38866,#38867,#38868,#38869,#38870,#38871,#38872,
#38873,#38874,#38875,#38876,#38877,#38878,#38879,#38880,#38881,#38882,#38883,
#38884,#38885,#38886,#38887,#38888,#38889,#38890,#38891,#38892,#38893,#38894,
#38895,#38896,#38897,#38898,#38899,#38900,#38901,#38902,#38903,#38904,#38905,
#38906,#38907,#38908,#38909,#38910,#38911,#38912,#38913,#38914,#38915,#38916,
#38917,#38918,#38919,#38920,#38921,#38922,#38923,#38924,#38925,#38926,#38927,
#38928,#38929,#38930,#38931,#38932,#38933,#38934,#38935,#38936,#38937,#38938,
#38939,#38940,#38941,#38942,#38943,#38944,#38945,#38946,#38947,#38948,#38949,
#38950,#38951,#38952),(#38953,#38954,#38955,#38956,#38957,#38958,#38959,
#38960,#38961,#38962,#38963,#38964,#38965,#38966,#38967,#38968,#38969,#38970,
#38971,#38972,#38973,#38974,#38975,#38976,#38977,#38978,#38979,#38980,#38981,
#38982,#38983,#38984,#38985,#38986,#38987,#38988,#38989,#38990,#38991,#38992,
#38993,#38994,#38995,#38996,#38997,#38998,#38999,#39000,#39001,#39002,#39003,
#39004,#39005,#39006,#39007,#39008,#39009,#39010,#39011,#39012,#39013,#39014,
#39015,#39016,#39017,#39018,#39019,#39020,#39021,#39022,#39023,#39024,#39025,
#39026,#39027,#39028,#39029,#39030,#39031,#39032,#39033,#39034,#39035,#39036,
#39037,#39038,#39039,#39040,#39041,#39042,#39043,#39044,#39045,#39046,#39047,
#39048,#39049,#39050,#39051,#39052,#39053,#39054,#39055,#39056,#39057,#39058,
#39059,#39060,#39061,#39062,#39063,#39064,#39065,#39066,#39067,#39068,#39069,
#39070,#39071,#39072,#39073,#39074,#39075,#39076,#39077,#39078,#39079,#39080,
#39081,#39082,#39083,#39084,#39085,#39086,#39087,#39088,#39089,#39090,#39091,
#39092,#39093,#39094,#39095,#39096,#39097,#39098,#39099,#39100,#39101,#39102,
#39103,#39104,#39105,#39106,#39107,#39108,#39109,#39110,#39111,#39112,#39113,
#39114,#39115,#39116,#39117,#39118,#39119)),.UNSPECIFIED.,.F.,.F.,.F.,(4,
4),(4,1,1,1,1,1,1,1,1,1,1,1,1,1,1,1,1,1,1,1,1,1,1,1,1,1,1,1,1,1,1,1,1,1,
1,1,1,1,1,1,1,1,1,1,1,1,1,1,1,1,1,1,1,1,1,1,1,1,1,1,1,1,1,1,1,1,1,1,1,1,
1,1,1,1,1,1,1,1,1,1,1,1,1,1,1,1,1,1,1,1,1,1,1,1,1,1,1,1,1,1,1,1,1,1,1,1,
1,1,1,1,1,1,1,1,1,1,1,1,1,1,1,1,1,1,1,1,1,1,1,1,1,1,1,1,1,1,1,1,1,1,1,1,
1,1,1,1,1,1,1,1,1,1,1,1,1,1,1,1,1,1,1,1,1,1,4),(0.,0.0658179306876167),
(8.30838445208293,8.80594720143358,9.30350995078422,9.80107270013487,10.2986354494855,
10.7961981988362,11.2937609481868,11.7913236975375,12.2888864468881,12.7864491962387,
13.2840119455894,13.78157469494,14.2791374442907,14.7767001936413,15.274262942992,
15.7718256923426,16.2693884416933,16.7669511910439,17.2645139403946,17.7620766897452,
18.2596394390959,18.7572021884465,19.2547649377972,19.7523276871478,20.2498904364984,
20.7474531858491,21.2450159351997,21.7425786845504,22.240141433901,22.7377041832517,
23.2352669326023,23.732829681953,24.2303924313036,24.7279551806543,25.2255179300049,
25.7230806793556,26.2206434287062,26.7182061780569,27.2157689274075,27.7133316767581,
28.2108944261088,28.7084571754594,29.2060199248101,29.7035826741607,30.2011454235114,
30.698708172862,31.1962709222127,31.6938336715633,32.191396420914,32.6889591702646,
33.1865219196153,33.6840846689659,34.1816474183166,34.6792101676672,35.1767729170178,
35.6743356663685,36.1718984157191,36.6694611650698,37.1670239144204,37.6645866637711,
38.1621494131217,38.6597121624724,39.157274911823,39.6548376611737,40.1524004105243,
40.649963159875,41.1475259092256,41.6450886585762,42.1426514079269,42.6402141572775,
43.1377769066282,43.6353396559788,44.1329024053295,44.6304651546801,45.1280279040308,
45.6255906533814,46.1231534027321,46.6207161520827,47.1182789014334,47.615841650784,
48.1134044001347,48.6109671494853,49.108529898836,49.6060926481866,50.1036553975372,
50.6012181468879,51.0987808962385,51.5963436455892,52.0939063949398,52.5914691442905,
53.0890318936411,53.5865946429918,54.0841573923424,54.5817201416931,55.0792828910437,
55.5768456403944,56.074408389745,56.5719711390957,57.0695338884463,57.5670966377969,
58.0646593871476,58.5622221364982,59.0597848858489,59.5573476351995,60.0549103845502,
60.5524731339008,61.0500358832515,61.5475986326021,62.0451613819528,62.5427241313034,
63.0402868806541,63.5378496300047,64.0354123793553,64.532975128706,65.0305378780566,
65.5281006274073,66.0256633767579,66.5232261261086,67.0207888754592,67.5183516248099,
68.0159143741605,68.5134771235112,69.0110398728618,69.5086026222125,70.0061653715631,
70.5037281209138,71.0012908702644,71.498853619615,71.9964163689657,72.4939791183163,
72.991541867667,73.4891046170176,73.9866673663683,74.4842301157189,74.9817928650696,
75.4793556144202,75.9769183637709,76.4744811131215,76.9720438624722,77.4696066118228,
77.9671693611735,78.4647321105241,78.9622948598747,79.4598576092254,79.957420358576,
80.4549831079267,80.9525458572773,81.450108606628,81.9476713559786,82.4452341053293,
82.9427968546799,83.4403596040306,83.9379223533812,84.4354851027319,84.9330478520825,
85.4306106014332,85.9281733507838,86.4257361001345,86.9232988494851,87.4208615988357,
87.9184243481864,88.415987097537,88.9135498468877,89.4111125962383,89.908675345589),
 .UNSPECIFIED.);
#906=B_SPLINE_SURFACE_WITH_KNOTS('',3,3,((#39480,#39481,#39482,#39483,#39484,
#39485,#39486,#39487,#39488,#39489,#39490,#39491,#39492,#39493,#39494,#39495,
#39496,#39497,#39498,#39499,#39500,#39501,#39502,#39503,#39504,#39505,#39506,
#39507,#39508,#39509,#39510,#39511,#39512,#39513,#39514,#39515,#39516,#39517,
#39518,#39519,#39520,#39521,#39522,#39523,#39524,#39525,#39526,#39527,#39528,
#39529,#39530,#39531,#39532,#39533,#39534,#39535,#39536,#39537,#39538,#39539,
#39540,#39541,#39542,#39543,#39544,#39545,#39546,#39547,#39548,#39549,#39550,
#39551,#39552,#39553,#39554,#39555,#39556,#39557,#39558,#39559,#39560,#39561,
#39562,#39563,#39564,#39565,#39566,#39567,#39568,#39569,#39570,#39571,#39572,
#39573,#39574,#39575,#39576,#39577,#39578,#39579,#39580,#39581,#39582,#39583,
#39584,#39585,#39586,#39587,#39588,#39589,#39590,#39591,#39592,#39593,#39594,
#39595,#39596,#39597,#39598,#39599,#39600,#39601,#39602,#39603,#39604,#39605,
#39606,#39607,#39608,#39609,#39610,#39611,#39612,#39613,#39614,#39615,#39616,
#39617,#39618,#39619,#39620,#39621,#39622,#39623,#39624,#39625,#39626,#39627,
#39628,#39629,#39630,#39631,#39632,#39633,#39634,#39635,#39636,#39637,#39638,
#39639,#39640,#39641,#39642,#39643,#39644,#39645,#39646),(#39647,#39648,
#39649,#39650,#39651,#39652,#39653,#39654,#39655,#39656,#39657,#39658,#39659,
#39660,#39661,#39662,#39663,#39664,#39665,#39666,#39667,#39668,#39669,#39670,
#39671,#39672,#39673,#39674,#39675,#39676,#39677,#39678,#39679,#39680,#39681,
#39682,#39683,#39684,#39685,#39686,#39687,#39688,#39689,#39690,#39691,#39692,
#39693,#39694,#39695,#39696,#39697,#39698,#39699,#39700,#39701,#39702,#39703,
#39704,#39705,#39706,#39707,#39708,#39709,#39710,#39711,#39712,#39713,#39714,
#39715,#39716,#39717,#39718,#39719,#39720,#39721,#39722,#39723,#39724,#39725,
#39726,#39727,#39728,#39729,#39730,#39731,#39732,#39733,#39734,#39735,#39736,
#39737,#39738,#39739,#39740,#39741,#39742,#39743,#39744,#39745,#39746,#39747,
#39748,#39749,#39750,#39751,#39752,#39753,#39754,#39755,#39756,#39757,#39758,
#39759,#39760,#39761,#39762,#39763,#39764,#39765,#39766,#39767,#39768,#39769,
#39770,#39771,#39772,#39773,#39774,#39775,#39776,#39777,#39778,#39779,#39780,
#39781,#39782,#39783,#39784,#39785,#39786,#39787,#39788,#39789,#39790,#39791,
#39792,#39793,#39794,#39795,#39796,#39797,#39798,#39799,#39800,#39801,#39802,
#39803,#39804,#39805,#39806,#39807,#39808,#39809,#39810,#39811,#39812,#39813),
(#39814,#39815,#39816,#39817,#39818,#39819,#39820,#39821,#39822,#39823,
#39824,#39825,#39826,#39827,#39828,#39829,#39830,#39831,#39832,#39833,#39834,
#39835,#39836,#39837,#39838,#39839,#39840,#39841,#39842,#39843,#39844,#39845,
#39846,#39847,#39848,#39849,#39850,#39851,#39852,#39853,#39854,#39855,#39856,
#39857,#39858,#39859,#39860,#39861,#39862,#39863,#39864,#39865,#39866,#39867,
#39868,#39869,#39870,#39871,#39872,#39873,#39874,#39875,#39876,#39877,#39878,
#39879,#39880,#39881,#39882,#39883,#39884,#39885,#39886,#39887,#39888,#39889,
#39890,#39891,#39892,#39893,#39894,#39895,#39896,#39897,#39898,#39899,#39900,
#39901,#39902,#39903,#39904,#39905,#39906,#39907,#39908,#39909,#39910,#39911,
#39912,#39913,#39914,#39915,#39916,#39917,#39918,#39919,#39920,#39921,#39922,
#39923,#39924,#39925,#39926,#39927,#39928,#39929,#39930,#39931,#39932,#39933,
#39934,#39935,#39936,#39937,#39938,#39939,#39940,#39941,#39942,#39943,#39944,
#39945,#39946,#39947,#39948,#39949,#39950,#39951,#39952,#39953,#39954,#39955,
#39956,#39957,#39958,#39959,#39960,#39961,#39962,#39963,#39964,#39965,#39966,
#39967,#39968,#39969,#39970,#39971,#39972,#39973,#39974,#39975,#39976,#39977,
#39978,#39979,#39980),(#39981,#39982,#39983,#39984,#39985,#39986,#39987,
#39988,#39989,#39990,#39991,#39992,#39993,#39994,#39995,#39996,#39997,#39998,
#39999,#40000,#40001,#40002,#40003,#40004,#40005,#40006,#40007,#40008,#40009,
#40010,#40011,#40012,#40013,#40014,#40015,#40016,#40017,#40018,#40019,#40020,
#40021,#40022,#40023,#40024,#40025,#40026,#40027,#40028,#40029,#40030,#40031,
#40032,#40033,#40034,#40035,#40036,#40037,#40038,#40039,#40040,#40041,#40042,
#40043,#40044,#40045,#40046,#40047,#40048,#40049,#40050,#40051,#40052,#40053,
#40054,#40055,#40056,#40057,#40058,#40059,#40060,#40061,#40062,#40063,#40064,
#40065,#40066,#40067,#40068,#40069,#40070,#40071,#40072,#40073,#40074,#40075,
#40076,#40077,#40078,#40079,#40080,#40081,#40082,#40083,#40084,#40085,#40086,
#40087,#40088,#40089,#40090,#40091,#40092,#40093,#40094,#40095,#40096,#40097,
#40098,#40099,#40100,#40101,#40102,#40103,#40104,#40105,#40106,#40107,#40108,
#40109,#40110,#40111,#40112,#40113,#40114,#40115,#40116,#40117,#40118,#40119,
#40120,#40121,#40122,#40123,#40124,#40125,#40126,#40127,#40128,#40129,#40130,
#40131,#40132,#40133,#40134,#40135,#40136,#40137,#40138,#40139,#40140,#40141,
#40142,#40143,#40144,#40145,#40146,#40147)),.UNSPECIFIED.,.F.,.F.,.F.,(4,
4),(4,1,1,1,1,1,1,1,1,1,1,1,1,1,1,1,1,1,1,1,1,1,1,1,1,1,1,1,1,1,1,1,1,1,
1,1,1,1,1,1,1,1,1,1,1,1,1,1,1,1,1,1,1,1,1,1,1,1,1,1,1,1,1,1,1,1,1,1,1,1,
1,1,1,1,1,1,1,1,1,1,1,1,1,1,1,1,1,1,1,1,1,1,1,1,1,1,1,1,1,1,1,1,1,1,1,1,
1,1,1,1,1,1,1,1,1,1,1,1,1,1,1,1,1,1,1,1,1,1,1,1,1,1,1,1,1,1,1,1,1,1,1,1,
1,1,1,1,1,1,1,1,1,1,1,1,1,1,1,1,1,1,1,1,1,1,4),(0.,0.0658179306876167),
(11.6150328478181,12.1125955971687,12.6101583465194,13.10772109587,13.6052838452207,
14.1028465945713,14.600409343922,15.0979720932726,15.5955348426233,16.0930975919739,
16.5906603413246,17.0882230906752,17.5857858400259,18.0833485893765,18.5809113387272,
19.0784740880778,19.5760368374285,20.0735995867791,20.5711623361297,21.0687250854804,
21.566287834831,22.0638505841817,22.5614133335323,23.058976082883,23.5565388322336,
24.0541015815843,24.5516643309349,25.0492270802856,25.5467898296362,26.0443525789869,
26.5419153283375,27.0394780776882,27.5370408270388,28.0346035763895,28.5321663257401,
29.0297290750907,29.5272918244414,30.024854573792,30.5224173231427,31.0199800724933,
31.517542821844,32.0151055711946,32.5126683205453,33.0102310698959,33.5077938192466,
34.0053565685972,34.5029193179479,35.0004820672985,35.4980448166492,35.9956075659998,
36.4931703153505,36.9907330647011,37.4882958140517,37.9858585634024,38.483421312753,
38.9809840621037,39.4785468114543,39.976109560805,40.4736723101556,40.9712350595063,
41.4687978088569,41.9663605582076,42.4639233075582,42.9614860569089,43.4590488062595,
43.9566115556102,44.4541743049608,44.9517370543115,45.4492998036621,45.9468625530127,
46.4444253023634,46.941988051714,47.4395508010647,47.9371135504153,48.434676299766,
48.9322390491166,49.4298017984673,49.9273645478179,50.4249272971686,50.9224900465192,
51.4200527958699,51.9176155452205,52.4151782945712,52.9127410439218,53.4103037932725,
53.9078665426231,54.4054292919737,54.9029920413244,55.400554790675,55.8981175400257,
56.3956802893763,56.893243038727,57.3908057880776,57.8883685374283,58.3859312867789,
58.8834940361296,59.3810567854802,59.8786195348309,60.3761822841815,60.8737450335322,
61.3713077828828,61.8688705322335,62.3664332815841,62.8639960309348,63.3615587802854,
63.859121529636,64.3566842789867,64.8542470283373,65.351809777688,65.8493725270386,
66.3469352763893,66.8444980257399,67.3420607750906,67.8396235244412,68.3371862737919,
68.8347490231425,69.3323117724932,69.8298745218438,70.3274372711945,70.8250000205451,
71.3225627698958,71.8201255192464,72.317688268597,72.8152510179477,73.3128137672983,
73.810376516649,74.3079392659996,74.8055020153503,75.3030647647009,75.8006275140516,
76.2981902634022,76.7957530127529,77.2933157621035,77.7908785114542,78.2884412608048,
78.7860040101555,79.2835667595061,79.7811295088568,80.2786922582074,80.776255007558,
81.2738177569087,81.7713805062593,82.26894325561,82.7665060049606,83.2640687543113,
83.7616315036619,84.2591942530126,84.7567570023632,85.2543197517139,85.7518825010645,
86.2494452504152,86.7470079997658,87.2445707491165,87.7421334984671,88.2396962478177,
88.7372589971684,89.234821746519,89.7323844958697,90.2299472452203,90.727509994571,
91.2250727439216,91.7226354932723,92.2201982426229,92.7177609919736,93.2153237413242),
 .UNSPECIFIED.);
#907=B_SPLINE_SURFACE_WITH_KNOTS('',3,3,((#41556,#41557,#41558,#41559,#41560,
#41561,#41562,#41563,#41564,#41565,#41566,#41567,#41568,#41569,#41570,#41571,
#41572,#41573,#41574,#41575,#41576,#41577,#41578,#41579,#41580,#41581,#41582,
#41583,#41584,#41585,#41586,#41587,#41588,#41589,#41590,#41591,#41592,#41593,
#41594,#41595,#41596,#41597,#41598,#41599,#41600,#41601,#41602,#41603,#41604,
#41605,#41606,#41607,#41608,#41609,#41610,#41611,#41612,#41613,#41614,#41615,
#41616,#41617,#41618,#41619,#41620,#41621,#41622,#41623,#41624,#41625,#41626,
#41627,#41628,#41629,#41630,#41631,#41632,#41633,#41634,#41635,#41636,#41637,
#41638,#41639,#41640,#41641),(#41642,#41643,#41644,#41645,#41646,#41647,
#41648,#41649,#41650,#41651,#41652,#41653,#41654,#41655,#41656,#41657,#41658,
#41659,#41660,#41661,#41662,#41663,#41664,#41665,#41666,#41667,#41668,#41669,
#41670,#41671,#41672,#41673,#41674,#41675,#41676,#41677,#41678,#41679,#41680,
#41681,#41682,#41683,#41684,#41685,#41686,#41687,#41688,#41689,#41690,#41691,
#41692,#41693,#41694,#41695,#41696,#41697,#41698,#41699,#41700,#41701,#41702,
#41703,#41704,#41705,#41706,#41707,#41708,#41709,#41710,#41711,#41712,#41713,
#41714,#41715,#41716,#41717,#41718,#41719,#41720,#41721,#41722,#41723,#41724,
#41725,#41726,#41727),(#41728,#41729,#41730,#41731,#41732,#41733,#41734,
#41735,#41736,#41737,#41738,#41739,#41740,#41741,#41742,#41743,#41744,#41745,
#41746,#41747,#41748,#41749,#41750,#41751,#41752,#41753,#41754,#41755,#41756,
#41757,#41758,#41759,#41760,#41761,#41762,#41763,#41764,#41765,#41766,#41767,
#41768,#41769,#41770,#41771,#41772,#41773,#41774,#41775,#41776,#41777,#41778,
#41779,#41780,#41781,#41782,#41783,#41784,#41785,#41786,#41787,#41788,#41789,
#41790,#41791,#41792,#41793,#41794,#41795,#41796,#41797,#41798,#41799,#41800,
#41801,#41802,#41803,#41804,#41805,#41806,#41807,#41808,#41809,#41810,#41811,
#41812,#41813),(#41814,#41815,#41816,#41817,#41818,#41819,#41820,#41821,
#41822,#41823,#41824,#41825,#41826,#41827,#41828,#41829,#41830,#41831,#41832,
#41833,#41834,#41835,#41836,#41837,#41838,#41839,#41840,#41841,#41842,#41843,
#41844,#41845,#41846,#41847,#41848,#41849,#41850,#41851,#41852,#41853,#41854,
#41855,#41856,#41857,#41858,#41859,#41860,#41861,#41862,#41863,#41864,#41865,
#41866,#41867,#41868,#41869,#41870,#41871,#41872,#41873,#41874,#41875,#41876,
#41877,#41878,#41879,#41880,#41881,#41882,#41883,#41884,#41885,#41886,#41887,
#41888,#41889,#41890,#41891,#41892,#41893,#41894,#41895,#41896,#41897,#41898,
#41899)),.UNSPECIFIED.,.F.,.F.,.F.,(4,4),(4,1,1,1,1,1,1,1,1,1,1,1,1,1,1,
1,1,1,1,1,1,1,1,1,1,1,1,1,1,1,1,1,1,1,1,1,1,1,1,1,1,1,1,1,1,1,1,1,1,1,1,
1,1,1,1,1,1,1,1,1,1,1,1,1,1,1,1,1,1,1,1,1,1,1,1,1,1,1,1,1,1,1,1,4),(0.,
0.0658179306876173),(8.30838445208316,8.80821144197691,9.30803843187066,
10.3076924116582,11.3073463914457,12.3070003712332,13.3066543510207,14.3063083308082,
15.3059623105957,16.3056162903832,17.3052702701707,18.3049242499582,19.3045782297458,
20.3042322095333,21.3038861893208,22.3035401691083,23.3031941488958,24.3028481286833,
25.3025021084708,26.3021560882583,27.3018100680458,28.3014640478333,29.3011180276209,
30.3007720074084,31.3004259871959,32.3000799669834,33.2997339467709,34.2993879265584,
35.2990419063459,36.2986958861334,37.2983498659209,38.2980038457084,39.2976578254959,
40.2973118052834,41.296965785071,42.2966197648585,43.296273744646,44.2959277244335,
45.295581704221,46.2952356840085,47.294889663796,48.2945436435835,49.294197623371,
50.2938516031585,51.2935055829461,52.2931595627336,53.2928135425211,54.2924675223086,
55.2921215020961,56.2917754818836,57.2914294616711,58.2910834414586,59.2907374212461,
60.2903914010336,61.2900453808211,62.2896993606087,63.2893533403962,64.2890073201837,
65.2886612999712,66.2883152797587,67.2879692595462,68.2876232393337,69.2872772191212,
70.2869311989087,71.2865851786962,72.2862391584838,73.2858931382713,74.2855471180588,
75.2852010978463,76.2848550776338,77.2845090574213,78.2841630372088,79.2838170169963,
80.2834709967838,81.2831249765713,82.2827789563588,83.2824329361463,84.2820869159339,
85.2817408957214,86.2813948755089,87.2810488552964,88.2807028350839,88.7805298249777,
89.2803568148714),.UNSPECIFIED.);
#908=B_SPLINE_SURFACE_WITH_KNOTS('',3,3,((#42261,#42262,#42263,#42264,#42265,
#42266,#42267,#42268,#42269,#42270,#42271,#42272,#42273,#42274,#42275,#42276,
#42277,#42278,#42279,#42280,#42281,#42282,#42283,#42284,#42285,#42286,#42287,
#42288,#42289,#42290,#42291,#42292,#42293,#42294,#42295,#42296,#42297,#42298,
#42299,#42300,#42301,#42302,#42303,#42304,#42305,#42306,#42307,#42308,#42309,
#42310,#42311,#42312,#42313,#42314,#42315,#42316,#42317,#42318,#42319,#42320,
#42321,#42322,#42323,#42324,#42325,#42326,#42327,#42328,#42329,#42330,#42331,
#42332,#42333,#42334,#42335,#42336,#42337,#42338,#42339,#42340,#42341,#42342,
#42343,#42344,#42345,#42346),(#42347,#42348,#42349,#42350,#42351,#42352,
#42353,#42354,#42355,#42356,#42357,#42358,#42359,#42360,#42361,#42362,#42363,
#42364,#42365,#42366,#42367,#42368,#42369,#42370,#42371,#42372,#42373,#42374,
#42375,#42376,#42377,#42378,#42379,#42380,#42381,#42382,#42383,#42384,#42385,
#42386,#42387,#42388,#42389,#42390,#42391,#42392,#42393,#42394,#42395,#42396,
#42397,#42398,#42399,#42400,#42401,#42402,#42403,#42404,#42405,#42406,#42407,
#42408,#42409,#42410,#42411,#42412,#42413,#42414,#42415,#42416,#42417,#42418,
#42419,#42420,#42421,#42422,#42423,#42424,#42425,#42426,#42427,#42428,#42429,
#42430,#42431,#42432),(#42433,#42434,#42435,#42436,#42437,#42438,#42439,
#42440,#42441,#42442,#42443,#42444,#42445,#42446,#42447,#42448,#42449,#42450,
#42451,#42452,#42453,#42454,#42455,#42456,#42457,#42458,#42459,#42460,#42461,
#42462,#42463,#42464,#42465,#42466,#42467,#42468,#42469,#42470,#42471,#42472,
#42473,#42474,#42475,#42476,#42477,#42478,#42479,#42480,#42481,#42482,#42483,
#42484,#42485,#42486,#42487,#42488,#42489,#42490,#42491,#42492,#42493,#42494,
#42495,#42496,#42497,#42498,#42499,#42500,#42501,#42502,#42503,#42504,#42505,
#42506,#42507,#42508,#42509,#42510,#42511,#42512,#42513,#42514,#42515,#42516,
#42517,#42518),(#42519,#42520,#42521,#42522,#42523,#42524,#42525,#42526,
#42527,#42528,#42529,#42530,#42531,#42532,#42533,#42534,#42535,#42536,#42537,
#42538,#42539,#42540,#42541,#42542,#42543,#42544,#42545,#42546,#42547,#42548,
#42549,#42550,#42551,#42552,#42553,#42554,#42555,#42556,#42557,#42558,#42559,
#42560,#42561,#42562,#42563,#42564,#42565,#42566,#42567,#42568,#42569,#42570,
#42571,#42572,#42573,#42574,#42575,#42576,#42577,#42578,#42579,#42580,#42581,
#42582,#42583,#42584,#42585,#42586,#42587,#42588,#42589,#42590,#42591,#42592,
#42593,#42594,#42595,#42596,#42597,#42598,#42599,#42600,#42601,#42602,#42603,
#42604)),.UNSPECIFIED.,.F.,.F.,.F.,(4,4),(4,1,1,1,1,1,1,1,1,1,1,1,1,1,1,
1,1,1,1,1,1,1,1,1,1,1,1,1,1,1,1,1,1,1,1,1,1,1,1,1,1,1,1,1,1,1,1,1,1,1,1,
1,1,1,1,1,1,1,1,1,1,1,1,1,1,1,1,1,1,1,1,1,1,1,1,1,1,1,1,1,1,1,1,4),(0.,
0.0658179306876173),(11.6150328478183,12.114859837712,12.6146868276058,
13.6143408073933,14.6139947871808,15.6136487669683,16.6133027467558,17.6129567265433,
18.6126107063308,19.6122646861183,20.6119186659058,21.6115726456933,22.6112266254809,
23.6108806052684,24.6105345850559,25.6101885648434,26.6098425446309,27.6094965244184,
28.6091505042059,29.6088044839934,30.6084584637809,31.6081124435684,32.6077664233559,
33.6074204031435,34.607074382931,35.6067283627185,36.606382342506,37.6060363222935,
38.605690302081,39.6053442818685,40.604998261656,41.6046522414435,42.604306221231,
43.6039602010186,44.6036141808061,45.6032681605936,46.6029221403811,47.6025761201686,
48.6022300999561,49.6018840797436,50.6015380595311,51.6011920393186,52.6008460191061,
53.6004999988936,54.6001539786812,55.5998079584687,56.5994619382562,57.5991159180437,
58.5987698978312,59.5984238776187,60.5980778574062,61.5977318371937,62.5973858169812,
63.5970397967687,64.5966937765562,65.5963477563437,66.5960017361313,67.5956557159188,
68.5953096957063,69.5949636754938,70.5946176552813,71.5942716350688,72.5939256148563,
73.5935795946438,74.5932335744313,75.5928875542188,76.5925415340064,77.5921955137939,
78.5918494935814,79.5915034733689,80.5911574531564,81.5908114329439,82.5904654127314,
83.5901193925189,84.5897733723064,85.5894273520939,86.5890813318814,87.588735311669,
88.5883892914565,89.588043271244,90.5876972510315,91.587351230819,92.0871782207128,
92.5870052106065),.UNSPECIFIED.);
#909=B_SPLINE_SURFACE_WITH_KNOTS('',2,1,((#42729,#42730),(#42731,#42732),
(#42733,#42734)),.UNSPECIFIED.,.F.,.F.,.F.,(3,3),(2,2),(0.,1.),(0.,0.0249999999999999),
 .UNSPECIFIED.);
#910=B_SPLINE_SURFACE_WITH_KNOTS('',2,1,((#42747,#42748),(#42749,#42750),
(#42751,#42752)),.UNSPECIFIED.,.F.,.F.,.F.,(3,3),(2,2),(0.,1.),(0.,0.0249999999999999),
 .UNSPECIFIED.);
#911=B_SPLINE_SURFACE_WITH_KNOTS('',2,1,((#42762,#42763),(#42764,#42765),
(#42766,#42767)),.UNSPECIFIED.,.F.,.F.,.F.,(3,3),(2,2),(0.,1.),(0.,0.0249999999999999),
 .UNSPECIFIED.);
#912=B_SPLINE_SURFACE_WITH_KNOTS('',2,1,((#42777,#42778),(#42779,#42780),
(#42781,#42782)),.UNSPECIFIED.,.F.,.F.,.F.,(3,3),(2,2),(0.,1.),(0.,0.0249999999999999),
 .UNSPECIFIED.);
#913=B_SPLINE_SURFACE_WITH_KNOTS('',2,1,((#42792,#42793),(#42794,#42795),
(#42796,#42797)),.UNSPECIFIED.,.F.,.F.,.F.,(3,3),(2,2),(0.,1.),(0.,0.0249999999999999),
 .UNSPECIFIED.);
#914=B_SPLINE_SURFACE_WITH_KNOTS('',2,1,((#42807,#42808),(#42809,#42810),
(#42811,#42812)),.UNSPECIFIED.,.F.,.F.,.F.,(3,3),(2,2),(0.,1.),(0.,0.0249999999999999),
 .UNSPECIFIED.);
#915=B_SPLINE_SURFACE_WITH_KNOTS('',2,1,((#42822,#42823),(#42824,#42825),
(#42826,#42827)),.UNSPECIFIED.,.F.,.F.,.F.,(3,3),(2,2),(0.,1.),(0.,0.0249999999999999),
 .UNSPECIFIED.);
#916=B_SPLINE_SURFACE_WITH_KNOTS('',2,1,((#42837,#42838),(#42839,#42840),
(#42841,#42842)),.UNSPECIFIED.,.F.,.F.,.F.,(3,3),(2,2),(0.,1.),(0.,0.0249999999999999),
 .UNSPECIFIED.);
#917=B_SPLINE_SURFACE_WITH_KNOTS('',2,1,((#42852,#42853),(#42854,#42855),
(#42856,#42857)),.UNSPECIFIED.,.F.,.F.,.F.,(3,3),(2,2),(0.,1.),(0.,0.0249999999999999),
 .UNSPECIFIED.);
#918=B_SPLINE_SURFACE_WITH_KNOTS('',2,1,((#42867,#42868),(#42869,#42870),
(#42871,#42872)),.UNSPECIFIED.,.F.,.F.,.F.,(3,3),(2,2),(0.,1.),(0.,0.0249999999999999),
 .UNSPECIFIED.);
#919=B_SPLINE_SURFACE_WITH_KNOTS('',2,1,((#42882,#42883),(#42884,#42885),
(#42886,#42887)),.UNSPECIFIED.,.F.,.F.,.F.,(3,3),(2,2),(0.,1.),(0.,0.0249999999999999),
 .UNSPECIFIED.);
#920=B_SPLINE_SURFACE_WITH_KNOTS('',2,1,((#42956,#42957),(#42958,#42959),
(#42960,#42961)),.UNSPECIFIED.,.F.,.F.,.F.,(3,3),(2,2),(0.,1.),(0.,0.0249999999999999),
 .UNSPECIFIED.);
#921=B_SPLINE_SURFACE_WITH_KNOTS('',2,1,((#42974,#42975),(#42976,#42977),
(#42978,#42979)),.UNSPECIFIED.,.F.,.F.,.F.,(3,3),(2,2),(0.,1.),(0.,0.0249999999999999),
 .UNSPECIFIED.);
#922=B_SPLINE_SURFACE_WITH_KNOTS('',2,1,((#42989,#42990),(#42991,#42992),
(#42993,#42994)),.UNSPECIFIED.,.F.,.F.,.F.,(3,3),(2,2),(0.,1.),(0.,0.0249999999999999),
 .UNSPECIFIED.);
#923=B_SPLINE_SURFACE_WITH_KNOTS('',2,1,((#43004,#43005),(#43006,#43007),
(#43008,#43009)),.UNSPECIFIED.,.F.,.F.,.F.,(3,3),(2,2),(0.,1.),(0.,0.0249999999999999),
 .UNSPECIFIED.);
#924=B_SPLINE_SURFACE_WITH_KNOTS('',2,1,((#43019,#43020),(#43021,#43022),
(#43023,#43024)),.UNSPECIFIED.,.F.,.F.,.F.,(3,3),(2,2),(0.,1.),(0.,0.0249999999999999),
 .UNSPECIFIED.);
#925=B_SPLINE_SURFACE_WITH_KNOTS('',2,1,((#43034,#43035),(#43036,#43037),
(#43038,#43039)),.UNSPECIFIED.,.F.,.F.,.F.,(3,3),(2,2),(0.,1.),(0.,0.0249999999999999),
 .UNSPECIFIED.);
#926=B_SPLINE_SURFACE_WITH_KNOTS('',2,1,((#43049,#43050),(#43051,#43052),
(#43053,#43054)),.UNSPECIFIED.,.F.,.F.,.F.,(3,3),(2,2),(0.,1.),(0.,0.0249999999999999),
 .UNSPECIFIED.);
#927=B_SPLINE_SURFACE_WITH_KNOTS('',2,1,((#43064,#43065),(#43066,#43067),
(#43068,#43069)),.UNSPECIFIED.,.F.,.F.,.F.,(3,3),(2,2),(0.,1.),(0.,0.0249999999999999),
 .UNSPECIFIED.);
#928=B_SPLINE_SURFACE_WITH_KNOTS('',2,1,((#43079,#43080),(#43081,#43082),
(#43083,#43084)),.UNSPECIFIED.,.F.,.F.,.F.,(3,3),(2,2),(0.,1.),(0.,0.0249999999999999),
 .UNSPECIFIED.);
#929=B_SPLINE_SURFACE_WITH_KNOTS('',2,1,((#43094,#43095),(#43096,#43097),
(#43098,#43099)),.UNSPECIFIED.,.F.,.F.,.F.,(3,3),(2,2),(0.,1.),(0.,0.0249999999999999),
 .UNSPECIFIED.);
#930=B_SPLINE_SURFACE_WITH_KNOTS('',2,1,((#43109,#43110),(#43111,#43112),
(#43113,#43114)),.UNSPECIFIED.,.F.,.F.,.F.,(3,3),(2,2),(0.,1.),(0.,0.0249999999999999),
 .UNSPECIFIED.);
#931=B_SPLINE_SURFACE_WITH_KNOTS('',3,3,((#43985,#43986,#43987,#43988,#43989,
#43990,#43991,#43992),(#43993,#43994,#43995,#43996,#43997,#43998,#43999,
#44000),(#44001,#44002,#44003,#44004,#44005,#44006,#44007,#44008),(#44009,
#44010,#44011,#44012,#44013,#44014,#44015,#44016)),.UNSPECIFIED.,.F.,.F.,
 .F.,(4,4),(4,1,1,1,1,4),(0.,1.),(0.,0.142857142857143,0.428571428571429,
0.571428571428571,0.857142857142857,1.),.UNSPECIFIED.);
#932=B_SPLINE_SURFACE_WITH_KNOTS('',3,3,((#44136,#44137,#44138,#44139,#44140,
#44141),(#44142,#44143,#44144,#44145,#44146,#44147),(#44148,#44149,#44150,
#44151,#44152,#44153),(#44154,#44155,#44156,#44157,#44158,#44159)),
 .UNSPECIFIED.,.F.,.F.,.F.,(4,4),(4,1,1,4),(0.,1.),(-1.83137755752329,-1.04650146144188,
-0.52325073072094,-1.12036785251785E-15),.UNSPECIFIED.);
#933=B_SPLINE_SURFACE_WITH_KNOTS('',3,3,((#44271,#44272,#44273,#44274,#44275,
#44276,#44277,#44278),(#44279,#44280,#44281,#44282,#44283,#44284,#44285,
#44286),(#44287,#44288,#44289,#44290,#44291,#44292,#44293,#44294),(#44295,
#44296,#44297,#44298,#44299,#44300,#44301,#44302)),.UNSPECIFIED.,.F.,.F.,
 .F.,(4,4),(4,1,1,1,1,4),(0.,1.),(0.,0.142857142857143,0.428571428571429,
0.571428571428571,0.857142857142857,1.),.UNSPECIFIED.);
#934=B_SPLINE_SURFACE_WITH_KNOTS('',3,3,((#44422,#44423,#44424,#44425,#44426,
#44427),(#44428,#44429,#44430,#44431,#44432,#44433),(#44434,#44435,#44436,
#44437,#44438,#44439),(#44440,#44441,#44442,#44443,#44444,#44445)),
 .UNSPECIFIED.,.F.,.F.,.F.,(4,4),(4,1,1,4),(0.,1.),(-1.83137755752328,-1.04650146144188,
-0.523250730720938,-1.19348975147204E-15),.UNSPECIFIED.);
#935=B_SPLINE_SURFACE_WITH_KNOTS('',3,3,((#44475,#44476,#44477,#44478,#44479,
#44480,#44481,#44482),(#44483,#44484,#44485,#44486,#44487,#44488,#44489,
#44490),(#44491,#44492,#44493,#44494,#44495,#44496,#44497,#44498),(#44499,
#44500,#44501,#44502,#44503,#44504,#44505,#44506)),.UNSPECIFIED.,.F.,.F.,
 .F.,(4,4),(4,1,1,1,1,4),(0.,1.),(0.,0.142857142857143,0.428571428571429,
0.571428571428571,0.857142857142857,1.),.UNSPECIFIED.);
#936=B_SPLINE_SURFACE_WITH_KNOTS('',3,3,((#44567,#44568,#44569,#44570,#44571,
#44572,#44573,#44574),(#44575,#44576,#44577,#44578,#44579,#44580,#44581,
#44582),(#44583,#44584,#44585,#44586,#44587,#44588,#44589,#44590),(#44591,
#44592,#44593,#44594,#44595,#44596,#44597,#44598)),.UNSPECIFIED.,.F.,.F.,
 .F.,(4,4),(4,1,1,1,1,4),(0.,1.),(0.,0.142857142857143,0.428571428571429,
0.571428571428571,0.857142857142857,1.),.UNSPECIFIED.);
#937=B_SPLINE_SURFACE_WITH_KNOTS('',3,3,((#44718,#44719,#44720,#44721,#44722,
#44723,#44724),(#44725,#44726,#44727,#44728,#44729,#44730,#44731),(#44732,
#44733,#44734,#44735,#44736,#44737,#44738),(#44739,#44740,#44741,#44742,
#44743,#44744,#44745)),.UNSPECIFIED.,.F.,.F.,.F.,(4,4),(4,1,1,1,4),(0.,
1.),(-1.84798528578773,-1.0559915918787,-0.527995795939349,-0.263997897969672,
4.44089209850066E-15),.UNSPECIFIED.);
#938=B_SPLINE_SURFACE_WITH_KNOTS('',3,3,((#44763,#44764,#44765,#44766,#44767,
#44768,#44769),(#44770,#44771,#44772,#44773,#44774,#44775,#44776),(#44777,
#44778,#44779,#44780,#44781,#44782,#44783),(#44784,#44785,#44786,#44787,
#44788,#44789,#44790)),.UNSPECIFIED.,.F.,.F.,.F.,(4,4),(4,1,1,1,4),(0.,
1.),(-1.84798528578773,-1.0559915918787,-0.527995795939349,-0.263997897969673,
2.22044604925035E-15),.UNSPECIFIED.);
#939=FACE_BOUND('',#2792,.T.);
#940=FACE_BOUND('',#2795,.T.);
#941=FACE_BOUND('',#2847,.T.);
#942=FACE_BOUND('',#2848,.T.);
#943=FACE_BOUND('',#2849,.T.);
#944=FACE_BOUND('',#2850,.T.);
#945=FACE_BOUND('',#2877,.T.);
#946=FACE_BOUND('',#2892,.T.);
#947=FACE_BOUND('',#3007,.T.);
#948=FACE_BOUND('',#3010,.T.);
#949=FACE_BOUND('',#3014,.T.);
#950=FACE_BOUND('',#3019,.T.);
#951=FACE_BOUND('',#3037,.T.);
#952=FACE_BOUND('',#3048,.T.);
#953=FACE_BOUND('',#3050,.T.);
#954=FACE_BOUND('',#3052,.T.);
#955=FACE_BOUND('',#3055,.T.);
#956=FACE_BOUND('',#3059,.T.);
#957=FACE_BOUND('',#3065,.T.);
#958=FACE_BOUND('',#3069,.T.);
#959=FACE_BOUND('',#3073,.T.);
#960=FACE_BOUND('',#3076,.T.);
#961=FACE_BOUND('',#3079,.T.);
#962=FACE_BOUND('',#3082,.T.);
#963=FACE_BOUND('',#3092,.T.);
#964=FACE_BOUND('',#3095,.T.);
#965=FACE_BOUND('',#3127,.T.);
#966=FACE_BOUND('',#3128,.T.);
#967=FACE_BOUND('',#3129,.T.);
#968=FACE_BOUND('',#3130,.T.);
#969=FACE_BOUND('',#3131,.T.);
#970=FACE_BOUND('',#3232,.T.);
#971=FACE_BOUND('',#3235,.T.);
#972=FACE_BOUND('',#3238,.T.);
#973=FACE_BOUND('',#3241,.T.);
#974=FACE_BOUND('',#3271,.T.);
#975=FACE_BOUND('',#3281,.T.);
#976=FACE_BOUND('',#3285,.T.);
#977=FACE_BOUND('',#3288,.T.);
#978=FACE_BOUND('',#3291,.T.);
#979=FACE_BOUND('',#3322,.T.);
#980=FACE_BOUND('',#3323,.T.);
#981=FACE_BOUND('',#3324,.T.);
#982=FACE_BOUND('',#3325,.T.);
#983=FACE_BOUND('',#3326,.T.);
#984=FACE_BOUND('',#3327,.T.);
#985=FACE_BOUND('',#3328,.T.);
#986=FACE_BOUND('',#3329,.T.);
#987=FACE_BOUND('',#3330,.T.);
#988=FACE_BOUND('',#3331,.T.);
#989=FACE_BOUND('',#3332,.T.);
#990=FACE_BOUND('',#3333,.T.);
#991=FACE_BOUND('',#3334,.T.);
#992=FACE_BOUND('',#3335,.T.);
#993=FACE_BOUND('',#3336,.T.);
#994=FACE_BOUND('',#3337,.T.);
#995=FACE_BOUND('',#3338,.T.);
#996=FACE_BOUND('',#3339,.T.);
#997=FACE_BOUND('',#3340,.T.);
#998=FACE_BOUND('',#3341,.T.);
#999=FACE_BOUND('',#3342,.T.);
#1000=FACE_BOUND('',#3450,.T.);
#1001=FACE_BOUND('',#3456,.T.);
#1002=FACE_BOUND('',#3459,.T.);
#1003=FACE_BOUND('',#3474,.T.);
#1004=FACE_BOUND('',#3508,.T.);
#1005=FACE_BOUND('',#3567,.T.);
#1006=FACE_BOUND('',#3697,.T.);
#1007=FACE_BOUND('',#3700,.T.);
#1008=FACE_BOUND('',#3701,.T.);
#1009=FACE_BOUND('',#3702,.T.);
#1010=FACE_BOUND('',#3703,.T.);
#1011=FACE_BOUND('',#3704,.T.);
#1012=FACE_BOUND('',#3705,.T.);
#1013=FACE_BOUND('',#3706,.T.);
#1014=FACE_BOUND('',#3707,.T.);
#1015=FACE_BOUND('',#3708,.T.);
#1016=FACE_BOUND('',#3709,.T.);
#1017=FACE_BOUND('',#3710,.T.);
#1018=FACE_BOUND('',#3711,.T.);
#1019=FACE_BOUND('',#3712,.T.);
#1020=FACE_BOUND('',#3713,.T.);
#1021=FACE_BOUND('',#3714,.T.);
#1022=FACE_BOUND('',#3715,.T.);
#1023=FACE_BOUND('',#3716,.T.);
#1024=FACE_BOUND('',#3717,.T.);
#1025=FACE_BOUND('',#3718,.T.);
#1026=FACE_BOUND('',#3719,.T.);
#1027=FACE_BOUND('',#3720,.T.);
#1028=FACE_BOUND('',#3721,.T.);
#1029=FACE_BOUND('',#3722,.T.);
#1030=FACE_BOUND('',#3723,.T.);
#1031=FACE_BOUND('',#3724,.T.);
#1032=FACE_BOUND('',#3725,.T.);
#1033=FACE_BOUND('',#3726,.T.);
#1034=FACE_BOUND('',#3727,.T.);
#1035=FACE_BOUND('',#3728,.T.);
#1036=FACE_BOUND('',#3731,.T.);
#1037=FACE_BOUND('',#3732,.T.);
#1038=FACE_BOUND('',#3733,.T.);
#1039=FACE_BOUND('',#3734,.T.);
#1040=FACE_BOUND('',#3735,.T.);
#1041=FACE_BOUND('',#3736,.T.);
#1042=FACE_BOUND('',#3746,.T.);
#1043=FACE_BOUND('',#3747,.T.);
#1044=FACE_BOUND('',#3762,.T.);
#1045=FACE_BOUND('',#3763,.T.);
#1046=FACE_BOUND('',#3770,.T.);
#1047=FACE_BOUND('',#3771,.T.);
#1048=FACE_BOUND('',#3784,.T.);
#1049=FACE_BOUND('',#3785,.T.);
#1050=FACE_BOUND('',#3806,.T.);
#1051=FACE_BOUND('',#3821,.T.);
#1052=FACE_BOUND('',#3822,.T.);
#1053=FACE_BOUND('',#3835,.T.);
#1054=FACE_BOUND('',#3836,.T.);
#1055=FACE_BOUND('',#3846,.T.);
#1056=FACE_BOUND('',#3849,.T.);
#1057=FACE_BOUND('',#3852,.T.);
#1058=FACE_BOUND('',#3855,.T.);
#1059=FACE_BOUND('',#3866,.T.);
#1060=FACE_BOUND('',#3873,.T.);
#1061=FACE_BOUND('',#3876,.T.);
#1062=PLANE('',#16766);
#1063=PLANE('',#16770);
#1064=PLANE('',#16774);
#1065=PLANE('',#16776);
#1066=PLANE('',#16781);
#1067=PLANE('',#16783);
#1068=PLANE('',#16786);
#1069=PLANE('',#16789);
#1070=PLANE('',#16801);
#1071=PLANE('',#16855);
#1072=PLANE('',#16856);
#1073=PLANE('',#16861);
#1074=PLANE('',#16867);
#1075=PLANE('',#16869);
#1076=PLANE('',#16873);
#1077=PLANE('',#16885);
#1078=PLANE('',#16888);
#1079=PLANE('',#16898);
#1080=PLANE('',#16933);
#1081=PLANE('',#16936);
#1082=PLANE('',#16938);
#1083=PLANE('',#16939);
#1084=PLANE('',#16940);
#1085=PLANE('',#16941);
#1086=PLANE('',#16942);
#1087=PLANE('',#16943);
#1088=PLANE('',#16944);
#1089=PLANE('',#16945);
#1090=PLANE('',#16946);
#1091=PLANE('',#16947);
#1092=PLANE('',#16948);
#1093=PLANE('',#16949);
#1094=PLANE('',#16950);
#1095=PLANE('',#16951);
#1096=PLANE('',#16952);
#1097=PLANE('',#16953);
#1098=PLANE('',#16954);
#1099=PLANE('',#16955);
#1100=PLANE('',#16956);
#1101=PLANE('',#16957);
#1102=PLANE('',#16958);
#1103=PLANE('',#16959);
#1104=PLANE('',#16962);
#1105=PLANE('',#16966);
#1106=PLANE('',#16967);
#1107=PLANE('',#16968);
#1108=PLANE('',#17034);
#1109=PLANE('',#17038);
#1110=PLANE('',#17046);
#1111=PLANE('',#17055);
#1112=PLANE('',#17057);
#1113=PLANE('',#17062);
#1114=PLANE('',#17071);
#1115=PLANE('',#17079);
#1116=PLANE('',#17091);
#1117=PLANE('',#17092);
#1118=PLANE('',#17098);
#1119=PLANE('',#17099);
#1120=PLANE('',#17102);
#1121=PLANE('',#17107);
#1122=PLANE('',#17115);
#1123=PLANE('',#17116);
#1124=PLANE('',#17122);
#1125=PLANE('',#17128);
#1126=PLANE('',#17132);
#1127=PLANE('',#17136);
#1128=PLANE('',#17140);
#1129=PLANE('',#17146);
#1130=PLANE('',#17150);
#1131=PLANE('',#17151);
#1132=PLANE('',#17160);
#1133=PLANE('',#17164);
#1134=PLANE('',#17166);
#1135=PLANE('',#17174);
#1136=PLANE('',#17176);
#1137=PLANE('',#17177);
#1138=PLANE('',#17178);
#1139=PLANE('',#17179);
#1140=PLANE('',#17180);
#1141=PLANE('',#17181);
#1142=PLANE('',#17182);
#1143=PLANE('',#17183);
#1144=PLANE('',#17184);
#1145=PLANE('',#17185);
#1146=PLANE('',#17186);
#1147=PLANE('',#17187);
#1148=PLANE('',#17188);
#1149=PLANE('',#17189);
#1150=PLANE('',#17190);
#1151=PLANE('',#17191);
#1152=PLANE('',#17192);
#1153=PLANE('',#17193);
#1154=PLANE('',#17194);
#1155=PLANE('',#17195);
#1156=PLANE('',#17196);
#1157=PLANE('',#17197);
#1158=PLANE('',#17198);
#1159=PLANE('',#17199);
#1160=PLANE('',#17200);
#1161=PLANE('',#17201);
#1162=PLANE('',#17202);
#1163=PLANE('',#17203);
#1164=PLANE('',#17204);
#1165=PLANE('',#17205);
#1166=PLANE('',#17206);
#1167=PLANE('',#17207);
#1168=PLANE('',#17208);
#1169=PLANE('',#17209);
#1170=PLANE('',#17210);
#1171=PLANE('',#17211);
#1172=PLANE('',#17212);
#1173=PLANE('',#17213);
#1174=PLANE('',#17214);
#1175=PLANE('',#17215);
#1176=PLANE('',#17216);
#1177=PLANE('',#17217);
#1178=PLANE('',#17218);
#1179=PLANE('',#17219);
#1180=PLANE('',#17220);
#1181=PLANE('',#17221);
#1182=PLANE('',#17222);
#1183=PLANE('',#17223);
#1184=PLANE('',#17224);
#1185=PLANE('',#17225);
#1186=PLANE('',#17226);
#1187=PLANE('',#17227);
#1188=PLANE('',#17228);
#1189=PLANE('',#17229);
#1190=PLANE('',#17230);
#1191=PLANE('',#17231);
#1192=PLANE('',#17232);
#1193=PLANE('',#17233);
#1194=PLANE('',#17234);
#1195=PLANE('',#17235);
#1196=PLANE('',#17236);
#1197=PLANE('',#17237);
#1198=PLANE('',#17238);
#1199=PLANE('',#17239);
#1200=PLANE('',#17240);
#1201=PLANE('',#17241);
#1202=PLANE('',#17242);
#1203=PLANE('',#17243);
#1204=PLANE('',#17244);
#1205=PLANE('',#17245);
#1206=PLANE('',#17246);
#1207=PLANE('',#17247);
#1208=PLANE('',#17248);
#1209=PLANE('',#17249);
#1210=PLANE('',#17250);
#1211=PLANE('',#17251);
#1212=PLANE('',#17252);
#1213=PLANE('',#17254);
#1214=PLANE('',#17260);
#1215=PLANE('',#17264);
#1216=PLANE('',#17268);
#1217=PLANE('',#17272);
#1218=PLANE('',#17278);
#1219=PLANE('',#17312);
#1220=PLANE('',#17319);
#1221=PLANE('',#17328);
#1222=PLANE('',#17333);
#1223=PLANE('',#17337);
#1224=PLANE('',#17341);
#1225=PLANE('',#17372);
#1226=PLANE('',#17375);
#1227=PLANE('',#17377);
#1228=PLANE('',#17439);
#1229=PLANE('',#17440);
#1230=PLANE('',#17445);
#1231=PLANE('',#17446);
#1232=PLANE('',#17447);
#1233=PLANE('',#17448);
#1234=PLANE('',#17449);
#1235=PLANE('',#17450);
#1236=PLANE('',#17451);
#1237=PLANE('',#17452);
#1238=PLANE('',#17453);
#1239=PLANE('',#17454);
#1240=PLANE('',#17455);
#1241=PLANE('',#17456);
#1242=PLANE('',#17457);
#1243=PLANE('',#17458);
#1244=PLANE('',#17459);
#1245=PLANE('',#17460);
#1246=PLANE('',#17461);
#1247=PLANE('',#17462);
#1248=PLANE('',#17463);
#1249=PLANE('',#17464);
#1250=PLANE('',#17465);
#1251=PLANE('',#17466);
#1252=PLANE('',#17467);
#1253=PLANE('',#17468);
#1254=PLANE('',#17469);
#1255=PLANE('',#17470);
#1256=PLANE('',#17471);
#1257=PLANE('',#17472);
#1258=PLANE('',#17473);
#1259=PLANE('',#17474);
#1260=PLANE('',#17475);
#1261=PLANE('',#17476);
#1262=PLANE('',#17477);
#1263=PLANE('',#17478);
#1264=PLANE('',#17479);
#1265=PLANE('',#17480);
#1266=PLANE('',#17481);
#1267=PLANE('',#17482);
#1268=PLANE('',#17483);
#1269=PLANE('',#17484);
#1270=PLANE('',#17485);
#1271=PLANE('',#17486);
#1272=PLANE('',#17487);
#1273=PLANE('',#17488);
#1274=PLANE('',#17489);
#1275=PLANE('',#17490);
#1276=PLANE('',#17491);
#1277=PLANE('',#17492);
#1278=PLANE('',#17493);
#1279=PLANE('',#17494);
#1280=PLANE('',#17495);
#1281=PLANE('',#17496);
#1282=PLANE('',#17497);
#1283=PLANE('',#17498);
#1284=PLANE('',#17499);
#1285=PLANE('',#17500);
#1286=PLANE('',#17501);
#1287=PLANE('',#17502);
#1288=PLANE('',#17503);
#1289=PLANE('',#17504);
#1290=PLANE('',#17505);
#1291=PLANE('',#17506);
#1292=PLANE('',#17507);
#1293=PLANE('',#17508);
#1294=PLANE('',#17509);
#1295=PLANE('',#17510);
#1296=PLANE('',#17511);
#1297=PLANE('',#17512);
#1298=PLANE('',#17513);
#1299=PLANE('',#17514);
#1300=PLANE('',#17515);
#1301=PLANE('',#17516);
#1302=PLANE('',#17517);
#1303=PLANE('',#17518);
#1304=PLANE('',#17519);
#1305=PLANE('',#17520);
#1306=PLANE('',#17521);
#1307=PLANE('',#17522);
#1308=PLANE('',#17523);
#1309=PLANE('',#17524);
#1310=PLANE('',#17525);
#1311=PLANE('',#17526);
#1312=PLANE('',#17527);
#1313=PLANE('',#17528);
#1314=PLANE('',#17529);
#1315=PLANE('',#17530);
#1316=PLANE('',#17531);
#1317=PLANE('',#17532);
#1318=PLANE('',#17533);
#1319=PLANE('',#17534);
#1320=PLANE('',#17535);
#1321=PLANE('',#17536);
#1322=PLANE('',#17537);
#1323=PLANE('',#17538);
#1324=PLANE('',#17539);
#1325=PLANE('',#17540);
#1326=PLANE('',#17541);
#1327=PLANE('',#17542);
#1328=PLANE('',#17547);
#1329=PLANE('',#17558);
#1330=PLANE('',#17562);
#1331=PLANE('',#17570);
#1332=PLANE('',#17571);
#1333=PLANE('',#17580);
#1334=PLANE('',#17595);
#1335=PLANE('',#17598);
#1336=PLANE('',#17629);
#1337=PLANE('',#17634);
#1338=PLANE('',#17637);
#1339=PLANE('',#17638);
#1340=PLANE('',#17639);
#1341=PLANE('',#17640);
#1342=PLANE('',#17641);
#1343=PLANE('',#17642);
#1344=PLANE('',#17643);
#1345=PLANE('',#17644);
#1346=PLANE('',#17645);
#1347=PLANE('',#17646);
#1348=PLANE('',#17647);
#1349=PLANE('',#17648);
#1350=PLANE('',#17649);
#1351=PLANE('',#17650);
#1352=PLANE('',#17651);
#1353=PLANE('',#17652);
#1354=PLANE('',#17653);
#1355=PLANE('',#17654);
#1356=PLANE('',#17655);
#1357=PLANE('',#17656);
#1358=PLANE('',#17657);
#1359=PLANE('',#17658);
#1360=PLANE('',#17659);
#1361=PLANE('',#17660);
#1362=PLANE('',#17661);
#1363=PLANE('',#17662);
#1364=PLANE('',#17663);
#1365=PLANE('',#17664);
#1366=PLANE('',#17665);
#1367=PLANE('',#17666);
#1368=PLANE('',#17667);
#1369=PLANE('',#17668);
#1370=PLANE('',#17669);
#1371=PLANE('',#17670);
#1372=PLANE('',#17671);
#1373=PLANE('',#17672);
#1374=PLANE('',#17679);
#1375=PLANE('',#17680);
#1376=PLANE('',#17681);
#1377=PLANE('',#17683);
#1378=PLANE('',#17684);
#1379=PLANE('',#17686);
#1380=PLANE('',#17687);
#1381=PLANE('',#17689);
#1382=PLANE('',#17690);
#1383=PLANE('',#17692);
#1384=PLANE('',#17693);
#1385=PLANE('',#17695);
#1386=PLANE('',#17696);
#1387=PLANE('',#17698);
#1388=PLANE('',#17699);
#1389=PLANE('',#17701);
#1390=PLANE('',#17702);
#1391=PLANE('',#17704);
#1392=PLANE('',#17705);
#1393=PLANE('',#17707);
#1394=PLANE('',#17708);
#1395=PLANE('',#17710);
#1396=PLANE('',#17711);
#1397=PLANE('',#17713);
#1398=PLANE('',#17714);
#1399=PLANE('',#17716);
#1400=PLANE('',#17717);
#1401=PLANE('',#17719);
#1402=PLANE('',#17720);
#1403=PLANE('',#17722);
#1404=PLANE('',#17723);
#1405=PLANE('',#17725);
#1406=PLANE('',#17726);
#1407=PLANE('',#17728);
#1408=PLANE('',#17729);
#1409=PLANE('',#17731);
#1410=PLANE('',#17732);
#1411=PLANE('',#17734);
#1412=PLANE('',#17735);
#1413=PLANE('',#17737);
#1414=PLANE('',#17738);
#1415=PLANE('',#17740);
#1416=PLANE('',#17741);
#1417=PLANE('',#17743);
#1418=PLANE('',#17744);
#1419=PLANE('',#17746);
#1420=PLANE('',#17747);
#1421=PLANE('',#17749);
#1422=PLANE('',#17750);
#1423=PLANE('',#17752);
#1424=PLANE('',#17753);
#1425=PLANE('',#17755);
#1426=PLANE('',#17756);
#1427=PLANE('',#17758);
#1428=PLANE('',#17759);
#1429=PLANE('',#17761);
#1430=PLANE('',#17762);
#1431=PLANE('',#17764);
#1432=PLANE('',#17765);
#1433=PLANE('',#17768);
#1434=PLANE('',#17769);
#1435=PLANE('',#17772);
#1436=PLANE('',#17773);
#1437=PLANE('',#17775);
#1438=PLANE('',#17776);
#1439=PLANE('',#17778);
#1440=PLANE('',#17779);
#1441=PLANE('',#17781);
#1442=PLANE('',#17782);
#1443=PLANE('',#17784);
#1444=PLANE('',#17785);
#1445=PLANE('',#17787);
#1446=PLANE('',#17788);
#1447=PLANE('',#17790);
#1448=PLANE('',#17791);
#1449=PLANE('',#17793);
#1450=PLANE('',#17794);
#1451=PLANE('',#17796);
#1452=PLANE('',#17797);
#1453=PLANE('',#17799);
#1454=PLANE('',#17800);
#1455=PLANE('',#17802);
#1456=PLANE('',#17803);
#1457=PLANE('',#17805);
#1458=PLANE('',#17806);
#1459=PLANE('',#17808);
#1460=PLANE('',#17809);
#1461=PLANE('',#17811);
#1462=PLANE('',#17812);
#1463=PLANE('',#17814);
#1464=PLANE('',#17815);
#1465=PLANE('',#17817);
#1466=PLANE('',#17818);
#1467=PLANE('',#17820);
#1468=PLANE('',#17821);
#1469=PLANE('',#17823);
#1470=PLANE('',#17824);
#1471=PLANE('',#17826);
#1472=PLANE('',#17827);
#1473=PLANE('',#17829);
#1474=PLANE('',#17830);
#1475=PLANE('',#17832);
#1476=PLANE('',#17833);
#1477=PLANE('',#17835);
#1478=PLANE('',#17836);
#1479=PLANE('',#17838);
#1480=PLANE('',#17839);
#1481=PLANE('',#17841);
#1482=PLANE('',#17842);
#1483=PLANE('',#17844);
#1484=PLANE('',#17845);
#1485=PLANE('',#17847);
#1486=PLANE('',#17848);
#1487=PLANE('',#17850);
#1488=PLANE('',#17851);
#1489=PLANE('',#17853);
#1490=PLANE('',#17854);
#1491=PLANE('',#17856);
#1492=PLANE('',#17857);
#1493=PLANE('',#17859);
#1494=PLANE('',#17860);
#1495=PLANE('',#17862);
#1496=PLANE('',#17870);
#1497=PLANE('',#17878);
#1498=PLANE('',#17880);
#1499=PLANE('',#17881);
#1500=PLANE('',#17882);
#1501=PLANE('',#17883);
#1502=PLANE('',#17884);
#1503=PLANE('',#17885);
#1504=PLANE('',#17889);
#1505=PLANE('',#17890);
#1506=PLANE('',#17893);
#1507=PLANE('',#17894);
#1508=PLANE('',#17898);
#1509=PLANE('',#17899);
#1510=PLANE('',#17901);
#1511=PLANE('',#17902);
#1512=PLANE('',#17905);
#1513=PLANE('',#17906);
#1514=PLANE('',#17907);
#1515=PLANE('',#17909);
#1516=PLANE('',#17914);
#1517=PLANE('',#17919);
#1518=PLANE('',#17922);
#1519=PLANE('',#17923);
#1520=PLANE('',#17933);
#1521=PLANE('',#17942);
#1522=PLANE('',#17954);
#1523=PLANE('',#17955);
#1524=PLANE('',#17956);
#1525=PLANE('',#17957);
#1526=PLANE('',#17968);
#1527=PLANE('',#17978);
#1528=PLANE('',#17979);
#1529=PLANE('',#17991);
#1530=PLANE('',#17995);
#1531=PLANE('',#17996);
#1532=PLANE('',#17999);
#1533=PLANE('',#18002);
#1534=PLANE('',#18005);
#1535=PLANE('',#18011);
#1536=PLANE('',#18012);
#1537=PLANE('',#18015);
#1538=PLANE('',#18020);
#1539=PLANE('',#18023);
#1540=PLANE('',#18027);
#1541=PLANE('',#18029);
#1542=PLANE('',#18035);
#1543=PLANE('',#18039);
#1544=PLANE('',#18043);
#1545=PLANE('',#18047);
#1546=PLANE('',#18053);
#1547=PLANE('',#18058);
#1548=PLANE('',#18059);
#1549=PLANE('',#18060);
#1550=PLANE('',#18061);
#1551=PLANE('',#18064);
#1552=PLANE('',#18068);
#1553=PLANE('',#18069);
#1554=PLANE('',#18070);
#1555=PLANE('',#18071);
#1556=PLANE('',#18072);
#1557=PLANE('',#18075);
#1558=PLANE('',#18077);
#1559=PLANE('',#18086);
#1560=PLANE('',#18090);
#1561=PLANE('',#18091);
#1562=PLANE('',#18092);
#1563=CYLINDRICAL_SURFACE('',#16764,15.2);
#1564=CYLINDRICAL_SURFACE('',#16779,1.5);
#1565=CYLINDRICAL_SURFACE('',#16784,1.5);
#1566=CYLINDRICAL_SURFACE('',#16787,1.5);
#1567=CYLINDRICAL_SURFACE('',#16790,1.5);
#1568=CYLINDRICAL_SURFACE('',#16799,1.5);
#1569=CYLINDRICAL_SURFACE('',#16800,1.5);
#1570=CYLINDRICAL_SURFACE('',#16806,1.5);
#1571=CYLINDRICAL_SURFACE('',#16807,1.5);
#1572=CYLINDRICAL_SURFACE('',#16815,1.5);
#1573=CYLINDRICAL_SURFACE('',#16816,1.5);
#1574=CYLINDRICAL_SURFACE('',#16825,1.5);
#1575=CYLINDRICAL_SURFACE('',#16826,1.5);
#1576=CYLINDRICAL_SURFACE('',#16834,1.5);
#1577=CYLINDRICAL_SURFACE('',#16835,1.5);
#1578=CYLINDRICAL_SURFACE('',#16840,1.5);
#1579=CYLINDRICAL_SURFACE('',#16845,1.5);
#1580=CYLINDRICAL_SURFACE('',#16847,1.5);
#1581=CYLINDRICAL_SURFACE('',#16852,1.5);
#1582=CYLINDRICAL_SURFACE('',#16857,1.5);
#1583=CYLINDRICAL_SURFACE('',#16858,1.5);
#1584=CYLINDRICAL_SURFACE('',#16859,1.5);
#1585=CYLINDRICAL_SURFACE('',#16862,1.5);
#1586=CYLINDRICAL_SURFACE('',#16863,1.5);
#1587=CYLINDRICAL_SURFACE('',#16865,1.5);
#1588=CYLINDRICAL_SURFACE('',#16866,1.5);
#1589=CYLINDRICAL_SURFACE('',#16871,1.5);
#1590=CYLINDRICAL_SURFACE('',#16872,1.5);
#1591=CYLINDRICAL_SURFACE('',#16878,1.5);
#1592=CYLINDRICAL_SURFACE('',#16879,1.5);
#1593=CYLINDRICAL_SURFACE('',#16884,1.5);
#1594=CYLINDRICAL_SURFACE('',#16886,1.5);
#1595=CYLINDRICAL_SURFACE('',#16887,1.5);
#1596=CYLINDRICAL_SURFACE('',#16904,27.);
#1597=CYLINDRICAL_SURFACE('',#16911,1.5);
#1598=CYLINDRICAL_SURFACE('',#16917,1.5);
#1599=CYLINDRICAL_SURFACE('',#16923,1.5);
#1600=CYLINDRICAL_SURFACE('',#16931,1.5);
#1601=CYLINDRICAL_SURFACE('',#16935,3.);
#1602=CYLINDRICAL_SURFACE('',#16937,3.);
#1603=CYLINDRICAL_SURFACE('',#16960,3.05);
#1604=CYLINDRICAL_SURFACE('',#16965,21.05);
#1605=CYLINDRICAL_SURFACE('',#16970,20.925);
#1606=CYLINDRICAL_SURFACE('',#16972,20.925);
#1607=CYLINDRICAL_SURFACE('',#16973,20.925);
#1608=CYLINDRICAL_SURFACE('',#16974,20.925);
#1609=CYLINDRICAL_SURFACE('',#16975,20.925);
#1610=CYLINDRICAL_SURFACE('',#16976,20.925);
#1611=CYLINDRICAL_SURFACE('',#16977,20.925);
#1612=CYLINDRICAL_SURFACE('',#16978,20.925);
#1613=CYLINDRICAL_SURFACE('',#16979,20.925);
#1614=CYLINDRICAL_SURFACE('',#16980,20.925);
#1615=CYLINDRICAL_SURFACE('',#16981,20.925);
#1616=CYLINDRICAL_SURFACE('',#16982,20.925);
#1617=CYLINDRICAL_SURFACE('',#16983,20.925);
#1618=CYLINDRICAL_SURFACE('',#16984,20.925);
#1619=CYLINDRICAL_SURFACE('',#16985,20.925);
#1620=CYLINDRICAL_SURFACE('',#16986,20.925);
#1621=CYLINDRICAL_SURFACE('',#16987,20.06595);
#1622=CYLINDRICAL_SURFACE('',#16989,20.06595);
#1623=CYLINDRICAL_SURFACE('',#16990,20.06595);
#1624=CYLINDRICAL_SURFACE('',#16991,20.06595);
#1625=CYLINDRICAL_SURFACE('',#16992,20.06595);
#1626=CYLINDRICAL_SURFACE('',#16993,20.06595);
#1627=CYLINDRICAL_SURFACE('',#16994,20.06595);
#1628=CYLINDRICAL_SURFACE('',#16995,20.06595);
#1629=CYLINDRICAL_SURFACE('',#16996,20.06595);
#1630=CYLINDRICAL_SURFACE('',#16997,20.06595);
#1631=CYLINDRICAL_SURFACE('',#16998,20.06595);
#1632=CYLINDRICAL_SURFACE('',#16999,20.06595);
#1633=CYLINDRICAL_SURFACE('',#17000,20.06595);
#1634=CYLINDRICAL_SURFACE('',#17001,20.06595);
#1635=CYLINDRICAL_SURFACE('',#17002,20.06595);
#1636=CYLINDRICAL_SURFACE('',#17003,16.425);
#1637=CYLINDRICAL_SURFACE('',#17005,16.425);
#1638=CYLINDRICAL_SURFACE('',#17006,16.425);
#1639=CYLINDRICAL_SURFACE('',#17007,16.425);
#1640=CYLINDRICAL_SURFACE('',#17008,16.425);
#1641=CYLINDRICAL_SURFACE('',#17009,16.425);
#1642=CYLINDRICAL_SURFACE('',#17010,16.425);
#1643=CYLINDRICAL_SURFACE('',#17011,16.425);
#1644=CYLINDRICAL_SURFACE('',#17012,16.425);
#1645=CYLINDRICAL_SURFACE('',#17013,16.425);
#1646=CYLINDRICAL_SURFACE('',#17014,16.425);
#1647=CYLINDRICAL_SURFACE('',#17016,15.56595);
#1648=CYLINDRICAL_SURFACE('',#17018,15.56595);
#1649=CYLINDRICAL_SURFACE('',#17019,15.56595);
#1650=CYLINDRICAL_SURFACE('',#17020,15.56595);
#1651=CYLINDRICAL_SURFACE('',#17021,15.56595);
#1652=CYLINDRICAL_SURFACE('',#17022,15.56595);
#1653=CYLINDRICAL_SURFACE('',#17023,15.56595);
#1654=CYLINDRICAL_SURFACE('',#17024,15.56595);
#1655=CYLINDRICAL_SURFACE('',#17025,15.56595);
#1656=CYLINDRICAL_SURFACE('',#17026,15.56595);
#1657=CYLINDRICAL_SURFACE('',#17031,4.);
#1658=CYLINDRICAL_SURFACE('',#17059,15.56595);
#1659=CYLINDRICAL_SURFACE('',#17060,16.425);
#1660=CYLINDRICAL_SURFACE('',#17066,20.06595);
#1661=CYLINDRICAL_SURFACE('',#17067,0.6);
#1662=CYLINDRICAL_SURFACE('',#17068,6.99999999999999);
#1663=CYLINDRICAL_SURFACE('',#17073,0.6);
#1664=CYLINDRICAL_SURFACE('',#17074,0.600000000000005);
#1665=CYLINDRICAL_SURFACE('',#17075,0.600000000000005);
#1666=CYLINDRICAL_SURFACE('',#17081,5.05000000000001);
#1667=CYLINDRICAL_SURFACE('',#17085,4.01);
#1668=CYLINDRICAL_SURFACE('',#17089,13.);
#1669=CYLINDRICAL_SURFACE('',#17090,10.);
#1670=CYLINDRICAL_SURFACE('',#17093,3.05);
#1671=CYLINDRICAL_SURFACE('',#17096,26.);
#1672=CYLINDRICAL_SURFACE('',#17100,18.);
#1673=CYLINDRICAL_SURFACE('',#17105,20.925);
#1674=CYLINDRICAL_SURFACE('',#17112,3.05);
#1675=CYLINDRICAL_SURFACE('',#17120,15.);
#1676=CYLINDRICAL_SURFACE('',#17126,17.96);
#1677=CYLINDRICAL_SURFACE('',#17130,15.05);
#1678=CYLINDRICAL_SURFACE('',#17134,17.96);
#1679=CYLINDRICAL_SURFACE('',#17138,15.05);
#1680=CYLINDRICAL_SURFACE('',#17142,17.96);
#1681=CYLINDRICAL_SURFACE('',#17157,15.06);
#1682=CYLINDRICAL_SURFACE('',#17162,17.97);
#1683=CYLINDRICAL_SURFACE('',#17170,3.);
#1684=CYLINDRICAL_SURFACE('',#17258,3.);
#1685=CYLINDRICAL_SURFACE('',#17262,2.5);
#1686=CYLINDRICAL_SURFACE('',#17266,3.);
#1687=CYLINDRICAL_SURFACE('',#17270,2.5);
#1688=CYLINDRICAL_SURFACE('',#17274,3.);
#1689=CYLINDRICAL_SURFACE('',#17280,11.925);
#1690=CYLINDRICAL_SURFACE('',#17282,11.925);
#1691=CYLINDRICAL_SURFACE('',#17283,11.925);
#1692=CYLINDRICAL_SURFACE('',#17284,11.925);
#1693=CYLINDRICAL_SURFACE('',#17285,11.925);
#1694=CYLINDRICAL_SURFACE('',#17286,11.925);
#1695=CYLINDRICAL_SURFACE('',#17287,11.925);
#1696=CYLINDRICAL_SURFACE('',#17288,11.925);
#1697=CYLINDRICAL_SURFACE('',#17289,11.925);
#1698=CYLINDRICAL_SURFACE('',#17290,11.925);
#1699=CYLINDRICAL_SURFACE('',#17291,11.925);
#1700=CYLINDRICAL_SURFACE('',#17292,11.925);
#1701=CYLINDRICAL_SURFACE('',#17293,11.06595);
#1702=CYLINDRICAL_SURFACE('',#17295,11.06595);
#1703=CYLINDRICAL_SURFACE('',#17296,11.06595);
#1704=CYLINDRICAL_SURFACE('',#17297,11.06595);
#1705=CYLINDRICAL_SURFACE('',#17298,11.06595);
#1706=CYLINDRICAL_SURFACE('',#17299,11.06595);
#1707=CYLINDRICAL_SURFACE('',#17300,11.06595);
#1708=CYLINDRICAL_SURFACE('',#17301,11.06595);
#1709=CYLINDRICAL_SURFACE('',#17302,11.06595);
#1710=CYLINDRICAL_SURFACE('',#17303,11.06595);
#1711=CYLINDRICAL_SURFACE('',#17304,11.06595);
#1712=CYLINDRICAL_SURFACE('',#17317,23.);
#1713=CYLINDRICAL_SURFACE('',#17322,11.06595);
#1714=CYLINDRICAL_SURFACE('',#17323,11.925);
#1715=CYLINDRICAL_SURFACE('',#17325,16.55);
#1716=CYLINDRICAL_SURFACE('',#17335,5.05);
#1717=CYLINDRICAL_SURFACE('',#17339,17.5);
#1718=CYLINDRICAL_SURFACE('',#17343,4.942);
#1719=CYLINDRICAL_SURFACE('',#17345,4.942);
#1720=CYLINDRICAL_SURFACE('',#17346,4.942);
#1721=CYLINDRICAL_SURFACE('',#17347,4.942);
#1722=CYLINDRICAL_SURFACE('',#17348,4.942);
#1723=CYLINDRICAL_SURFACE('',#17349,4.942);
#1724=CYLINDRICAL_SURFACE('',#17350,4.942);
#1725=CYLINDRICAL_SURFACE('',#17351,4.942);
#1726=CYLINDRICAL_SURFACE('',#17352,4.942);
#1727=CYLINDRICAL_SURFACE('',#17353,4.942);
#1728=CYLINDRICAL_SURFACE('',#17354,4.942);
#1729=CYLINDRICAL_SURFACE('',#17355,4.942);
#1730=CYLINDRICAL_SURFACE('',#17356,4.942);
#1731=CYLINDRICAL_SURFACE('',#17357,4.372);
#1732=CYLINDRICAL_SURFACE('',#17359,4.372);
#1733=CYLINDRICAL_SURFACE('',#17361,4.372);
#1734=CYLINDRICAL_SURFACE('',#17362,4.372);
#1735=CYLINDRICAL_SURFACE('',#17363,4.372);
#1736=CYLINDRICAL_SURFACE('',#17364,4.372);
#1737=CYLINDRICAL_SURFACE('',#17365,4.372);
#1738=CYLINDRICAL_SURFACE('',#17366,4.372);
#1739=CYLINDRICAL_SURFACE('',#17367,4.372);
#1740=CYLINDRICAL_SURFACE('',#17368,4.372);
#1741=CYLINDRICAL_SURFACE('',#17369,4.372);
#1742=CYLINDRICAL_SURFACE('',#17370,4.372);
#1743=CYLINDRICAL_SURFACE('',#17371,4.372);
#1744=CYLINDRICAL_SURFACE('',#17380,7.);
#1745=CYLINDRICAL_SURFACE('',#17444,4.372);
#1746=CYLINDRICAL_SURFACE('',#17545,4.942);
#1747=CYLINDRICAL_SURFACE('',#17556,9.5);
#1748=CYLINDRICAL_SURFACE('',#17560,12.05);
#1749=CYLINDRICAL_SURFACE('',#17566,13.);
#1750=CYLINDRICAL_SURFACE('',#17590,15.);
#1751=CYLINDRICAL_SURFACE('',#17592,13.);
#1752=CYLINDRICAL_SURFACE('',#17602,4.942);
#1753=CYLINDRICAL_SURFACE('',#17604,4.942);
#1754=CYLINDRICAL_SURFACE('',#17605,4.942);
#1755=CYLINDRICAL_SURFACE('',#17606,4.942);
#1756=CYLINDRICAL_SURFACE('',#17607,4.942);
#1757=CYLINDRICAL_SURFACE('',#17608,4.942);
#1758=CYLINDRICAL_SURFACE('',#17609,4.942);
#1759=CYLINDRICAL_SURFACE('',#17610,4.942);
#1760=CYLINDRICAL_SURFACE('',#17611,4.942);
#1761=CYLINDRICAL_SURFACE('',#17612,4.942);
#1762=CYLINDRICAL_SURFACE('',#17613,4.942);
#1763=CYLINDRICAL_SURFACE('',#17614,4.942);
#1764=CYLINDRICAL_SURFACE('',#17615,4.942);
#1765=CYLINDRICAL_SURFACE('',#17616,4.372);
#1766=CYLINDRICAL_SURFACE('',#17618,4.372);
#1767=CYLINDRICAL_SURFACE('',#17619,4.372);
#1768=CYLINDRICAL_SURFACE('',#17620,4.372);
#1769=CYLINDRICAL_SURFACE('',#17621,4.372);
#1770=CYLINDRICAL_SURFACE('',#17622,4.372);
#1771=CYLINDRICAL_SURFACE('',#17623,4.372);
#1772=CYLINDRICAL_SURFACE('',#17624,4.372);
#1773=CYLINDRICAL_SURFACE('',#17625,4.372);
#1774=CYLINDRICAL_SURFACE('',#17626,4.372);
#1775=CYLINDRICAL_SURFACE('',#17627,4.372);
#1776=CYLINDRICAL_SURFACE('',#17628,4.372);
#1777=CYLINDRICAL_SURFACE('',#17633,4.372);
#1778=CYLINDRICAL_SURFACE('',#17675,3.6);
#1779=CYLINDRICAL_SURFACE('',#17677,3.);
#1780=CYLINDRICAL_SURFACE('',#17867,4.942);
#1781=CYLINDRICAL_SURFACE('',#17868,4.);
#1782=CYLINDRICAL_SURFACE('',#17874,13.);
#1783=CYLINDRICAL_SURFACE('',#17903,9.);
#1784=CYLINDRICAL_SURFACE('',#17913,1.);
#1785=CYLINDRICAL_SURFACE('',#17917,1.);
#1786=CYLINDRICAL_SURFACE('',#17924,1.);
#1787=CYLINDRICAL_SURFACE('',#17926,1.);
#1788=CYLINDRICAL_SURFACE('',#17928,1.);
#1789=CYLINDRICAL_SURFACE('',#17929,1.);
#1790=CYLINDRICAL_SURFACE('',#17936,1.);
#1791=CYLINDRICAL_SURFACE('',#17941,1.);
#1792=CYLINDRICAL_SURFACE('',#17943,9.);
#1793=CYLINDRICAL_SURFACE('',#17944,3.05);
#1794=CYLINDRICAL_SURFACE('',#17945,3.05);
#1795=CYLINDRICAL_SURFACE('',#17946,3.05);
#1796=CYLINDRICAL_SURFACE('',#17947,3.05);
#1797=CYLINDRICAL_SURFACE('',#17948,8.);
#1798=CYLINDRICAL_SURFACE('',#17964,11.);
#1799=CYLINDRICAL_SURFACE('',#17975,11.);
#1800=CYLINDRICAL_SURFACE('',#17984,8.);
#1801=CYLINDRICAL_SURFACE('',#17997,6.);
#1802=CYLINDRICAL_SURFACE('',#18024,3.05);
#1803=CYLINDRICAL_SURFACE('',#18025,3.05);
#1804=CYLINDRICAL_SURFACE('',#18026,6.);
#1805=CYLINDRICAL_SURFACE('',#18033,3.);
#1806=CYLINDRICAL_SURFACE('',#18037,2.5);
#1807=CYLINDRICAL_SURFACE('',#18041,3.);
#1808=CYLINDRICAL_SURFACE('',#18045,2.5);
#1809=CYLINDRICAL_SURFACE('',#18049,3.);
#1810=CYLINDRICAL_SURFACE('',#18062,5.5);
#1811=CYLINDRICAL_SURFACE('',#18074,3.05);
#1812=CYLINDRICAL_SURFACE('',#18081,3.99);
#1813=CYLINDRICAL_SURFACE('',#18083,5.5);
#1814=CYLINDRICAL_SURFACE('',#18087,2.5);
#1815=FACE_OUTER_BOUND('',#2789,.T.);
#1816=FACE_OUTER_BOUND('',#2790,.T.);
#1817=FACE_OUTER_BOUND('',#2791,.T.);
#1818=FACE_OUTER_BOUND('',#2793,.T.);
#1819=FACE_OUTER_BOUND('',#2794,.T.);
#1820=FACE_OUTER_BOUND('',#2796,.T.);
#1821=FACE_OUTER_BOUND('',#2797,.T.);
#1822=FACE_OUTER_BOUND('',#2798,.T.);
#1823=FACE_OUTER_BOUND('',#2799,.T.);
#1824=FACE_OUTER_BOUND('',#2800,.T.);
#1825=FACE_OUTER_BOUND('',#2801,.T.);
#1826=FACE_OUTER_BOUND('',#2802,.T.);
#1827=FACE_OUTER_BOUND('',#2803,.T.);
#1828=FACE_OUTER_BOUND('',#2804,.T.);
#1829=FACE_OUTER_BOUND('',#2805,.T.);
#1830=FACE_OUTER_BOUND('',#2806,.T.);
#1831=FACE_OUTER_BOUND('',#2807,.T.);
#1832=FACE_OUTER_BOUND('',#2808,.T.);
#1833=FACE_OUTER_BOUND('',#2809,.T.);
#1834=FACE_OUTER_BOUND('',#2810,.T.);
#1835=FACE_OUTER_BOUND('',#2811,.T.);
#1836=FACE_OUTER_BOUND('',#2812,.T.);
#1837=FACE_OUTER_BOUND('',#2813,.T.);
#1838=FACE_OUTER_BOUND('',#2814,.T.);
#1839=FACE_OUTER_BOUND('',#2815,.T.);
#1840=FACE_OUTER_BOUND('',#2816,.T.);
#1841=FACE_OUTER_BOUND('',#2817,.T.);
#1842=FACE_OUTER_BOUND('',#2818,.T.);
#1843=FACE_OUTER_BOUND('',#2819,.T.);
#1844=FACE_OUTER_BOUND('',#2820,.T.);
#1845=FACE_OUTER_BOUND('',#2821,.T.);
#1846=FACE_OUTER_BOUND('',#2822,.T.);
#1847=FACE_OUTER_BOUND('',#2823,.T.);
#1848=FACE_OUTER_BOUND('',#2824,.T.);
#1849=FACE_OUTER_BOUND('',#2825,.T.);
#1850=FACE_OUTER_BOUND('',#2826,.T.);
#1851=FACE_OUTER_BOUND('',#2827,.T.);
#1852=FACE_OUTER_BOUND('',#2828,.T.);
#1853=FACE_OUTER_BOUND('',#2829,.T.);
#1854=FACE_OUTER_BOUND('',#2830,.T.);
#1855=FACE_OUTER_BOUND('',#2831,.T.);
#1856=FACE_OUTER_BOUND('',#2832,.T.);
#1857=FACE_OUTER_BOUND('',#2833,.T.);
#1858=FACE_OUTER_BOUND('',#2834,.T.);
#1859=FACE_OUTER_BOUND('',#2835,.T.);
#1860=FACE_OUTER_BOUND('',#2836,.T.);
#1861=FACE_OUTER_BOUND('',#2837,.T.);
#1862=FACE_OUTER_BOUND('',#2838,.T.);
#1863=FACE_OUTER_BOUND('',#2839,.T.);
#1864=FACE_OUTER_BOUND('',#2840,.T.);
#1865=FACE_OUTER_BOUND('',#2841,.T.);
#1866=FACE_OUTER_BOUND('',#2842,.T.);
#1867=FACE_OUTER_BOUND('',#2843,.T.);
#1868=FACE_OUTER_BOUND('',#2844,.T.);
#1869=FACE_OUTER_BOUND('',#2845,.T.);
#1870=FACE_OUTER_BOUND('',#2846,.T.);
#1871=FACE_OUTER_BOUND('',#2851,.T.);
#1872=FACE_OUTER_BOUND('',#2852,.T.);
#1873=FACE_OUTER_BOUND('',#2853,.T.);
#1874=FACE_OUTER_BOUND('',#2854,.T.);
#1875=FACE_OUTER_BOUND('',#2855,.T.);
#1876=FACE_OUTER_BOUND('',#2856,.T.);
#1877=FACE_OUTER_BOUND('',#2857,.T.);
#1878=FACE_OUTER_BOUND('',#2858,.T.);
#1879=FACE_OUTER_BOUND('',#2859,.T.);
#1880=FACE_OUTER_BOUND('',#2860,.T.);
#1881=FACE_OUTER_BOUND('',#2861,.T.);
#1882=FACE_OUTER_BOUND('',#2862,.T.);
#1883=FACE_OUTER_BOUND('',#2863,.T.);
#1884=FACE_OUTER_BOUND('',#2864,.T.);
#1885=FACE_OUTER_BOUND('',#2865,.T.);
#1886=FACE_OUTER_BOUND('',#2866,.T.);
#1887=FACE_OUTER_BOUND('',#2867,.T.);
#1888=FACE_OUTER_BOUND('',#2868,.T.);
#1889=FACE_OUTER_BOUND('',#2869,.T.);
#1890=FACE_OUTER_BOUND('',#2870,.T.);
#1891=FACE_OUTER_BOUND('',#2871,.T.);
#1892=FACE_OUTER_BOUND('',#2872,.T.);
#1893=FACE_OUTER_BOUND('',#2873,.T.);
#1894=FACE_OUTER_BOUND('',#2874,.T.);
#1895=FACE_OUTER_BOUND('',#2875,.T.);
#1896=FACE_OUTER_BOUND('',#2876,.T.);
#1897=FACE_OUTER_BOUND('',#2878,.T.);
#1898=FACE_OUTER_BOUND('',#2879,.T.);
#1899=FACE_OUTER_BOUND('',#2880,.T.);
#1900=FACE_OUTER_BOUND('',#2881,.T.);
#1901=FACE_OUTER_BOUND('',#2882,.T.);
#1902=FACE_OUTER_BOUND('',#2883,.T.);
#1903=FACE_OUTER_BOUND('',#2884,.T.);
#1904=FACE_OUTER_BOUND('',#2885,.T.);
#1905=FACE_OUTER_BOUND('',#2886,.T.);
#1906=FACE_OUTER_BOUND('',#2887,.T.);
#1907=FACE_OUTER_BOUND('',#2888,.T.);
#1908=FACE_OUTER_BOUND('',#2889,.T.);
#1909=FACE_OUTER_BOUND('',#2890,.T.);
#1910=FACE_OUTER_BOUND('',#2891,.T.);
#1911=FACE_OUTER_BOUND('',#2893,.T.);
#1912=FACE_OUTER_BOUND('',#2894,.T.);
#1913=FACE_OUTER_BOUND('',#2895,.T.);
#1914=FACE_OUTER_BOUND('',#2896,.T.);
#1915=FACE_OUTER_BOUND('',#2897,.T.);
#1916=FACE_OUTER_BOUND('',#2898,.T.);
#1917=FACE_OUTER_BOUND('',#2899,.T.);
#1918=FACE_OUTER_BOUND('',#2900,.T.);
#1919=FACE_OUTER_BOUND('',#2901,.T.);
#1920=FACE_OUTER_BOUND('',#2902,.T.);
#1921=FACE_OUTER_BOUND('',#2903,.T.);
#1922=FACE_OUTER_BOUND('',#2904,.T.);
#1923=FACE_OUTER_BOUND('',#2905,.T.);
#1924=FACE_OUTER_BOUND('',#2906,.T.);
#1925=FACE_OUTER_BOUND('',#2907,.T.);
#1926=FACE_OUTER_BOUND('',#2908,.T.);
#1927=FACE_OUTER_BOUND('',#2909,.T.);
#1928=FACE_OUTER_BOUND('',#2910,.T.);
#1929=FACE_OUTER_BOUND('',#2911,.T.);
#1930=FACE_OUTER_BOUND('',#2912,.T.);
#1931=FACE_OUTER_BOUND('',#2913,.T.);
#1932=FACE_OUTER_BOUND('',#2914,.T.);
#1933=FACE_OUTER_BOUND('',#2915,.T.);
#1934=FACE_OUTER_BOUND('',#2916,.T.);
#1935=FACE_OUTER_BOUND('',#2917,.T.);
#1936=FACE_OUTER_BOUND('',#2918,.T.);
#1937=FACE_OUTER_BOUND('',#2919,.T.);
#1938=FACE_OUTER_BOUND('',#2920,.T.);
#1939=FACE_OUTER_BOUND('',#2921,.T.);
#1940=FACE_OUTER_BOUND('',#2922,.T.);
#1941=FACE_OUTER_BOUND('',#2923,.T.);
#1942=FACE_OUTER_BOUND('',#2924,.T.);
#1943=FACE_OUTER_BOUND('',#2925,.T.);
#1944=FACE_OUTER_BOUND('',#2926,.T.);
#1945=FACE_OUTER_BOUND('',#2927,.T.);
#1946=FACE_OUTER_BOUND('',#2928,.T.);
#1947=FACE_OUTER_BOUND('',#2929,.T.);
#1948=FACE_OUTER_BOUND('',#2930,.T.);
#1949=FACE_OUTER_BOUND('',#2931,.T.);
#1950=FACE_OUTER_BOUND('',#2932,.T.);
#1951=FACE_OUTER_BOUND('',#2933,.T.);
#1952=FACE_OUTER_BOUND('',#2934,.T.);
#1953=FACE_OUTER_BOUND('',#2935,.T.);
#1954=FACE_OUTER_BOUND('',#2936,.T.);
#1955=FACE_OUTER_BOUND('',#2937,.T.);
#1956=FACE_OUTER_BOUND('',#2938,.T.);
#1957=FACE_OUTER_BOUND('',#2939,.T.);
#1958=FACE_OUTER_BOUND('',#2940,.T.);
#1959=FACE_OUTER_BOUND('',#2941,.T.);
#1960=FACE_OUTER_BOUND('',#2942,.T.);
#1961=FACE_OUTER_BOUND('',#2943,.T.);
#1962=FACE_OUTER_BOUND('',#2944,.T.);
#1963=FACE_OUTER_BOUND('',#2945,.T.);
#1964=FACE_OUTER_BOUND('',#2946,.T.);
#1965=FACE_OUTER_BOUND('',#2947,.T.);
#1966=FACE_OUTER_BOUND('',#2948,.T.);
#1967=FACE_OUTER_BOUND('',#2949,.T.);
#1968=FACE_OUTER_BOUND('',#2950,.T.);
#1969=FACE_OUTER_BOUND('',#2951,.T.);
#1970=FACE_OUTER_BOUND('',#2952,.T.);
#1971=FACE_OUTER_BOUND('',#2953,.T.);
#1972=FACE_OUTER_BOUND('',#2954,.T.);
#1973=FACE_OUTER_BOUND('',#2955,.T.);
#1974=FACE_OUTER_BOUND('',#2956,.T.);
#1975=FACE_OUTER_BOUND('',#2957,.T.);
#1976=FACE_OUTER_BOUND('',#2958,.T.);
#1977=FACE_OUTER_BOUND('',#2959,.T.);
#1978=FACE_OUTER_BOUND('',#2960,.T.);
#1979=FACE_OUTER_BOUND('',#2961,.T.);
#1980=FACE_OUTER_BOUND('',#2962,.T.);
#1981=FACE_OUTER_BOUND('',#2963,.T.);
#1982=FACE_OUTER_BOUND('',#2964,.T.);
#1983=FACE_OUTER_BOUND('',#2965,.T.);
#1984=FACE_OUTER_BOUND('',#2966,.T.);
#1985=FACE_OUTER_BOUND('',#2967,.T.);
#1986=FACE_OUTER_BOUND('',#2968,.T.);
#1987=FACE_OUTER_BOUND('',#2969,.T.);
#1988=FACE_OUTER_BOUND('',#2970,.T.);
#1989=FACE_OUTER_BOUND('',#2971,.T.);
#1990=FACE_OUTER_BOUND('',#2972,.T.);
#1991=FACE_OUTER_BOUND('',#2973,.T.);
#1992=FACE_OUTER_BOUND('',#2974,.T.);
#1993=FACE_OUTER_BOUND('',#2975,.T.);
#1994=FACE_OUTER_BOUND('',#2976,.T.);
#1995=FACE_OUTER_BOUND('',#2977,.T.);
#1996=FACE_OUTER_BOUND('',#2978,.T.);
#1997=FACE_OUTER_BOUND('',#2979,.T.);
#1998=FACE_OUTER_BOUND('',#2980,.T.);
#1999=FACE_OUTER_BOUND('',#2981,.T.);
#2000=FACE_OUTER_BOUND('',#2982,.T.);
#2001=FACE_OUTER_BOUND('',#2983,.T.);
#2002=FACE_OUTER_BOUND('',#2984,.T.);
#2003=FACE_OUTER_BOUND('',#2985,.T.);
#2004=FACE_OUTER_BOUND('',#2986,.T.);
#2005=FACE_OUTER_BOUND('',#2987,.T.);
#2006=FACE_OUTER_BOUND('',#2988,.T.);
#2007=FACE_OUTER_BOUND('',#2989,.T.);
#2008=FACE_OUTER_BOUND('',#2990,.T.);
#2009=FACE_OUTER_BOUND('',#2991,.T.);
#2010=FACE_OUTER_BOUND('',#2992,.T.);
#2011=FACE_OUTER_BOUND('',#2993,.T.);
#2012=FACE_OUTER_BOUND('',#2994,.T.);
#2013=FACE_OUTER_BOUND('',#2995,.T.);
#2014=FACE_OUTER_BOUND('',#2996,.T.);
#2015=FACE_OUTER_BOUND('',#2997,.T.);
#2016=FACE_OUTER_BOUND('',#2998,.T.);
#2017=FACE_OUTER_BOUND('',#2999,.T.);
#2018=FACE_OUTER_BOUND('',#3000,.T.);
#2019=FACE_OUTER_BOUND('',#3001,.T.);
#2020=FACE_OUTER_BOUND('',#3002,.T.);
#2021=FACE_OUTER_BOUND('',#3003,.T.);
#2022=FACE_OUTER_BOUND('',#3004,.T.);
#2023=FACE_OUTER_BOUND('',#3005,.T.);
#2024=FACE_OUTER_BOUND('',#3006,.T.);
#2025=FACE_OUTER_BOUND('',#3008,.T.);
#2026=FACE_OUTER_BOUND('',#3009,.T.);
#2027=FACE_OUTER_BOUND('',#3011,.T.);
#2028=FACE_OUTER_BOUND('',#3012,.T.);
#2029=FACE_OUTER_BOUND('',#3013,.T.);
#2030=FACE_OUTER_BOUND('',#3015,.T.);
#2031=FACE_OUTER_BOUND('',#3016,.T.);
#2032=FACE_OUTER_BOUND('',#3017,.T.);
#2033=FACE_OUTER_BOUND('',#3018,.T.);
#2034=FACE_OUTER_BOUND('',#3020,.T.);
#2035=FACE_OUTER_BOUND('',#3021,.T.);
#2036=FACE_OUTER_BOUND('',#3022,.T.);
#2037=FACE_OUTER_BOUND('',#3023,.T.);
#2038=FACE_OUTER_BOUND('',#3024,.T.);
#2039=FACE_OUTER_BOUND('',#3025,.T.);
#2040=FACE_OUTER_BOUND('',#3026,.T.);
#2041=FACE_OUTER_BOUND('',#3027,.T.);
#2042=FACE_OUTER_BOUND('',#3028,.T.);
#2043=FACE_OUTER_BOUND('',#3029,.T.);
#2044=FACE_OUTER_BOUND('',#3030,.T.);
#2045=FACE_OUTER_BOUND('',#3031,.T.);
#2046=FACE_OUTER_BOUND('',#3032,.T.);
#2047=FACE_OUTER_BOUND('',#3033,.T.);
#2048=FACE_OUTER_BOUND('',#3034,.T.);
#2049=FACE_OUTER_BOUND('',#3035,.T.);
#2050=FACE_OUTER_BOUND('',#3036,.T.);
#2051=FACE_OUTER_BOUND('',#3038,.T.);
#2052=FACE_OUTER_BOUND('',#3039,.T.);
#2053=FACE_OUTER_BOUND('',#3040,.T.);
#2054=FACE_OUTER_BOUND('',#3041,.T.);
#2055=FACE_OUTER_BOUND('',#3042,.T.);
#2056=FACE_OUTER_BOUND('',#3043,.T.);
#2057=FACE_OUTER_BOUND('',#3044,.T.);
#2058=FACE_OUTER_BOUND('',#3045,.T.);
#2059=FACE_OUTER_BOUND('',#3046,.T.);
#2060=FACE_OUTER_BOUND('',#3047,.T.);
#2061=FACE_OUTER_BOUND('',#3049,.T.);
#2062=FACE_OUTER_BOUND('',#3051,.T.);
#2063=FACE_OUTER_BOUND('',#3053,.T.);
#2064=FACE_OUTER_BOUND('',#3054,.T.);
#2065=FACE_OUTER_BOUND('',#3056,.T.);
#2066=FACE_OUTER_BOUND('',#3057,.T.);
#2067=FACE_OUTER_BOUND('',#3058,.T.);
#2068=FACE_OUTER_BOUND('',#3060,.T.);
#2069=FACE_OUTER_BOUND('',#3061,.T.);
#2070=FACE_OUTER_BOUND('',#3062,.T.);
#2071=FACE_OUTER_BOUND('',#3063,.T.);
#2072=FACE_OUTER_BOUND('',#3064,.T.);
#2073=FACE_OUTER_BOUND('',#3066,.T.);
#2074=FACE_OUTER_BOUND('',#3067,.T.);
#2075=FACE_OUTER_BOUND('',#3068,.T.);
#2076=FACE_OUTER_BOUND('',#3070,.T.);
#2077=FACE_OUTER_BOUND('',#3071,.T.);
#2078=FACE_OUTER_BOUND('',#3072,.T.);
#2079=FACE_OUTER_BOUND('',#3074,.T.);
#2080=FACE_OUTER_BOUND('',#3075,.T.);
#2081=FACE_OUTER_BOUND('',#3077,.T.);
#2082=FACE_OUTER_BOUND('',#3078,.T.);
#2083=FACE_OUTER_BOUND('',#3080,.T.);
#2084=FACE_OUTER_BOUND('',#3081,.T.);
#2085=FACE_OUTER_BOUND('',#3083,.T.);
#2086=FACE_OUTER_BOUND('',#3084,.T.);
#2087=FACE_OUTER_BOUND('',#3085,.T.);
#2088=FACE_OUTER_BOUND('',#3086,.T.);
#2089=FACE_OUTER_BOUND('',#3087,.T.);
#2090=FACE_OUTER_BOUND('',#3088,.T.);
#2091=FACE_OUTER_BOUND('',#3089,.T.);
#2092=FACE_OUTER_BOUND('',#3090,.T.);
#2093=FACE_OUTER_BOUND('',#3091,.T.);
#2094=FACE_OUTER_BOUND('',#3093,.T.);
#2095=FACE_OUTER_BOUND('',#3094,.T.);
#2096=FACE_OUTER_BOUND('',#3096,.T.);
#2097=FACE_OUTER_BOUND('',#3097,.T.);
#2098=FACE_OUTER_BOUND('',#3098,.T.);
#2099=FACE_OUTER_BOUND('',#3099,.T.);
#2100=FACE_OUTER_BOUND('',#3100,.T.);
#2101=FACE_OUTER_BOUND('',#3101,.T.);
#2102=FACE_OUTER_BOUND('',#3102,.T.);
#2103=FACE_OUTER_BOUND('',#3103,.T.);
#2104=FACE_OUTER_BOUND('',#3104,.T.);
#2105=FACE_OUTER_BOUND('',#3105,.T.);
#2106=FACE_OUTER_BOUND('',#3106,.T.);
#2107=FACE_OUTER_BOUND('',#3107,.T.);
#2108=FACE_OUTER_BOUND('',#3108,.T.);
#2109=FACE_OUTER_BOUND('',#3109,.T.);
#2110=FACE_OUTER_BOUND('',#3110,.T.);
#2111=FACE_OUTER_BOUND('',#3111,.T.);
#2112=FACE_OUTER_BOUND('',#3112,.T.);
#2113=FACE_OUTER_BOUND('',#3113,.T.);
#2114=FACE_OUTER_BOUND('',#3114,.T.);
#2115=FACE_OUTER_BOUND('',#3115,.T.);
#2116=FACE_OUTER_BOUND('',#3116,.T.);
#2117=FACE_OUTER_BOUND('',#3117,.T.);
#2118=FACE_OUTER_BOUND('',#3118,.T.);
#2119=FACE_OUTER_BOUND('',#3119,.T.);
#2120=FACE_OUTER_BOUND('',#3120,.T.);
#2121=FACE_OUTER_BOUND('',#3121,.T.);
#2122=FACE_OUTER_BOUND('',#3122,.T.);
#2123=FACE_OUTER_BOUND('',#3123,.T.);
#2124=FACE_OUTER_BOUND('',#3124,.T.);
#2125=FACE_OUTER_BOUND('',#3125,.T.);
#2126=FACE_OUTER_BOUND('',#3126,.T.);
#2127=FACE_OUTER_BOUND('',#3132,.T.);
#2128=FACE_OUTER_BOUND('',#3133,.T.);
#2129=FACE_OUTER_BOUND('',#3134,.T.);
#2130=FACE_OUTER_BOUND('',#3135,.T.);
#2131=FACE_OUTER_BOUND('',#3136,.T.);
#2132=FACE_OUTER_BOUND('',#3137,.T.);
#2133=FACE_OUTER_BOUND('',#3138,.T.);
#2134=FACE_OUTER_BOUND('',#3139,.T.);
#2135=FACE_OUTER_BOUND('',#3140,.T.);
#2136=FACE_OUTER_BOUND('',#3141,.T.);
#2137=FACE_OUTER_BOUND('',#3142,.T.);
#2138=FACE_OUTER_BOUND('',#3143,.T.);
#2139=FACE_OUTER_BOUND('',#3144,.T.);
#2140=FACE_OUTER_BOUND('',#3145,.T.);
#2141=FACE_OUTER_BOUND('',#3146,.T.);
#2142=FACE_OUTER_BOUND('',#3147,.T.);
#2143=FACE_OUTER_BOUND('',#3148,.T.);
#2144=FACE_OUTER_BOUND('',#3149,.T.);
#2145=FACE_OUTER_BOUND('',#3150,.T.);
#2146=FACE_OUTER_BOUND('',#3151,.T.);
#2147=FACE_OUTER_BOUND('',#3152,.T.);
#2148=FACE_OUTER_BOUND('',#3153,.T.);
#2149=FACE_OUTER_BOUND('',#3154,.T.);
#2150=FACE_OUTER_BOUND('',#3155,.T.);
#2151=FACE_OUTER_BOUND('',#3156,.T.);
#2152=FACE_OUTER_BOUND('',#3157,.T.);
#2153=FACE_OUTER_BOUND('',#3158,.T.);
#2154=FACE_OUTER_BOUND('',#3159,.T.);
#2155=FACE_OUTER_BOUND('',#3160,.T.);
#2156=FACE_OUTER_BOUND('',#3161,.T.);
#2157=FACE_OUTER_BOUND('',#3162,.T.);
#2158=FACE_OUTER_BOUND('',#3163,.T.);
#2159=FACE_OUTER_BOUND('',#3164,.T.);
#2160=FACE_OUTER_BOUND('',#3165,.T.);
#2161=FACE_OUTER_BOUND('',#3166,.T.);
#2162=FACE_OUTER_BOUND('',#3167,.T.);
#2163=FACE_OUTER_BOUND('',#3168,.T.);
#2164=FACE_OUTER_BOUND('',#3169,.T.);
#2165=FACE_OUTER_BOUND('',#3170,.T.);
#2166=FACE_OUTER_BOUND('',#3171,.T.);
#2167=FACE_OUTER_BOUND('',#3172,.T.);
#2168=FACE_OUTER_BOUND('',#3173,.T.);
#2169=FACE_OUTER_BOUND('',#3174,.T.);
#2170=FACE_OUTER_BOUND('',#3175,.T.);
#2171=FACE_OUTER_BOUND('',#3176,.T.);
#2172=FACE_OUTER_BOUND('',#3177,.T.);
#2173=FACE_OUTER_BOUND('',#3178,.T.);
#2174=FACE_OUTER_BOUND('',#3179,.T.);
#2175=FACE_OUTER_BOUND('',#3180,.T.);
#2176=FACE_OUTER_BOUND('',#3181,.T.);
#2177=FACE_OUTER_BOUND('',#3182,.T.);
#2178=FACE_OUTER_BOUND('',#3183,.T.);
#2179=FACE_OUTER_BOUND('',#3184,.T.);
#2180=FACE_OUTER_BOUND('',#3185,.T.);
#2181=FACE_OUTER_BOUND('',#3186,.T.);
#2182=FACE_OUTER_BOUND('',#3187,.T.);
#2183=FACE_OUTER_BOUND('',#3188,.T.);
#2184=FACE_OUTER_BOUND('',#3189,.T.);
#2185=FACE_OUTER_BOUND('',#3190,.T.);
#2186=FACE_OUTER_BOUND('',#3191,.T.);
#2187=FACE_OUTER_BOUND('',#3192,.T.);
#2188=FACE_OUTER_BOUND('',#3193,.T.);
#2189=FACE_OUTER_BOUND('',#3194,.T.);
#2190=FACE_OUTER_BOUND('',#3195,.T.);
#2191=FACE_OUTER_BOUND('',#3196,.T.);
#2192=FACE_OUTER_BOUND('',#3197,.T.);
#2193=FACE_OUTER_BOUND('',#3198,.T.);
#2194=FACE_OUTER_BOUND('',#3199,.T.);
#2195=FACE_OUTER_BOUND('',#3200,.T.);
#2196=FACE_OUTER_BOUND('',#3201,.T.);
#2197=FACE_OUTER_BOUND('',#3202,.T.);
#2198=FACE_OUTER_BOUND('',#3203,.T.);
#2199=FACE_OUTER_BOUND('',#3204,.T.);
#2200=FACE_OUTER_BOUND('',#3205,.T.);
#2201=FACE_OUTER_BOUND('',#3206,.T.);
#2202=FACE_OUTER_BOUND('',#3207,.T.);
#2203=FACE_OUTER_BOUND('',#3208,.T.);
#2204=FACE_OUTER_BOUND('',#3209,.T.);
#2205=FACE_OUTER_BOUND('',#3210,.T.);
#2206=FACE_OUTER_BOUND('',#3211,.T.);
#2207=FACE_OUTER_BOUND('',#3212,.T.);
#2208=FACE_OUTER_BOUND('',#3213,.T.);
#2209=FACE_OUTER_BOUND('',#3214,.T.);
#2210=FACE_OUTER_BOUND('',#3215,.T.);
#2211=FACE_OUTER_BOUND('',#3216,.T.);
#2212=FACE_OUTER_BOUND('',#3217,.T.);
#2213=FACE_OUTER_BOUND('',#3218,.T.);
#2214=FACE_OUTER_BOUND('',#3219,.T.);
#2215=FACE_OUTER_BOUND('',#3220,.T.);
#2216=FACE_OUTER_BOUND('',#3221,.T.);
#2217=FACE_OUTER_BOUND('',#3222,.T.);
#2218=FACE_OUTER_BOUND('',#3223,.T.);
#2219=FACE_OUTER_BOUND('',#3224,.T.);
#2220=FACE_OUTER_BOUND('',#3225,.T.);
#2221=FACE_OUTER_BOUND('',#3226,.T.);
#2222=FACE_OUTER_BOUND('',#3227,.T.);
#2223=FACE_OUTER_BOUND('',#3228,.T.);
#2224=FACE_OUTER_BOUND('',#3229,.T.);
#2225=FACE_OUTER_BOUND('',#3230,.T.);
#2226=FACE_OUTER_BOUND('',#3231,.T.);
#2227=FACE_OUTER_BOUND('',#3233,.T.);
#2228=FACE_OUTER_BOUND('',#3234,.T.);
#2229=FACE_OUTER_BOUND('',#3236,.T.);
#2230=FACE_OUTER_BOUND('',#3237,.T.);
#2231=FACE_OUTER_BOUND('',#3239,.T.);
#2232=FACE_OUTER_BOUND('',#3240,.T.);
#2233=FACE_OUTER_BOUND('',#3242,.T.);
#2234=FACE_OUTER_BOUND('',#3243,.T.);
#2235=FACE_OUTER_BOUND('',#3244,.T.);
#2236=FACE_OUTER_BOUND('',#3245,.T.);
#2237=FACE_OUTER_BOUND('',#3246,.T.);
#2238=FACE_OUTER_BOUND('',#3247,.T.);
#2239=FACE_OUTER_BOUND('',#3248,.T.);
#2240=FACE_OUTER_BOUND('',#3249,.T.);
#2241=FACE_OUTER_BOUND('',#3250,.T.);
#2242=FACE_OUTER_BOUND('',#3251,.T.);
#2243=FACE_OUTER_BOUND('',#3252,.T.);
#2244=FACE_OUTER_BOUND('',#3253,.T.);
#2245=FACE_OUTER_BOUND('',#3254,.T.);
#2246=FACE_OUTER_BOUND('',#3255,.T.);
#2247=FACE_OUTER_BOUND('',#3256,.T.);
#2248=FACE_OUTER_BOUND('',#3257,.T.);
#2249=FACE_OUTER_BOUND('',#3258,.T.);
#2250=FACE_OUTER_BOUND('',#3259,.T.);
#2251=FACE_OUTER_BOUND('',#3260,.T.);
#2252=FACE_OUTER_BOUND('',#3261,.T.);
#2253=FACE_OUTER_BOUND('',#3262,.T.);
#2254=FACE_OUTER_BOUND('',#3263,.T.);
#2255=FACE_OUTER_BOUND('',#3264,.T.);
#2256=FACE_OUTER_BOUND('',#3265,.T.);
#2257=FACE_OUTER_BOUND('',#3266,.T.);
#2258=FACE_OUTER_BOUND('',#3267,.T.);
#2259=FACE_OUTER_BOUND('',#3268,.T.);
#2260=FACE_OUTER_BOUND('',#3269,.T.);
#2261=FACE_OUTER_BOUND('',#3270,.T.);
#2262=FACE_OUTER_BOUND('',#3272,.T.);
#2263=FACE_OUTER_BOUND('',#3273,.T.);
#2264=FACE_OUTER_BOUND('',#3274,.T.);
#2265=FACE_OUTER_BOUND('',#3275,.T.);
#2266=FACE_OUTER_BOUND('',#3276,.T.);
#2267=FACE_OUTER_BOUND('',#3277,.T.);
#2268=FACE_OUTER_BOUND('',#3278,.T.);
#2269=FACE_OUTER_BOUND('',#3279,.T.);
#2270=FACE_OUTER_BOUND('',#3280,.T.);
#2271=FACE_OUTER_BOUND('',#3282,.T.);
#2272=FACE_OUTER_BOUND('',#3283,.T.);
#2273=FACE_OUTER_BOUND('',#3284,.T.);
#2274=FACE_OUTER_BOUND('',#3286,.T.);
#2275=FACE_OUTER_BOUND('',#3287,.T.);
#2276=FACE_OUTER_BOUND('',#3289,.T.);
#2277=FACE_OUTER_BOUND('',#3290,.T.);
#2278=FACE_OUTER_BOUND('',#3292,.T.);
#2279=FACE_OUTER_BOUND('',#3293,.T.);
#2280=FACE_OUTER_BOUND('',#3294,.T.);
#2281=FACE_OUTER_BOUND('',#3295,.T.);
#2282=FACE_OUTER_BOUND('',#3296,.T.);
#2283=FACE_OUTER_BOUND('',#3297,.T.);
#2284=FACE_OUTER_BOUND('',#3298,.T.);
#2285=FACE_OUTER_BOUND('',#3299,.T.);
#2286=FACE_OUTER_BOUND('',#3300,.T.);
#2287=FACE_OUTER_BOUND('',#3301,.T.);
#2288=FACE_OUTER_BOUND('',#3302,.T.);
#2289=FACE_OUTER_BOUND('',#3303,.T.);
#2290=FACE_OUTER_BOUND('',#3304,.T.);
#2291=FACE_OUTER_BOUND('',#3305,.T.);
#2292=FACE_OUTER_BOUND('',#3306,.T.);
#2293=FACE_OUTER_BOUND('',#3307,.T.);
#2294=FACE_OUTER_BOUND('',#3308,.T.);
#2295=FACE_OUTER_BOUND('',#3309,.T.);
#2296=FACE_OUTER_BOUND('',#3310,.T.);
#2297=FACE_OUTER_BOUND('',#3311,.T.);
#2298=FACE_OUTER_BOUND('',#3312,.T.);
#2299=FACE_OUTER_BOUND('',#3313,.T.);
#2300=FACE_OUTER_BOUND('',#3314,.T.);
#2301=FACE_OUTER_BOUND('',#3315,.T.);
#2302=FACE_OUTER_BOUND('',#3316,.T.);
#2303=FACE_OUTER_BOUND('',#3317,.T.);
#2304=FACE_OUTER_BOUND('',#3318,.T.);
#2305=FACE_OUTER_BOUND('',#3319,.T.);
#2306=FACE_OUTER_BOUND('',#3320,.T.);
#2307=FACE_OUTER_BOUND('',#3321,.T.);
#2308=FACE_OUTER_BOUND('',#3343,.T.);
#2309=FACE_OUTER_BOUND('',#3344,.T.);
#2310=FACE_OUTER_BOUND('',#3345,.T.);
#2311=FACE_OUTER_BOUND('',#3346,.T.);
#2312=FACE_OUTER_BOUND('',#3347,.T.);
#2313=FACE_OUTER_BOUND('',#3348,.T.);
#2314=FACE_OUTER_BOUND('',#3349,.T.);
#2315=FACE_OUTER_BOUND('',#3350,.T.);
#2316=FACE_OUTER_BOUND('',#3351,.T.);
#2317=FACE_OUTER_BOUND('',#3352,.T.);
#2318=FACE_OUTER_BOUND('',#3353,.T.);
#2319=FACE_OUTER_BOUND('',#3354,.T.);
#2320=FACE_OUTER_BOUND('',#3355,.T.);
#2321=FACE_OUTER_BOUND('',#3356,.T.);
#2322=FACE_OUTER_BOUND('',#3357,.T.);
#2323=FACE_OUTER_BOUND('',#3358,.T.);
#2324=FACE_OUTER_BOUND('',#3359,.T.);
#2325=FACE_OUTER_BOUND('',#3360,.T.);
#2326=FACE_OUTER_BOUND('',#3361,.T.);
#2327=FACE_OUTER_BOUND('',#3362,.T.);
#2328=FACE_OUTER_BOUND('',#3363,.T.);
#2329=FACE_OUTER_BOUND('',#3364,.T.);
#2330=FACE_OUTER_BOUND('',#3365,.T.);
#2331=FACE_OUTER_BOUND('',#3366,.T.);
#2332=FACE_OUTER_BOUND('',#3367,.T.);
#2333=FACE_OUTER_BOUND('',#3368,.T.);
#2334=FACE_OUTER_BOUND('',#3369,.T.);
#2335=FACE_OUTER_BOUND('',#3370,.T.);
#2336=FACE_OUTER_BOUND('',#3371,.T.);
#2337=FACE_OUTER_BOUND('',#3372,.T.);
#2338=FACE_OUTER_BOUND('',#3373,.T.);
#2339=FACE_OUTER_BOUND('',#3374,.T.);
#2340=FACE_OUTER_BOUND('',#3375,.T.);
#2341=FACE_OUTER_BOUND('',#3376,.T.);
#2342=FACE_OUTER_BOUND('',#3377,.T.);
#2343=FACE_OUTER_BOUND('',#3378,.T.);
#2344=FACE_OUTER_BOUND('',#3379,.T.);
#2345=FACE_OUTER_BOUND('',#3380,.T.);
#2346=FACE_OUTER_BOUND('',#3381,.T.);
#2347=FACE_OUTER_BOUND('',#3382,.T.);
#2348=FACE_OUTER_BOUND('',#3383,.T.);
#2349=FACE_OUTER_BOUND('',#3384,.T.);
#2350=FACE_OUTER_BOUND('',#3385,.T.);
#2351=FACE_OUTER_BOUND('',#3386,.T.);
#2352=FACE_OUTER_BOUND('',#3387,.T.);
#2353=FACE_OUTER_BOUND('',#3388,.T.);
#2354=FACE_OUTER_BOUND('',#3389,.T.);
#2355=FACE_OUTER_BOUND('',#3390,.T.);
#2356=FACE_OUTER_BOUND('',#3391,.T.);
#2357=FACE_OUTER_BOUND('',#3392,.T.);
#2358=FACE_OUTER_BOUND('',#3393,.T.);
#2359=FACE_OUTER_BOUND('',#3394,.T.);
#2360=FACE_OUTER_BOUND('',#3395,.T.);
#2361=FACE_OUTER_BOUND('',#3396,.T.);
#2362=FACE_OUTER_BOUND('',#3397,.T.);
#2363=FACE_OUTER_BOUND('',#3398,.T.);
#2364=FACE_OUTER_BOUND('',#3399,.T.);
#2365=FACE_OUTER_BOUND('',#3400,.T.);
#2366=FACE_OUTER_BOUND('',#3401,.T.);
#2367=FACE_OUTER_BOUND('',#3402,.T.);
#2368=FACE_OUTER_BOUND('',#3403,.T.);
#2369=FACE_OUTER_BOUND('',#3404,.T.);
#2370=FACE_OUTER_BOUND('',#3405,.T.);
#2371=FACE_OUTER_BOUND('',#3406,.T.);
#2372=FACE_OUTER_BOUND('',#3407,.T.);
#2373=FACE_OUTER_BOUND('',#3408,.T.);
#2374=FACE_OUTER_BOUND('',#3409,.T.);
#2375=FACE_OUTER_BOUND('',#3410,.T.);
#2376=FACE_OUTER_BOUND('',#3411,.T.);
#2377=FACE_OUTER_BOUND('',#3412,.T.);
#2378=FACE_OUTER_BOUND('',#3413,.T.);
#2379=FACE_OUTER_BOUND('',#3414,.T.);
#2380=FACE_OUTER_BOUND('',#3415,.T.);
#2381=FACE_OUTER_BOUND('',#3416,.T.);
#2382=FACE_OUTER_BOUND('',#3417,.T.);
#2383=FACE_OUTER_BOUND('',#3418,.T.);
#2384=FACE_OUTER_BOUND('',#3419,.T.);
#2385=FACE_OUTER_BOUND('',#3420,.T.);
#2386=FACE_OUTER_BOUND('',#3421,.T.);
#2387=FACE_OUTER_BOUND('',#3422,.T.);
#2388=FACE_OUTER_BOUND('',#3423,.T.);
#2389=FACE_OUTER_BOUND('',#3424,.T.);
#2390=FACE_OUTER_BOUND('',#3425,.T.);
#2391=FACE_OUTER_BOUND('',#3426,.T.);
#2392=FACE_OUTER_BOUND('',#3427,.T.);
#2393=FACE_OUTER_BOUND('',#3428,.T.);
#2394=FACE_OUTER_BOUND('',#3429,.T.);
#2395=FACE_OUTER_BOUND('',#3430,.T.);
#2396=FACE_OUTER_BOUND('',#3431,.T.);
#2397=FACE_OUTER_BOUND('',#3432,.T.);
#2398=FACE_OUTER_BOUND('',#3433,.T.);
#2399=FACE_OUTER_BOUND('',#3434,.T.);
#2400=FACE_OUTER_BOUND('',#3435,.T.);
#2401=FACE_OUTER_BOUND('',#3436,.T.);
#2402=FACE_OUTER_BOUND('',#3437,.T.);
#2403=FACE_OUTER_BOUND('',#3438,.T.);
#2404=FACE_OUTER_BOUND('',#3439,.T.);
#2405=FACE_OUTER_BOUND('',#3440,.T.);
#2406=FACE_OUTER_BOUND('',#3441,.T.);
#2407=FACE_OUTER_BOUND('',#3442,.T.);
#2408=FACE_OUTER_BOUND('',#3443,.T.);
#2409=FACE_OUTER_BOUND('',#3444,.T.);
#2410=FACE_OUTER_BOUND('',#3445,.T.);
#2411=FACE_OUTER_BOUND('',#3446,.T.);
#2412=FACE_OUTER_BOUND('',#3447,.T.);
#2413=FACE_OUTER_BOUND('',#3448,.T.);
#2414=FACE_OUTER_BOUND('',#3449,.T.);
#2415=FACE_OUTER_BOUND('',#3451,.T.);
#2416=FACE_OUTER_BOUND('',#3452,.T.);
#2417=FACE_OUTER_BOUND('',#3453,.T.);
#2418=FACE_OUTER_BOUND('',#3454,.T.);
#2419=FACE_OUTER_BOUND('',#3455,.T.);
#2420=FACE_OUTER_BOUND('',#3457,.T.);
#2421=FACE_OUTER_BOUND('',#3458,.T.);
#2422=FACE_OUTER_BOUND('',#3460,.T.);
#2423=FACE_OUTER_BOUND('',#3461,.T.);
#2424=FACE_OUTER_BOUND('',#3462,.T.);
#2425=FACE_OUTER_BOUND('',#3463,.T.);
#2426=FACE_OUTER_BOUND('',#3464,.T.);
#2427=FACE_OUTER_BOUND('',#3465,.T.);
#2428=FACE_OUTER_BOUND('',#3466,.T.);
#2429=FACE_OUTER_BOUND('',#3467,.T.);
#2430=FACE_OUTER_BOUND('',#3468,.T.);
#2431=FACE_OUTER_BOUND('',#3469,.T.);
#2432=FACE_OUTER_BOUND('',#3470,.T.);
#2433=FACE_OUTER_BOUND('',#3471,.T.);
#2434=FACE_OUTER_BOUND('',#3472,.T.);
#2435=FACE_OUTER_BOUND('',#3473,.T.);
#2436=FACE_OUTER_BOUND('',#3475,.T.);
#2437=FACE_OUTER_BOUND('',#3476,.T.);
#2438=FACE_OUTER_BOUND('',#3477,.T.);
#2439=FACE_OUTER_BOUND('',#3478,.T.);
#2440=FACE_OUTER_BOUND('',#3479,.T.);
#2441=FACE_OUTER_BOUND('',#3480,.T.);
#2442=FACE_OUTER_BOUND('',#3481,.T.);
#2443=FACE_OUTER_BOUND('',#3482,.T.);
#2444=FACE_OUTER_BOUND('',#3483,.T.);
#2445=FACE_OUTER_BOUND('',#3484,.T.);
#2446=FACE_OUTER_BOUND('',#3485,.T.);
#2447=FACE_OUTER_BOUND('',#3486,.T.);
#2448=FACE_OUTER_BOUND('',#3487,.T.);
#2449=FACE_OUTER_BOUND('',#3488,.T.);
#2450=FACE_OUTER_BOUND('',#3489,.T.);
#2451=FACE_OUTER_BOUND('',#3490,.T.);
#2452=FACE_OUTER_BOUND('',#3491,.T.);
#2453=FACE_OUTER_BOUND('',#3492,.T.);
#2454=FACE_OUTER_BOUND('',#3493,.T.);
#2455=FACE_OUTER_BOUND('',#3494,.T.);
#2456=FACE_OUTER_BOUND('',#3495,.T.);
#2457=FACE_OUTER_BOUND('',#3496,.T.);
#2458=FACE_OUTER_BOUND('',#3497,.T.);
#2459=FACE_OUTER_BOUND('',#3498,.T.);
#2460=FACE_OUTER_BOUND('',#3499,.T.);
#2461=FACE_OUTER_BOUND('',#3500,.T.);
#2462=FACE_OUTER_BOUND('',#3501,.T.);
#2463=FACE_OUTER_BOUND('',#3502,.T.);
#2464=FACE_OUTER_BOUND('',#3503,.T.);
#2465=FACE_OUTER_BOUND('',#3504,.T.);
#2466=FACE_OUTER_BOUND('',#3505,.T.);
#2467=FACE_OUTER_BOUND('',#3506,.T.);
#2468=FACE_OUTER_BOUND('',#3507,.T.);
#2469=FACE_OUTER_BOUND('',#3509,.T.);
#2470=FACE_OUTER_BOUND('',#3510,.T.);
#2471=FACE_OUTER_BOUND('',#3511,.T.);
#2472=FACE_OUTER_BOUND('',#3512,.T.);
#2473=FACE_OUTER_BOUND('',#3513,.T.);
#2474=FACE_OUTER_BOUND('',#3514,.T.);
#2475=FACE_OUTER_BOUND('',#3515,.T.);
#2476=FACE_OUTER_BOUND('',#3516,.T.);
#2477=FACE_OUTER_BOUND('',#3517,.T.);
#2478=FACE_OUTER_BOUND('',#3518,.T.);
#2479=FACE_OUTER_BOUND('',#3519,.T.);
#2480=FACE_OUTER_BOUND('',#3520,.T.);
#2481=FACE_OUTER_BOUND('',#3521,.T.);
#2482=FACE_OUTER_BOUND('',#3522,.T.);
#2483=FACE_OUTER_BOUND('',#3523,.T.);
#2484=FACE_OUTER_BOUND('',#3524,.T.);
#2485=FACE_OUTER_BOUND('',#3525,.T.);
#2486=FACE_OUTER_BOUND('',#3526,.T.);
#2487=FACE_OUTER_BOUND('',#3527,.T.);
#2488=FACE_OUTER_BOUND('',#3528,.T.);
#2489=FACE_OUTER_BOUND('',#3529,.T.);
#2490=FACE_OUTER_BOUND('',#3530,.T.);
#2491=FACE_OUTER_BOUND('',#3531,.T.);
#2492=FACE_OUTER_BOUND('',#3532,.T.);
#2493=FACE_OUTER_BOUND('',#3533,.T.);
#2494=FACE_OUTER_BOUND('',#3534,.T.);
#2495=FACE_OUTER_BOUND('',#3535,.T.);
#2496=FACE_OUTER_BOUND('',#3536,.T.);
#2497=FACE_OUTER_BOUND('',#3537,.T.);
#2498=FACE_OUTER_BOUND('',#3538,.T.);
#2499=FACE_OUTER_BOUND('',#3539,.T.);
#2500=FACE_OUTER_BOUND('',#3540,.T.);
#2501=FACE_OUTER_BOUND('',#3541,.T.);
#2502=FACE_OUTER_BOUND('',#3542,.T.);
#2503=FACE_OUTER_BOUND('',#3543,.T.);
#2504=FACE_OUTER_BOUND('',#3544,.T.);
#2505=FACE_OUTER_BOUND('',#3545,.T.);
#2506=FACE_OUTER_BOUND('',#3546,.T.);
#2507=FACE_OUTER_BOUND('',#3547,.T.);
#2508=FACE_OUTER_BOUND('',#3548,.T.);
#2509=FACE_OUTER_BOUND('',#3549,.T.);
#2510=FACE_OUTER_BOUND('',#3550,.T.);
#2511=FACE_OUTER_BOUND('',#3551,.T.);
#2512=FACE_OUTER_BOUND('',#3552,.T.);
#2513=FACE_OUTER_BOUND('',#3553,.T.);
#2514=FACE_OUTER_BOUND('',#3554,.T.);
#2515=FACE_OUTER_BOUND('',#3555,.T.);
#2516=FACE_OUTER_BOUND('',#3556,.T.);
#2517=FACE_OUTER_BOUND('',#3557,.T.);
#2518=FACE_OUTER_BOUND('',#3558,.T.);
#2519=FACE_OUTER_BOUND('',#3559,.T.);
#2520=FACE_OUTER_BOUND('',#3560,.T.);
#2521=FACE_OUTER_BOUND('',#3561,.T.);
#2522=FACE_OUTER_BOUND('',#3562,.T.);
#2523=FACE_OUTER_BOUND('',#3563,.T.);
#2524=FACE_OUTER_BOUND('',#3564,.T.);
#2525=FACE_OUTER_BOUND('',#3565,.T.);
#2526=FACE_OUTER_BOUND('',#3566,.T.);
#2527=FACE_OUTER_BOUND('',#3568,.T.);
#2528=FACE_OUTER_BOUND('',#3569,.T.);
#2529=FACE_OUTER_BOUND('',#3570,.T.);
#2530=FACE_OUTER_BOUND('',#3571,.T.);
#2531=FACE_OUTER_BOUND('',#3572,.T.);
#2532=FACE_OUTER_BOUND('',#3573,.T.);
#2533=FACE_OUTER_BOUND('',#3574,.T.);
#2534=FACE_OUTER_BOUND('',#3575,.T.);
#2535=FACE_OUTER_BOUND('',#3576,.T.);
#2536=FACE_OUTER_BOUND('',#3577,.T.);
#2537=FACE_OUTER_BOUND('',#3578,.T.);
#2538=FACE_OUTER_BOUND('',#3579,.T.);
#2539=FACE_OUTER_BOUND('',#3580,.T.);
#2540=FACE_OUTER_BOUND('',#3581,.T.);
#2541=FACE_OUTER_BOUND('',#3582,.T.);
#2542=FACE_OUTER_BOUND('',#3583,.T.);
#2543=FACE_OUTER_BOUND('',#3584,.T.);
#2544=FACE_OUTER_BOUND('',#3585,.T.);
#2545=FACE_OUTER_BOUND('',#3586,.T.);
#2546=FACE_OUTER_BOUND('',#3587,.T.);
#2547=FACE_OUTER_BOUND('',#3588,.T.);
#2548=FACE_OUTER_BOUND('',#3589,.T.);
#2549=FACE_OUTER_BOUND('',#3590,.T.);
#2550=FACE_OUTER_BOUND('',#3591,.T.);
#2551=FACE_OUTER_BOUND('',#3592,.T.);
#2552=FACE_OUTER_BOUND('',#3593,.T.);
#2553=FACE_OUTER_BOUND('',#3594,.T.);
#2554=FACE_OUTER_BOUND('',#3595,.T.);
#2555=FACE_OUTER_BOUND('',#3596,.T.);
#2556=FACE_OUTER_BOUND('',#3597,.T.);
#2557=FACE_OUTER_BOUND('',#3598,.T.);
#2558=FACE_OUTER_BOUND('',#3599,.T.);
#2559=FACE_OUTER_BOUND('',#3600,.T.);
#2560=FACE_OUTER_BOUND('',#3601,.T.);
#2561=FACE_OUTER_BOUND('',#3602,.T.);
#2562=FACE_OUTER_BOUND('',#3603,.T.);
#2563=FACE_OUTER_BOUND('',#3604,.T.);
#2564=FACE_OUTER_BOUND('',#3605,.T.);
#2565=FACE_OUTER_BOUND('',#3606,.T.);
#2566=FACE_OUTER_BOUND('',#3607,.T.);
#2567=FACE_OUTER_BOUND('',#3608,.T.);
#2568=FACE_OUTER_BOUND('',#3609,.T.);
#2569=FACE_OUTER_BOUND('',#3610,.T.);
#2570=FACE_OUTER_BOUND('',#3611,.T.);
#2571=FACE_OUTER_BOUND('',#3612,.T.);
#2572=FACE_OUTER_BOUND('',#3613,.T.);
#2573=FACE_OUTER_BOUND('',#3614,.T.);
#2574=FACE_OUTER_BOUND('',#3615,.T.);
#2575=FACE_OUTER_BOUND('',#3616,.T.);
#2576=FACE_OUTER_BOUND('',#3617,.T.);
#2577=FACE_OUTER_BOUND('',#3618,.T.);
#2578=FACE_OUTER_BOUND('',#3619,.T.);
#2579=FACE_OUTER_BOUND('',#3620,.T.);
#2580=FACE_OUTER_BOUND('',#3621,.T.);
#2581=FACE_OUTER_BOUND('',#3622,.T.);
#2582=FACE_OUTER_BOUND('',#3623,.T.);
#2583=FACE_OUTER_BOUND('',#3624,.T.);
#2584=FACE_OUTER_BOUND('',#3625,.T.);
#2585=FACE_OUTER_BOUND('',#3626,.T.);
#2586=FACE_OUTER_BOUND('',#3627,.T.);
#2587=FACE_OUTER_BOUND('',#3628,.T.);
#2588=FACE_OUTER_BOUND('',#3629,.T.);
#2589=FACE_OUTER_BOUND('',#3630,.T.);
#2590=FACE_OUTER_BOUND('',#3631,.T.);
#2591=FACE_OUTER_BOUND('',#3632,.T.);
#2592=FACE_OUTER_BOUND('',#3633,.T.);
#2593=FACE_OUTER_BOUND('',#3634,.T.);
#2594=FACE_OUTER_BOUND('',#3635,.T.);
#2595=FACE_OUTER_BOUND('',#3636,.T.);
#2596=FACE_OUTER_BOUND('',#3637,.T.);
#2597=FACE_OUTER_BOUND('',#3638,.T.);
#2598=FACE_OUTER_BOUND('',#3639,.T.);
#2599=FACE_OUTER_BOUND('',#3640,.T.);
#2600=FACE_OUTER_BOUND('',#3641,.T.);
#2601=FACE_OUTER_BOUND('',#3642,.T.);
#2602=FACE_OUTER_BOUND('',#3643,.T.);
#2603=FACE_OUTER_BOUND('',#3644,.T.);
#2604=FACE_OUTER_BOUND('',#3645,.T.);
#2605=FACE_OUTER_BOUND('',#3646,.T.);
#2606=FACE_OUTER_BOUND('',#3647,.T.);
#2607=FACE_OUTER_BOUND('',#3648,.T.);
#2608=FACE_OUTER_BOUND('',#3649,.T.);
#2609=FACE_OUTER_BOUND('',#3650,.T.);
#2610=FACE_OUTER_BOUND('',#3651,.T.);
#2611=FACE_OUTER_BOUND('',#3652,.T.);
#2612=FACE_OUTER_BOUND('',#3653,.T.);
#2613=FACE_OUTER_BOUND('',#3654,.T.);
#2614=FACE_OUTER_BOUND('',#3655,.T.);
#2615=FACE_OUTER_BOUND('',#3656,.T.);
#2616=FACE_OUTER_BOUND('',#3657,.T.);
#2617=FACE_OUTER_BOUND('',#3658,.T.);
#2618=FACE_OUTER_BOUND('',#3659,.T.);
#2619=FACE_OUTER_BOUND('',#3660,.T.);
#2620=FACE_OUTER_BOUND('',#3661,.T.);
#2621=FACE_OUTER_BOUND('',#3662,.T.);
#2622=FACE_OUTER_BOUND('',#3663,.T.);
#2623=FACE_OUTER_BOUND('',#3664,.T.);
#2624=FACE_OUTER_BOUND('',#3665,.T.);
#2625=FACE_OUTER_BOUND('',#3666,.T.);
#2626=FACE_OUTER_BOUND('',#3667,.T.);
#2627=FACE_OUTER_BOUND('',#3668,.T.);
#2628=FACE_OUTER_BOUND('',#3669,.T.);
#2629=FACE_OUTER_BOUND('',#3670,.T.);
#2630=FACE_OUTER_BOUND('',#3671,.T.);
#2631=FACE_OUTER_BOUND('',#3672,.T.);
#2632=FACE_OUTER_BOUND('',#3673,.T.);
#2633=FACE_OUTER_BOUND('',#3674,.T.);
#2634=FACE_OUTER_BOUND('',#3675,.T.);
#2635=FACE_OUTER_BOUND('',#3676,.T.);
#2636=FACE_OUTER_BOUND('',#3677,.T.);
#2637=FACE_OUTER_BOUND('',#3678,.T.);
#2638=FACE_OUTER_BOUND('',#3679,.T.);
#2639=FACE_OUTER_BOUND('',#3680,.T.);
#2640=FACE_OUTER_BOUND('',#3681,.T.);
#2641=FACE_OUTER_BOUND('',#3682,.T.);
#2642=FACE_OUTER_BOUND('',#3683,.T.);
#2643=FACE_OUTER_BOUND('',#3684,.T.);
#2644=FACE_OUTER_BOUND('',#3685,.T.);
#2645=FACE_OUTER_BOUND('',#3686,.T.);
#2646=FACE_OUTER_BOUND('',#3687,.T.);
#2647=FACE_OUTER_BOUND('',#3688,.T.);
#2648=FACE_OUTER_BOUND('',#3689,.T.);
#2649=FACE_OUTER_BOUND('',#3690,.T.);
#2650=FACE_OUTER_BOUND('',#3691,.T.);
#2651=FACE_OUTER_BOUND('',#3692,.T.);
#2652=FACE_OUTER_BOUND('',#3693,.T.);
#2653=FACE_OUTER_BOUND('',#3694,.T.);
#2654=FACE_OUTER_BOUND('',#3695,.T.);
#2655=FACE_OUTER_BOUND('',#3696,.T.);
#2656=FACE_OUTER_BOUND('',#3698,.T.);
#2657=FACE_OUTER_BOUND('',#3699,.T.);
#2658=FACE_OUTER_BOUND('',#3729,.T.);
#2659=FACE_OUTER_BOUND('',#3730,.T.);
#2660=FACE_OUTER_BOUND('',#3737,.T.);
#2661=FACE_OUTER_BOUND('',#3738,.T.);
#2662=FACE_OUTER_BOUND('',#3739,.T.);
#2663=FACE_OUTER_BOUND('',#3740,.T.);
#2664=FACE_OUTER_BOUND('',#3741,.T.);
#2665=FACE_OUTER_BOUND('',#3742,.T.);
#2666=FACE_OUTER_BOUND('',#3743,.T.);
#2667=FACE_OUTER_BOUND('',#3744,.T.);
#2668=FACE_OUTER_BOUND('',#3745,.T.);
#2669=FACE_OUTER_BOUND('',#3748,.T.);
#2670=FACE_OUTER_BOUND('',#3749,.T.);
#2671=FACE_OUTER_BOUND('',#3750,.T.);
#2672=FACE_OUTER_BOUND('',#3751,.T.);
#2673=FACE_OUTER_BOUND('',#3752,.T.);
#2674=FACE_OUTER_BOUND('',#3753,.T.);
#2675=FACE_OUTER_BOUND('',#3754,.T.);
#2676=FACE_OUTER_BOUND('',#3755,.T.);
#2677=FACE_OUTER_BOUND('',#3756,.T.);
#2678=FACE_OUTER_BOUND('',#3757,.T.);
#2679=FACE_OUTER_BOUND('',#3758,.T.);
#2680=FACE_OUTER_BOUND('',#3759,.T.);
#2681=FACE_OUTER_BOUND('',#3760,.T.);
#2682=FACE_OUTER_BOUND('',#3761,.T.);
#2683=FACE_OUTER_BOUND('',#3764,.T.);
#2684=FACE_OUTER_BOUND('',#3765,.T.);
#2685=FACE_OUTER_BOUND('',#3766,.T.);
#2686=FACE_OUTER_BOUND('',#3767,.T.);
#2687=FACE_OUTER_BOUND('',#3768,.T.);
#2688=FACE_OUTER_BOUND('',#3769,.T.);
#2689=FACE_OUTER_BOUND('',#3772,.T.);
#2690=FACE_OUTER_BOUND('',#3773,.T.);
#2691=FACE_OUTER_BOUND('',#3774,.T.);
#2692=FACE_OUTER_BOUND('',#3775,.T.);
#2693=FACE_OUTER_BOUND('',#3776,.T.);
#2694=FACE_OUTER_BOUND('',#3777,.T.);
#2695=FACE_OUTER_BOUND('',#3778,.T.);
#2696=FACE_OUTER_BOUND('',#3779,.T.);
#2697=FACE_OUTER_BOUND('',#3780,.T.);
#2698=FACE_OUTER_BOUND('',#3781,.T.);
#2699=FACE_OUTER_BOUND('',#3782,.T.);
#2700=FACE_OUTER_BOUND('',#3783,.T.);
#2701=FACE_OUTER_BOUND('',#3786,.T.);
#2702=FACE_OUTER_BOUND('',#3787,.T.);
#2703=FACE_OUTER_BOUND('',#3788,.T.);
#2704=FACE_OUTER_BOUND('',#3789,.T.);
#2705=FACE_OUTER_BOUND('',#3790,.T.);
#2706=FACE_OUTER_BOUND('',#3791,.T.);
#2707=FACE_OUTER_BOUND('',#3792,.T.);
#2708=FACE_OUTER_BOUND('',#3793,.T.);
#2709=FACE_OUTER_BOUND('',#3794,.T.);
#2710=FACE_OUTER_BOUND('',#3795,.T.);
#2711=FACE_OUTER_BOUND('',#3796,.T.);
#2712=FACE_OUTER_BOUND('',#3797,.T.);
#2713=FACE_OUTER_BOUND('',#3798,.T.);
#2714=FACE_OUTER_BOUND('',#3799,.T.);
#2715=FACE_OUTER_BOUND('',#3800,.T.);
#2716=FACE_OUTER_BOUND('',#3801,.T.);
#2717=FACE_OUTER_BOUND('',#3802,.T.);
#2718=FACE_OUTER_BOUND('',#3803,.T.);
#2719=FACE_OUTER_BOUND('',#3804,.T.);
#2720=FACE_OUTER_BOUND('',#3805,.T.);
#2721=FACE_OUTER_BOUND('',#3807,.T.);
#2722=FACE_OUTER_BOUND('',#3808,.T.);
#2723=FACE_OUTER_BOUND('',#3809,.T.);
#2724=FACE_OUTER_BOUND('',#3810,.T.);
#2725=FACE_OUTER_BOUND('',#3811,.T.);
#2726=FACE_OUTER_BOUND('',#3812,.T.);
#2727=FACE_OUTER_BOUND('',#3813,.T.);
#2728=FACE_OUTER_BOUND('',#3814,.T.);
#2729=FACE_OUTER_BOUND('',#3815,.T.);
#2730=FACE_OUTER_BOUND('',#3816,.T.);
#2731=FACE_OUTER_BOUND('',#3817,.T.);
#2732=FACE_OUTER_BOUND('',#3818,.T.);
#2733=FACE_OUTER_BOUND('',#3819,.T.);
#2734=FACE_OUTER_BOUND('',#3820,.T.);
#2735=FACE_OUTER_BOUND('',#3823,.T.);
#2736=FACE_OUTER_BOUND('',#3824,.T.);
#2737=FACE_OUTER_BOUND('',#3825,.T.);
#2738=FACE_OUTER_BOUND('',#3826,.T.);
#2739=FACE_OUTER_BOUND('',#3827,.T.);
#2740=FACE_OUTER_BOUND('',#3828,.T.);
#2741=FACE_OUTER_BOUND('',#3829,.T.);
#2742=FACE_OUTER_BOUND('',#3830,.T.);
#2743=FACE_OUTER_BOUND('',#3831,.T.);
#2744=FACE_OUTER_BOUND('',#3832,.T.);
#2745=FACE_OUTER_BOUND('',#3833,.T.);
#2746=FACE_OUTER_BOUND('',#3834,.T.);
#2747=FACE_OUTER_BOUND('',#3837,.T.);
#2748=FACE_OUTER_BOUND('',#3838,.T.);
#2749=FACE_OUTER_BOUND('',#3839,.T.);
#2750=FACE_OUTER_BOUND('',#3840,.T.);
#2751=FACE_OUTER_BOUND('',#3841,.T.);
#2752=FACE_OUTER_BOUND('',#3842,.T.);
#2753=FACE_OUTER_BOUND('',#3843,.T.);
#2754=FACE_OUTER_BOUND('',#3844,.T.);
#2755=FACE_OUTER_BOUND('',#3845,.T.);
#2756=FACE_OUTER_BOUND('',#3847,.T.);
#2757=FACE_OUTER_BOUND('',#3848,.T.);
#2758=FACE_OUTER_BOUND('',#3850,.T.);
#2759=FACE_OUTER_BOUND('',#3851,.T.);
#2760=FACE_OUTER_BOUND('',#3853,.T.);
#2761=FACE_OUTER_BOUND('',#3854,.T.);
#2762=FACE_OUTER_BOUND('',#3856,.T.);
#2763=FACE_OUTER_BOUND('',#3857,.T.);
#2764=FACE_OUTER_BOUND('',#3858,.T.);
#2765=FACE_OUTER_BOUND('',#3859,.T.);
#2766=FACE_OUTER_BOUND('',#3860,.T.);
#2767=FACE_OUTER_BOUND('',#3861,.T.);
#2768=FACE_OUTER_BOUND('',#3862,.T.);
#2769=FACE_OUTER_BOUND('',#3863,.T.);
#2770=FACE_OUTER_BOUND('',#3864,.T.);
#2771=FACE_OUTER_BOUND('',#3865,.T.);
#2772=FACE_OUTER_BOUND('',#3867,.T.);
#2773=FACE_OUTER_BOUND('',#3868,.T.);
#2774=FACE_OUTER_BOUND('',#3869,.T.);
#2775=FACE_OUTER_BOUND('',#3870,.T.);
#2776=FACE_OUTER_BOUND('',#3871,.T.);
#2777=FACE_OUTER_BOUND('',#3872,.T.);
#2778=FACE_OUTER_BOUND('',#3874,.T.);
#2779=FACE_OUTER_BOUND('',#3875,.T.);
#2780=FACE_OUTER_BOUND('',#3877,.T.);
#2781=FACE_OUTER_BOUND('',#3878,.T.);
#2782=FACE_OUTER_BOUND('',#3879,.T.);
#2783=FACE_OUTER_BOUND('',#3880,.T.);
#2784=FACE_OUTER_BOUND('',#3881,.T.);
#2785=FACE_OUTER_BOUND('',#3882,.T.);
#2786=FACE_OUTER_BOUND('',#3883,.T.);
#2787=FACE_OUTER_BOUND('',#3884,.T.);
#2788=FACE_OUTER_BOUND('',#3885,.T.);
#2789=EDGE_LOOP('',(#10802,#10803,#10804,#10805,#10806));
#2790=EDGE_LOOP('',(#10807,#10808,#10809,#10810,#10811));
#2791=EDGE_LOOP('',(#10812));
#2792=EDGE_LOOP('',(#10813));
#2793=EDGE_LOOP('',(#10814,#10815,#10816,#10817));
#2794=EDGE_LOOP('',(#10818,#10819,#10820,#10821,#10822,#10823,#10824,#10825,
#10826,#10827));
#2795=EDGE_LOOP('',(#10828));
#2796=EDGE_LOOP('',(#10829,#10830,#10831,#10832));
#2797=EDGE_LOOP('',(#10833,#10834,#10835,#10836));
#2798=EDGE_LOOP('',(#10837,#10838,#10839,#10840));
#2799=EDGE_LOOP('',(#10841,#10842,#10843,#10844,#10845,#10846,#10847,#10848,
#10849,#10850,#10851,#10852,#10853,#10854));
#2800=EDGE_LOOP('',(#10855,#10856,#10857,#10858,#10859));
#2801=EDGE_LOOP('',(#10860,#10861,#10862,#10863,#10864,#10865));
#2802=EDGE_LOOP('',(#10866,#10867,#10868,#10869));
#2803=EDGE_LOOP('',(#10870,#10871,#10872,#10873));
#2804=EDGE_LOOP('',(#10874,#10875,#10876,#10877));
#2805=EDGE_LOOP('',(#10878,#10879,#10880,#10881));
#2806=EDGE_LOOP('',(#10882,#10883,#10884,#10885));
#2807=EDGE_LOOP('',(#10886,#10887,#10888,#10889));
#2808=EDGE_LOOP('',(#10890,#10891,#10892,#10893));
#2809=EDGE_LOOP('',(#10894,#10895,#10896,#10897));
#2810=EDGE_LOOP('',(#10898,#10899,#10900,#10901));
#2811=EDGE_LOOP('',(#10902,#10903,#10904,#10905));
#2812=EDGE_LOOP('',(#10906,#10907,#10908,#10909));
#2813=EDGE_LOOP('',(#10910,#10911,#10912,#10913,#10914,#10915,#10916));
#2814=EDGE_LOOP('',(#10917,#10918,#10919,#10920,#10921));
#2815=EDGE_LOOP('',(#10922,#10923,#10924,#10925,#10926));
#2816=EDGE_LOOP('',(#10927,#10928,#10929,#10930,#10931,#10932,#10933,#10934,
#10935,#10936));
#2817=EDGE_LOOP('',(#10937,#10938,#10939,#10940));
#2818=EDGE_LOOP('',(#10941,#10942,#10943));
#2819=EDGE_LOOP('',(#10944,#10945,#10946));
#2820=EDGE_LOOP('',(#10947,#10948,#10949,#10950));
#2821=EDGE_LOOP('',(#10951,#10952,#10953,#10954));
#2822=EDGE_LOOP('',(#10955,#10956,#10957,#10958));
#2823=EDGE_LOOP('',(#10959,#10960,#10961));
#2824=EDGE_LOOP('',(#10962,#10963,#10964,#10965));
#2825=EDGE_LOOP('',(#10966,#10967,#10968,#10969));
#2826=EDGE_LOOP('',(#10970,#10971,#10972));
#2827=EDGE_LOOP('',(#10973,#10974,#10975));
#2828=EDGE_LOOP('',(#10976,#10977,#10978,#10979));
#2829=EDGE_LOOP('',(#10980,#10981,#10982,#10983));
#2830=EDGE_LOOP('',(#10984,#10985,#10986));
#2831=EDGE_LOOP('',(#10987,#10988,#10989));
#2832=EDGE_LOOP('',(#10990,#10991,#10992,#10993));
#2833=EDGE_LOOP('',(#10994,#10995,#10996,#10997));
#2834=EDGE_LOOP('',(#10998,#10999,#11000));
#2835=EDGE_LOOP('',(#11001,#11002,#11003));
#2836=EDGE_LOOP('',(#11004,#11005,#11006,#11007));
#2837=EDGE_LOOP('',(#11008,#11009,#11010,#11011));
#2838=EDGE_LOOP('',(#11012,#11013,#11014));
#2839=EDGE_LOOP('',(#11015,#11016,#11017,#11018));
#2840=EDGE_LOOP('',(#11019,#11020,#11021));
#2841=EDGE_LOOP('',(#11022,#11023,#11024,#11025));
#2842=EDGE_LOOP('',(#11026,#11027,#11028,#11029,#11030));
#2843=EDGE_LOOP('',(#11031,#11032,#11033));
#2844=EDGE_LOOP('',(#11034,#11035,#11036,#11037,#11038,#11039,#11040));
#2845=EDGE_LOOP('',(#11041,#11042,#11043));
#2846=EDGE_LOOP('',(#11044,#11045,#11046,#11047));
#2847=EDGE_LOOP('',(#11048,#11049,#11050,#11051,#11052,#11053,#11054,#11055,
#11056,#11057,#11058));
#2848=EDGE_LOOP('',(#11059,#11060,#11061,#11062,#11063,#11064,#11065,#11066));
#2849=EDGE_LOOP('',(#11067,#11068,#11069,#11070,#11071,#11072,#11073,#11074,
#11075,#11076,#11077,#11078,#11079,#11080,#11081,#11082));
#2850=EDGE_LOOP('',(#11083,#11084,#11085,#11086,#11087,#11088,#11089,#11090,
#11091,#11092));
#2851=EDGE_LOOP('',(#11093,#11094,#11095,#11096));
#2852=EDGE_LOOP('',(#11097,#11098,#11099,#11100));
#2853=EDGE_LOOP('',(#11101,#11102,#11103,#11104));
#2854=EDGE_LOOP('',(#11105,#11106,#11107,#11108));
#2855=EDGE_LOOP('',(#11109,#11110,#11111,#11112,#11113));
#2856=EDGE_LOOP('',(#11114,#11115,#11116,#11117));
#2857=EDGE_LOOP('',(#11118,#11119,#11120,#11121));
#2858=EDGE_LOOP('',(#11122,#11123,#11124,#11125));
#2859=EDGE_LOOP('',(#11126,#11127,#11128,#11129,#11130));
#2860=EDGE_LOOP('',(#11131,#11132,#11133));
#2861=EDGE_LOOP('',(#11134,#11135,#11136));
#2862=EDGE_LOOP('',(#11137,#11138,#11139,#11140));
#2863=EDGE_LOOP('',(#11141,#11142,#11143,#11144));
#2864=EDGE_LOOP('',(#11145,#11146,#11147,#11148));
#2865=EDGE_LOOP('',(#11149,#11150,#11151));
#2866=EDGE_LOOP('',(#11152,#11153,#11154,#11155));
#2867=EDGE_LOOP('',(#11156,#11157,#11158,#11159));
#2868=EDGE_LOOP('',(#11160,#11161,#11162));
#2869=EDGE_LOOP('',(#11163,#11164,#11165,#11166));
#2870=EDGE_LOOP('',(#11167,#11168,#11169,#11170));
#2871=EDGE_LOOP('',(#11171,#11172,#11173,#11174));
#2872=EDGE_LOOP('',(#11175,#11176,#11177,#11178));
#2873=EDGE_LOOP('',(#11179,#11180,#11181));
#2874=EDGE_LOOP('',(#11182,#11183,#11184,#11185,#11186));
#2875=EDGE_LOOP('',(#11187,#11188,#11189,#11190,#11191,#11192));
#2876=EDGE_LOOP('',(#11193));
#2877=EDGE_LOOP('',(#11194));
#2878=EDGE_LOOP('',(#11195,#11196,#11197,#11198,#11199,#11200));
#2879=EDGE_LOOP('',(#11201,#11202,#11203,#11204,#11205,#11206,#11207,#11208,
#11209,#11210,#11211,#11212,#11213,#11214,#11215,#11216,#11217,#11218,#11219,
#11220,#11221,#11222,#11223,#11224,#11225,#11226,#11227));
#2880=EDGE_LOOP('',(#11228,#11229,#11230,#11231));
#2881=EDGE_LOOP('',(#11232,#11233,#11234,#11235));
#2882=EDGE_LOOP('',(#11236,#11237,#11238,#11239));
#2883=EDGE_LOOP('',(#11240,#11241,#11242,#11243));
#2884=EDGE_LOOP('',(#11244,#11245,#11246,#11247));
#2885=EDGE_LOOP('',(#11248,#11249,#11250,#11251));
#2886=EDGE_LOOP('',(#11252,#11253,#11254,#11255));
#2887=EDGE_LOOP('',(#11256,#11257,#11258,#11259,#11260));
#2888=EDGE_LOOP('',(#11261,#11262,#11263,#11264));
#2889=EDGE_LOOP('',(#11265,#11266,#11267,#11268));
#2890=EDGE_LOOP('',(#11269,#11270,#11271,#11272));
#2891=EDGE_LOOP('',(#11273,#11274,#11275,#11276));
#2892=EDGE_LOOP('',(#11277));
#2893=EDGE_LOOP('',(#11278,#11279,#11280,#11281));
#2894=EDGE_LOOP('',(#11282,#11283,#11284,#11285));
#2895=EDGE_LOOP('',(#11286,#11287,#11288,#11289));
#2896=EDGE_LOOP('',(#11290,#11291,#11292,#11293));
#2897=EDGE_LOOP('',(#11294,#11295,#11296,#11297));
#2898=EDGE_LOOP('',(#11298,#11299,#11300,#11301));
#2899=EDGE_LOOP('',(#11302,#11303,#11304,#11305));
#2900=EDGE_LOOP('',(#11306,#11307,#11308,#11309));
#2901=EDGE_LOOP('',(#11310,#11311,#11312,#11313));
#2902=EDGE_LOOP('',(#11314,#11315,#11316,#11317));
#2903=EDGE_LOOP('',(#11318,#11319,#11320,#11321));
#2904=EDGE_LOOP('',(#11322,#11323,#11324,#11325));
#2905=EDGE_LOOP('',(#11326,#11327,#11328,#11329));
#2906=EDGE_LOOP('',(#11330,#11331,#11332,#11333));
#2907=EDGE_LOOP('',(#11334,#11335,#11336,#11337,#11338,#11339,#11340,#11341,
#11342,#11343,#11344));
#2908=EDGE_LOOP('',(#11345,#11346,#11347,#11348));
#2909=EDGE_LOOP('',(#11349,#11350,#11351,#11352));
#2910=EDGE_LOOP('',(#11353,#11354,#11355,#11356));
#2911=EDGE_LOOP('',(#11357,#11358,#11359,#11360));
#2912=EDGE_LOOP('',(#11361,#11362,#11363,#11364));
#2913=EDGE_LOOP('',(#11365,#11366,#11367,#11368));
#2914=EDGE_LOOP('',(#11369,#11370,#11371,#11372));
#2915=EDGE_LOOP('',(#11373,#11374,#11375,#11376));
#2916=EDGE_LOOP('',(#11377,#11378,#11379,#11380,#11381,#11382,#11383,#11384));
#2917=EDGE_LOOP('',(#11385,#11386,#11387,#11388));
#2918=EDGE_LOOP('',(#11389,#11390,#11391,#11392));
#2919=EDGE_LOOP('',(#11393,#11394,#11395,#11396));
#2920=EDGE_LOOP('',(#11397,#11398,#11399,#11400));
#2921=EDGE_LOOP('',(#11401,#11402,#11403,#11404));
#2922=EDGE_LOOP('',(#11405,#11406,#11407,#11408));
#2923=EDGE_LOOP('',(#11409,#11410,#11411,#11412));
#2924=EDGE_LOOP('',(#11413,#11414,#11415,#11416));
#2925=EDGE_LOOP('',(#11417,#11418,#11419,#11420));
#2926=EDGE_LOOP('',(#11421,#11422,#11423,#11424));
#2927=EDGE_LOOP('',(#11425,#11426,#11427,#11428));
#2928=EDGE_LOOP('',(#11429,#11430,#11431,#11432));
#2929=EDGE_LOOP('',(#11433,#11434,#11435,#11436));
#2930=EDGE_LOOP('',(#11437,#11438,#11439,#11440));
#2931=EDGE_LOOP('',(#11441,#11442,#11443,#11444));
#2932=EDGE_LOOP('',(#11445,#11446,#11447,#11448));
#2933=EDGE_LOOP('',(#11449,#11450,#11451,#11452,#11453,#11454,#11455,#11456,
#11457,#11458,#11459,#11460,#11461,#11462,#11463,#11464));
#2934=EDGE_LOOP('',(#11465,#11466,#11467,#11468));
#2935=EDGE_LOOP('',(#11469,#11470,#11471,#11472));
#2936=EDGE_LOOP('',(#11473,#11474,#11475,#11476));
#2937=EDGE_LOOP('',(#11477,#11478,#11479,#11480));
#2938=EDGE_LOOP('',(#11481,#11482,#11483,#11484));
#2939=EDGE_LOOP('',(#11485,#11486,#11487,#11488));
#2940=EDGE_LOOP('',(#11489,#11490,#11491,#11492));
#2941=EDGE_LOOP('',(#11493,#11494,#11495,#11496));
#2942=EDGE_LOOP('',(#11497,#11498,#11499,#11500));
#2943=EDGE_LOOP('',(#11501,#11502,#11503,#11504));
#2944=EDGE_LOOP('',(#11505,#11506,#11507,#11508,#11509,#11510,#11511,#11512,
#11513,#11514));
#2945=EDGE_LOOP('',(#11515,#11516,#11517,#11518));
#2946=EDGE_LOOP('',(#11519));
#2947=EDGE_LOOP('',(#11520,#11521,#11522,#11523));
#2948=EDGE_LOOP('',(#11524,#11525,#11526,#11527));
#2949=EDGE_LOOP('',(#11528,#11529,#11530,#11531,#11532,#11533,#11534,#11535,
#11536,#11537,#11538,#11539,#11540,#11541,#11542));
#2950=EDGE_LOOP('',(#11543,#11544,#11545));
#2951=EDGE_LOOP('',(#11546,#11547,#11548,#11549));
#2952=EDGE_LOOP('',(#11550,#11551,#11552,#11553));
#2953=EDGE_LOOP('',(#11554,#11555,#11556,#11557));
#2954=EDGE_LOOP('',(#11558,#11559,#11560,#11561));
#2955=EDGE_LOOP('',(#11562,#11563,#11564,#11565));
#2956=EDGE_LOOP('',(#11566,#11567,#11568,#11569));
#2957=EDGE_LOOP('',(#11570,#11571,#11572,#11573));
#2958=EDGE_LOOP('',(#11574,#11575,#11576,#11577));
#2959=EDGE_LOOP('',(#11578,#11579,#11580,#11581));
#2960=EDGE_LOOP('',(#11582,#11583,#11584,#11585));
#2961=EDGE_LOOP('',(#11586,#11587,#11588,#11589));
#2962=EDGE_LOOP('',(#11590,#11591,#11592,#11593));
#2963=EDGE_LOOP('',(#11594,#11595,#11596,#11597));
#2964=EDGE_LOOP('',(#11598,#11599,#11600,#11601));
#2965=EDGE_LOOP('',(#11602,#11603,#11604,#11605));
#2966=EDGE_LOOP('',(#11606,#11607,#11608,#11609));
#2967=EDGE_LOOP('',(#11610,#11611,#11612,#11613));
#2968=EDGE_LOOP('',(#11614,#11615,#11616,#11617));
#2969=EDGE_LOOP('',(#11618,#11619,#11620,#11621));
#2970=EDGE_LOOP('',(#11622,#11623,#11624,#11625));
#2971=EDGE_LOOP('',(#11626,#11627,#11628,#11629));
#2972=EDGE_LOOP('',(#11630,#11631,#11632,#11633));
#2973=EDGE_LOOP('',(#11634,#11635,#11636,#11637));
#2974=EDGE_LOOP('',(#11638,#11639,#11640,#11641));
#2975=EDGE_LOOP('',(#11642,#11643,#11644,#11645));
#2976=EDGE_LOOP('',(#11646,#11647,#11648,#11649));
#2977=EDGE_LOOP('',(#11650,#11651,#11652,#11653));
#2978=EDGE_LOOP('',(#11654,#11655,#11656,#11657));
#2979=EDGE_LOOP('',(#11658,#11659,#11660,#11661));
#2980=EDGE_LOOP('',(#11662,#11663,#11664,#11665));
#2981=EDGE_LOOP('',(#11666,#11667,#11668,#11669));
#2982=EDGE_LOOP('',(#11670,#11671,#11672,#11673));
#2983=EDGE_LOOP('',(#11674,#11675,#11676,#11677));
#2984=EDGE_LOOP('',(#11678,#11679,#11680,#11681));
#2985=EDGE_LOOP('',(#11682,#11683,#11684,#11685));
#2986=EDGE_LOOP('',(#11686,#11687,#11688,#11689));
#2987=EDGE_LOOP('',(#11690,#11691,#11692,#11693));
#2988=EDGE_LOOP('',(#11694,#11695,#11696,#11697));
#2989=EDGE_LOOP('',(#11698,#11699,#11700,#11701));
#2990=EDGE_LOOP('',(#11702,#11703,#11704,#11705));
#2991=EDGE_LOOP('',(#11706,#11707,#11708,#11709));
#2992=EDGE_LOOP('',(#11710,#11711,#11712,#11713));
#2993=EDGE_LOOP('',(#11714,#11715,#11716,#11717,#11718));
#2994=EDGE_LOOP('',(#11719,#11720,#11721,#11722));
#2995=EDGE_LOOP('',(#11723,#11724,#11725,#11726));
#2996=EDGE_LOOP('',(#11727,#11728,#11729,#11730));
#2997=EDGE_LOOP('',(#11731,#11732,#11733,#11734));
#2998=EDGE_LOOP('',(#11735,#11736,#11737,#11738));
#2999=EDGE_LOOP('',(#11739,#11740,#11741,#11742));
#3000=EDGE_LOOP('',(#11743,#11744,#11745,#11746));
#3001=EDGE_LOOP('',(#11747,#11748,#11749,#11750));
#3002=EDGE_LOOP('',(#11751,#11752,#11753,#11754));
#3003=EDGE_LOOP('',(#11755,#11756,#11757,#11758));
#3004=EDGE_LOOP('',(#11759,#11760,#11761,#11762,#11763));
#3005=EDGE_LOOP('',(#11764,#11765,#11766,#11767,#11768,#11769));
#3006=EDGE_LOOP('',(#11770));
#3007=EDGE_LOOP('',(#11771));
#3008=EDGE_LOOP('',(#11772,#11773,#11774,#11775,#11776));
#3009=EDGE_LOOP('',(#11777));
#3010=EDGE_LOOP('',(#11778));
#3011=EDGE_LOOP('',(#11779,#11780,#11781,#11782,#11783));
#3012=EDGE_LOOP('',(#11784,#11785,#11786,#11787,#11788));
#3013=EDGE_LOOP('',(#11789));
#3014=EDGE_LOOP('',(#11790,#11791,#11792,#11793));
#3015=EDGE_LOOP('',(#11794,#11795,#11796,#11797,#11798,#11799));
#3016=EDGE_LOOP('',(#11800,#11801,#11802,#11803));
#3017=EDGE_LOOP('',(#11804,#11805,#11806,#11807));
#3018=EDGE_LOOP('',(#11808));
#3019=EDGE_LOOP('',(#11809));
#3020=EDGE_LOOP('',(#11810,#11811,#11812,#11813));
#3021=EDGE_LOOP('',(#11814,#11815,#11816,#11817,#11818,#11819,#11820,#11821,
#11822,#11823,#11824,#11825,#11826,#11827,#11828,#11829,#11830,#11831,#11832,
#11833,#11834,#11835,#11836,#11837,#11838));
#3022=EDGE_LOOP('',(#11839,#11840,#11841,#11842));
#3023=EDGE_LOOP('',(#11843,#11844,#11845,#11846,#11847,#11848,#11849,#11850,
#11851,#11852,#11853,#11854,#11855,#11856,#11857,#11858,#11859,#11860,#11861,
#11862,#11863,#11864,#11865,#11866));
#3024=EDGE_LOOP('',(#11867,#11868,#11869));
#3025=EDGE_LOOP('',(#11870,#11871,#11872,#11873,#11874,#11875,#11876,#11877,
#11878,#11879,#11880,#11881,#11882,#11883,#11884,#11885,#11886,#11887,#11888,
#11889,#11890,#11891,#11892,#11893,#11894,#11895,#11896,#11897,#11898,#11899,
#11900,#11901,#11902,#11903,#11904));
#3026=EDGE_LOOP('',(#11905,#11906,#11907,#11908,#11909));
#3027=EDGE_LOOP('',(#11910,#11911,#11912,#11913));
#3028=EDGE_LOOP('',(#11914,#11915,#11916,#11917,#11918,#11919,#11920,#11921,
#11922,#11923,#11924,#11925,#11926,#11927,#11928,#11929,#11930,#11931,#11932,
#11933,#11934,#11935,#11936,#11937,#11938,#11939,#11940,#11941,#11942,#11943,
#11944,#11945,#11946,#11947,#11948));
#3029=EDGE_LOOP('',(#11949,#11950,#11951,#11952));
#3030=EDGE_LOOP('',(#11953,#11954,#11955,#11956,#11957,#11958,#11959,#11960,
#11961,#11962,#11963));
#3031=EDGE_LOOP('',(#11964,#11965,#11966,#11967));
#3032=EDGE_LOOP('',(#11968,#11969,#11970,#11971));
#3033=EDGE_LOOP('',(#11972,#11973,#11974,#11975));
#3034=EDGE_LOOP('',(#11976,#11977,#11978,#11979));
#3035=EDGE_LOOP('',(#11980,#11981,#11982,#11983));
#3036=EDGE_LOOP('',(#11984));
#3037=EDGE_LOOP('',(#11985));
#3038=EDGE_LOOP('',(#11986,#11987,#11988,#11989));
#3039=EDGE_LOOP('',(#11990,#11991,#11992,#11993));
#3040=EDGE_LOOP('',(#11994,#11995,#11996,#11997));
#3041=EDGE_LOOP('',(#11998,#11999,#12000,#12001));
#3042=EDGE_LOOP('',(#12002,#12003,#12004,#12005,#12006));
#3043=EDGE_LOOP('',(#12007,#12008,#12009,#12010,#12011,#12012));
#3044=EDGE_LOOP('',(#12013));
#3045=EDGE_LOOP('',(#12014));
#3046=EDGE_LOOP('',(#12015,#12016,#12017,#12018));
#3047=EDGE_LOOP('',(#12019,#12020,#12021,#12022,#12023,#12024));
#3048=EDGE_LOOP('',(#12025,#12026,#12027,#12028,#12029,#12030,#12031,#12032));
#3049=EDGE_LOOP('',(#12033,#12034,#12035,#12036));
#3050=EDGE_LOOP('',(#12037));
#3051=EDGE_LOOP('',(#12038,#12039,#12040,#12041));
#3052=EDGE_LOOP('',(#12042));
#3053=EDGE_LOOP('',(#12043,#12044,#12045,#12046));
#3054=EDGE_LOOP('',(#12047));
#3055=EDGE_LOOP('',(#12048));
#3056=EDGE_LOOP('',(#12049,#12050,#12051,#12052,#12053,#12054));
#3057=EDGE_LOOP('',(#12055,#12056,#12057,#12058));
#3058=EDGE_LOOP('',(#12059));
#3059=EDGE_LOOP('',(#12060,#12061,#12062,#12063));
#3060=EDGE_LOOP('',(#12064,#12065,#12066,#12067));
#3061=EDGE_LOOP('',(#12068,#12069,#12070,#12071,#12072,#12073));
#3062=EDGE_LOOP('',(#12074,#12075,#12076,#12077));
#3063=EDGE_LOOP('',(#12078));
#3064=EDGE_LOOP('',(#12079));
#3065=EDGE_LOOP('',(#12080));
#3066=EDGE_LOOP('',(#12081,#12082,#12083,#12084));
#3067=EDGE_LOOP('',(#12085,#12086,#12087,#12088));
#3068=EDGE_LOOP('',(#12089));
#3069=EDGE_LOOP('',(#12090));
#3070=EDGE_LOOP('',(#12091,#12092,#12093,#12094));
#3071=EDGE_LOOP('',(#12095,#12096,#12097,#12098));
#3072=EDGE_LOOP('',(#12099));
#3073=EDGE_LOOP('',(#12100));
#3074=EDGE_LOOP('',(#12101,#12102,#12103,#12104));
#3075=EDGE_LOOP('',(#12105));
#3076=EDGE_LOOP('',(#12106));
#3077=EDGE_LOOP('',(#12107,#12108,#12109,#12110));
#3078=EDGE_LOOP('',(#12111));
#3079=EDGE_LOOP('',(#12112));
#3080=EDGE_LOOP('',(#12113,#12114,#12115,#12116));
#3081=EDGE_LOOP('',(#12117));
#3082=EDGE_LOOP('',(#12118));
#3083=EDGE_LOOP('',(#12119,#12120,#12121,#12122));
#3084=EDGE_LOOP('',(#12123,#12124,#12125,#12126));
#3085=EDGE_LOOP('',(#12127));
#3086=EDGE_LOOP('',(#12128,#12129,#12130,#12131));
#3087=EDGE_LOOP('',(#12132));
#3088=EDGE_LOOP('',(#12133));
#3089=EDGE_LOOP('',(#12134,#12135,#12136,#12137));
#3090=EDGE_LOOP('',(#12138,#12139,#12140,#12141));
#3091=EDGE_LOOP('',(#12142));
#3092=EDGE_LOOP('',(#12143));
#3093=EDGE_LOOP('',(#12144,#12145,#12146,#12147));
#3094=EDGE_LOOP('',(#12148));
#3095=EDGE_LOOP('',(#12149));
#3096=EDGE_LOOP('',(#12150));
#3097=EDGE_LOOP('',(#12151,#12152,#12153,#12154));
#3098=EDGE_LOOP('',(#12155,#12156,#12157,#12158));
#3099=EDGE_LOOP('',(#12159,#12160,#12161,#12162));
#3100=EDGE_LOOP('',(#12163));
#3101=EDGE_LOOP('',(#12164,#12165,#12166,#12167));
#3102=EDGE_LOOP('',(#12168,#12169,#12170,#12171,#12172,#12173));
#3103=EDGE_LOOP('',(#12174,#12175,#12176,#12177));
#3104=EDGE_LOOP('',(#12178,#12179,#12180,#12181));
#3105=EDGE_LOOP('',(#12182,#12183,#12184,#12185));
#3106=EDGE_LOOP('',(#12186,#12187,#12188,#12189,#12190,#12191));
#3107=EDGE_LOOP('',(#12192,#12193,#12194,#12195,#12196,#12197));
#3108=EDGE_LOOP('',(#12198,#12199,#12200,#12201));
#3109=EDGE_LOOP('',(#12202,#12203,#12204,#12205,#12206,#12207));
#3110=EDGE_LOOP('',(#12208,#12209,#12210,#12211,#12212));
#3111=EDGE_LOOP('',(#12213,#12214,#12215,#12216,#12217));
#3112=EDGE_LOOP('',(#12218,#12219,#12220,#12221));
#3113=EDGE_LOOP('',(#12222,#12223,#12224,#12225,#12226));
#3114=EDGE_LOOP('',(#12227,#12228,#12229,#12230,#12231,#12232));
#3115=EDGE_LOOP('',(#12233,#12234,#12235,#12236,#12237,#12238,#12239,#12240));
#3116=EDGE_LOOP('',(#12241,#12242,#12243,#12244,#12245,#12246));
#3117=EDGE_LOOP('',(#12247,#12248,#12249,#12250));
#3118=EDGE_LOOP('',(#12251,#12252,#12253,#12254,#12255,#12256));
#3119=EDGE_LOOP('',(#12257,#12258,#12259,#12260));
#3120=EDGE_LOOP('',(#12261,#12262,#12263,#12264));
#3121=EDGE_LOOP('',(#12265,#12266,#12267,#12268));
#3122=EDGE_LOOP('',(#12269,#12270,#12271,#12272,#12273,#12274));
#3123=EDGE_LOOP('',(#12275,#12276,#12277,#12278));
#3124=EDGE_LOOP('',(#12279,#12280,#12281,#12282,#12283));
#3125=EDGE_LOOP('',(#12284,#12285,#12286,#12287));
#3126=EDGE_LOOP('',(#12288,#12289,#12290,#12291,#12292,#12293,#12294,#12295));
#3127=EDGE_LOOP('',(#12296,#12297,#12298,#12299,#12300,#12301,#12302,#12303,
#12304,#12305,#12306,#12307,#12308,#12309,#12310,#12311,#12312,#12313,#12314));
#3128=EDGE_LOOP('',(#12315,#12316,#12317,#12318,#12319,#12320,#12321,#12322));
#3129=EDGE_LOOP('',(#12323,#12324,#12325,#12326,#12327,#12328,#12329,#12330,
#12331,#12332,#12333,#12334));
#3130=EDGE_LOOP('',(#12335,#12336,#12337,#12338,#12339,#12340,#12341,#12342,
#12343));
#3131=EDGE_LOOP('',(#12344,#12345,#12346,#12347,#12348,#12349,#12350,#12351,
#12352,#12353,#12354,#12355,#12356,#12357,#12358,#12359,#12360,#12361,#12362,
#12363,#12364,#12365,#12366,#12367,#12368,#12369,#12370,#12371,#12372));
#3132=EDGE_LOOP('',(#12373,#12374,#12375,#12376,#12377,#12378));
#3133=EDGE_LOOP('',(#12379,#12380,#12381,#12382,#12383,#12384));
#3134=EDGE_LOOP('',(#12385,#12386,#12387,#12388));
#3135=EDGE_LOOP('',(#12389,#12390,#12391,#12392));
#3136=EDGE_LOOP('',(#12393,#12394,#12395,#12396,#12397,#12398));
#3137=EDGE_LOOP('',(#12399,#12400,#12401,#12402,#12403,#12404));
#3138=EDGE_LOOP('',(#12405,#12406,#12407,#12408));
#3139=EDGE_LOOP('',(#12409,#12410,#12411,#12412));
#3140=EDGE_LOOP('',(#12413,#12414,#12415,#12416));
#3141=EDGE_LOOP('',(#12417,#12418,#12419,#12420));
#3142=EDGE_LOOP('',(#12421,#12422,#12423,#12424));
#3143=EDGE_LOOP('',(#12425,#12426,#12427,#12428));
#3144=EDGE_LOOP('',(#12429,#12430,#12431,#12432));
#3145=EDGE_LOOP('',(#12433,#12434,#12435,#12436));
#3146=EDGE_LOOP('',(#12437,#12438,#12439,#12440));
#3147=EDGE_LOOP('',(#12441,#12442,#12443,#12444));
#3148=EDGE_LOOP('',(#12445,#12446,#12447,#12448));
#3149=EDGE_LOOP('',(#12449,#12450,#12451,#12452));
#3150=EDGE_LOOP('',(#12453,#12454,#12455,#12456));
#3151=EDGE_LOOP('',(#12457,#12458,#12459,#12460));
#3152=EDGE_LOOP('',(#12461,#12462,#12463,#12464));
#3153=EDGE_LOOP('',(#12465,#12466,#12467,#12468));
#3154=EDGE_LOOP('',(#12469,#12470,#12471,#12472));
#3155=EDGE_LOOP('',(#12473,#12474,#12475,#12476));
#3156=EDGE_LOOP('',(#12477,#12478,#12479,#12480));
#3157=EDGE_LOOP('',(#12481,#12482,#12483,#12484));
#3158=EDGE_LOOP('',(#12485,#12486,#12487,#12488,#12489,#12490,#12491,#12492,
#12493,#12494,#12495,#12496,#12497,#12498,#12499,#12500,#12501,#12502,#12503));
#3159=EDGE_LOOP('',(#12504,#12505,#12506,#12507));
#3160=EDGE_LOOP('',(#12508,#12509,#12510,#12511));
#3161=EDGE_LOOP('',(#12512,#12513,#12514,#12515));
#3162=EDGE_LOOP('',(#12516,#12517,#12518,#12519));
#3163=EDGE_LOOP('',(#12520,#12521,#12522,#12523));
#3164=EDGE_LOOP('',(#12524,#12525,#12526,#12527));
#3165=EDGE_LOOP('',(#12528,#12529,#12530,#12531));
#3166=EDGE_LOOP('',(#12532,#12533,#12534,#12535));
#3167=EDGE_LOOP('',(#12536,#12537,#12538,#12539,#12540,#12541,#12542,#12543));
#3168=EDGE_LOOP('',(#12544,#12545,#12546,#12547));
#3169=EDGE_LOOP('',(#12548,#12549,#12550,#12551));
#3170=EDGE_LOOP('',(#12552,#12553,#12554,#12555));
#3171=EDGE_LOOP('',(#12556,#12557,#12558,#12559));
#3172=EDGE_LOOP('',(#12560,#12561,#12562,#12563));
#3173=EDGE_LOOP('',(#12564,#12565,#12566,#12567));
#3174=EDGE_LOOP('',(#12568,#12569,#12570,#12571));
#3175=EDGE_LOOP('',(#12572,#12573,#12574,#12575));
#3176=EDGE_LOOP('',(#12576,#12577,#12578,#12579));
#3177=EDGE_LOOP('',(#12580,#12581,#12582,#12583));
#3178=EDGE_LOOP('',(#12584,#12585,#12586,#12587));
#3179=EDGE_LOOP('',(#12588,#12589,#12590,#12591));
#3180=EDGE_LOOP('',(#12592,#12593,#12594,#12595,#12596,#12597,#12598,#12599,
#12600,#12601,#12602,#12603));
#3181=EDGE_LOOP('',(#12604,#12605,#12606,#12607));
#3182=EDGE_LOOP('',(#12608,#12609,#12610,#12611));
#3183=EDGE_LOOP('',(#12612,#12613,#12614,#12615));
#3184=EDGE_LOOP('',(#12616,#12617,#12618,#12619));
#3185=EDGE_LOOP('',(#12620,#12621,#12622,#12623));
#3186=EDGE_LOOP('',(#12624,#12625,#12626,#12627));
#3187=EDGE_LOOP('',(#12628,#12629,#12630,#12631));
#3188=EDGE_LOOP('',(#12632,#12633,#12634,#12635));
#3189=EDGE_LOOP('',(#12636,#12637,#12638,#12639));
#3190=EDGE_LOOP('',(#12640,#12641,#12642,#12643,#12644,#12645,#12646,#12647,
#12648));
#3191=EDGE_LOOP('',(#12649,#12650,#12651,#12652));
#3192=EDGE_LOOP('',(#12653,#12654,#12655,#12656));
#3193=EDGE_LOOP('',(#12657,#12658,#12659,#12660));
#3194=EDGE_LOOP('',(#12661,#12662,#12663,#12664));
#3195=EDGE_LOOP('',(#12665,#12666,#12667,#12668));
#3196=EDGE_LOOP('',(#12669,#12670,#12671,#12672));
#3197=EDGE_LOOP('',(#12673,#12674,#12675,#12676));
#3198=EDGE_LOOP('',(#12677,#12678,#12679,#12680));
#3199=EDGE_LOOP('',(#12681,#12682,#12683,#12684));
#3200=EDGE_LOOP('',(#12685,#12686,#12687,#12688));
#3201=EDGE_LOOP('',(#12689,#12690,#12691,#12692));
#3202=EDGE_LOOP('',(#12693,#12694,#12695,#12696));
#3203=EDGE_LOOP('',(#12697,#12698,#12699,#12700));
#3204=EDGE_LOOP('',(#12701,#12702,#12703,#12704));
#3205=EDGE_LOOP('',(#12705,#12706,#12707,#12708));
#3206=EDGE_LOOP('',(#12709,#12710,#12711,#12712));
#3207=EDGE_LOOP('',(#12713,#12714,#12715,#12716));
#3208=EDGE_LOOP('',(#12717,#12718,#12719,#12720));
#3209=EDGE_LOOP('',(#12721,#12722,#12723,#12724));
#3210=EDGE_LOOP('',(#12725,#12726,#12727,#12728));
#3211=EDGE_LOOP('',(#12729,#12730,#12731,#12732));
#3212=EDGE_LOOP('',(#12733,#12734,#12735,#12736));
#3213=EDGE_LOOP('',(#12737,#12738,#12739,#12740));
#3214=EDGE_LOOP('',(#12741,#12742,#12743,#12744));
#3215=EDGE_LOOP('',(#12745,#12746,#12747,#12748));
#3216=EDGE_LOOP('',(#12749,#12750,#12751,#12752));
#3217=EDGE_LOOP('',(#12753,#12754,#12755,#12756));
#3218=EDGE_LOOP('',(#12757,#12758,#12759,#12760));
#3219=EDGE_LOOP('',(#12761,#12762,#12763,#12764));
#3220=EDGE_LOOP('',(#12765,#12766,#12767,#12768,#12769,#12770,#12771,#12772,
#12773,#12774,#12775,#12776,#12777,#12778,#12779,#12780,#12781,#12782,#12783,
#12784,#12785,#12786,#12787,#12788,#12789,#12790,#12791,#12792,#12793));
#3221=EDGE_LOOP('',(#12794,#12795,#12796,#12797,#12798,#12799));
#3222=EDGE_LOOP('',(#12800,#12801,#12802,#12803,#12804,#12805));
#3223=EDGE_LOOP('',(#12806,#12807,#12808,#12809,#12810,#12811));
#3224=EDGE_LOOP('',(#12812,#12813,#12814,#12815));
#3225=EDGE_LOOP('',(#12816,#12817,#12818,#12819,#12820,#12821));
#3226=EDGE_LOOP('',(#12822,#12823,#12824,#12825));
#3227=EDGE_LOOP('',(#12826,#12827,#12828,#12829));
#3228=EDGE_LOOP('',(#12830));
#3229=EDGE_LOOP('',(#12831,#12832,#12833,#12834));
#3230=EDGE_LOOP('',(#12835,#12836,#12837,#12838));
#3231=EDGE_LOOP('',(#12839));
#3232=EDGE_LOOP('',(#12840));
#3233=EDGE_LOOP('',(#12841,#12842,#12843,#12844));
#3234=EDGE_LOOP('',(#12845));
#3235=EDGE_LOOP('',(#12846));
#3236=EDGE_LOOP('',(#12847,#12848,#12849,#12850));
#3237=EDGE_LOOP('',(#12851));
#3238=EDGE_LOOP('',(#12852));
#3239=EDGE_LOOP('',(#12853,#12854,#12855,#12856));
#3240=EDGE_LOOP('',(#12857));
#3241=EDGE_LOOP('',(#12858));
#3242=EDGE_LOOP('',(#12859,#12860,#12861,#12862));
#3243=EDGE_LOOP('',(#12863,#12864,#12865,#12866));
#3244=EDGE_LOOP('',(#12867));
#3245=EDGE_LOOP('',(#12868,#12869,#12870,#12871));
#3246=EDGE_LOOP('',(#12872,#12873,#12874,#12875));
#3247=EDGE_LOOP('',(#12876,#12877,#12878,#12879));
#3248=EDGE_LOOP('',(#12880,#12881,#12882,#12883));
#3249=EDGE_LOOP('',(#12884,#12885,#12886,#12887));
#3250=EDGE_LOOP('',(#12888,#12889,#12890,#12891));
#3251=EDGE_LOOP('',(#12892,#12893,#12894,#12895));
#3252=EDGE_LOOP('',(#12896,#12897,#12898,#12899));
#3253=EDGE_LOOP('',(#12900,#12901,#12902,#12903));
#3254=EDGE_LOOP('',(#12904,#12905,#12906,#12907));
#3255=EDGE_LOOP('',(#12908,#12909,#12910,#12911));
#3256=EDGE_LOOP('',(#12912,#12913,#12914,#12915));
#3257=EDGE_LOOP('',(#12916,#12917,#12918,#12919));
#3258=EDGE_LOOP('',(#12920,#12921,#12922,#12923));
#3259=EDGE_LOOP('',(#12924,#12925,#12926,#12927));
#3260=EDGE_LOOP('',(#12928,#12929,#12930,#12931));
#3261=EDGE_LOOP('',(#12932,#12933,#12934,#12935));
#3262=EDGE_LOOP('',(#12936,#12937,#12938,#12939));
#3263=EDGE_LOOP('',(#12940,#12941,#12942,#12943));
#3264=EDGE_LOOP('',(#12944,#12945,#12946,#12947));
#3265=EDGE_LOOP('',(#12948,#12949,#12950,#12951));
#3266=EDGE_LOOP('',(#12952,#12953,#12954,#12955));
#3267=EDGE_LOOP('',(#12956,#12957,#12958,#12959));
#3268=EDGE_LOOP('',(#12960,#12961,#12962,#12963,#12964));
#3269=EDGE_LOOP('',(#12965,#12966,#12967,#12968,#12969,#12970));
#3270=EDGE_LOOP('',(#12971));
#3271=EDGE_LOOP('',(#12972,#12973,#12974,#12975));
#3272=EDGE_LOOP('',(#12976,#12977,#12978,#12979,#12980,#12981));
#3273=EDGE_LOOP('',(#12982,#12983,#12984,#12985,#12986));
#3274=EDGE_LOOP('',(#12987,#12988,#12989,#12990,#12991));
#3275=EDGE_LOOP('',(#12992,#12993,#12994,#12995,#12996,#12997,#12998,#12999,
#13000,#13001,#13002,#13003,#13004,#13005,#13006,#13007,#13008,#13009,#13010,
#13011,#13012,#13013,#13014,#13015,#13016,#13017,#13018));
#3276=EDGE_LOOP('',(#13019,#13020,#13021,#13022));
#3277=EDGE_LOOP('',(#13023,#13024,#13025,#13026,#13027,#13028,#13029,#13030,
#13031,#13032,#13033,#13034,#13035,#13036,#13037,#13038,#13039,#13040,#13041,
#13042,#13043,#13044,#13045,#13046,#13047,#13048,#13049));
#3278=EDGE_LOOP('',(#13050,#13051,#13052,#13053));
#3279=EDGE_LOOP('',(#13054,#13055,#13056,#13057));
#3280=EDGE_LOOP('',(#13058));
#3281=EDGE_LOOP('',(#13059));
#3282=EDGE_LOOP('',(#13060,#13061,#13062,#13063));
#3283=EDGE_LOOP('',(#13064,#13065,#13066,#13067,#13068,#13069));
#3284=EDGE_LOOP('',(#13070));
#3285=EDGE_LOOP('',(#13071));
#3286=EDGE_LOOP('',(#13072,#13073,#13074,#13075));
#3287=EDGE_LOOP('',(#13076));
#3288=EDGE_LOOP('',(#13077));
#3289=EDGE_LOOP('',(#13078,#13079,#13080,#13081));
#3290=EDGE_LOOP('',(#13082));
#3291=EDGE_LOOP('',(#13083));
#3292=EDGE_LOOP('',(#13084,#13085,#13086,#13087));
#3293=EDGE_LOOP('',(#13088,#13089,#13090,#13091));
#3294=EDGE_LOOP('',(#13092,#13093,#13094,#13095));
#3295=EDGE_LOOP('',(#13096,#13097,#13098,#13099));
#3296=EDGE_LOOP('',(#13100,#13101,#13102,#13103));
#3297=EDGE_LOOP('',(#13104,#13105,#13106,#13107));
#3298=EDGE_LOOP('',(#13108,#13109,#13110,#13111));
#3299=EDGE_LOOP('',(#13112,#13113,#13114,#13115));
#3300=EDGE_LOOP('',(#13116,#13117,#13118,#13119));
#3301=EDGE_LOOP('',(#13120,#13121,#13122,#13123));
#3302=EDGE_LOOP('',(#13124,#13125,#13126,#13127));
#3303=EDGE_LOOP('',(#13128,#13129,#13130,#13131));
#3304=EDGE_LOOP('',(#13132,#13133,#13134,#13135));
#3305=EDGE_LOOP('',(#13136,#13137,#13138));
#3306=EDGE_LOOP('',(#13139,#13140,#13141,#13142,#13143));
#3307=EDGE_LOOP('',(#13144,#13145,#13146,#13147));
#3308=EDGE_LOOP('',(#13148,#13149,#13150,#13151));
#3309=EDGE_LOOP('',(#13152,#13153,#13154,#13155));
#3310=EDGE_LOOP('',(#13156,#13157,#13158,#13159));
#3311=EDGE_LOOP('',(#13160,#13161,#13162,#13163));
#3312=EDGE_LOOP('',(#13164,#13165,#13166,#13167));
#3313=EDGE_LOOP('',(#13168,#13169,#13170,#13171));
#3314=EDGE_LOOP('',(#13172,#13173,#13174,#13175));
#3315=EDGE_LOOP('',(#13176,#13177,#13178,#13179));
#3316=EDGE_LOOP('',(#13180,#13181,#13182,#13183));
#3317=EDGE_LOOP('',(#13184,#13185,#13186,#13187));
#3318=EDGE_LOOP('',(#13188,#13189,#13190,#13191,#13192,#13193));
#3319=EDGE_LOOP('',(#13194,#13195));
#3320=EDGE_LOOP('',(#13196,#13197,#13198,#13199,#13200,#13201));
#3321=EDGE_LOOP('',(#13202,#13203,#13204,#13205,#13206,#13207,#13208,#13209,
#13210,#13211,#13212,#13213,#13214,#13215,#13216,#13217,#13218,#13219,#13220,
#13221,#13222,#13223,#13224,#13225,#13226,#13227,#13228,#13229,#13230,#13231,
#13232,#13233));
#3322=EDGE_LOOP('',(#13234,#13235,#13236,#13237));
#3323=EDGE_LOOP('',(#13238,#13239,#13240,#13241));
#3324=EDGE_LOOP('',(#13242,#13243,#13244,#13245));
#3325=EDGE_LOOP('',(#13246,#13247,#13248,#13249));
#3326=EDGE_LOOP('',(#13250,#13251,#13252,#13253));
#3327=EDGE_LOOP('',(#13254,#13255,#13256,#13257));
#3328=EDGE_LOOP('',(#13258,#13259,#13260,#13261));
#3329=EDGE_LOOP('',(#13262,#13263,#13264,#13265));
#3330=EDGE_LOOP('',(#13266,#13267,#13268,#13269));
#3331=EDGE_LOOP('',(#13270,#13271,#13272,#13273));
#3332=EDGE_LOOP('',(#13274,#13275,#13276,#13277));
#3333=EDGE_LOOP('',(#13278,#13279,#13280,#13281));
#3334=EDGE_LOOP('',(#13282,#13283,#13284,#13285));
#3335=EDGE_LOOP('',(#13286,#13287,#13288,#13289));
#3336=EDGE_LOOP('',(#13290,#13291,#13292,#13293));
#3337=EDGE_LOOP('',(#13294,#13295,#13296,#13297));
#3338=EDGE_LOOP('',(#13298,#13299,#13300,#13301));
#3339=EDGE_LOOP('',(#13302,#13303,#13304,#13305));
#3340=EDGE_LOOP('',(#13306,#13307,#13308,#13309));
#3341=EDGE_LOOP('',(#13310,#13311,#13312,#13313));
#3342=EDGE_LOOP('',(#13314,#13315,#13316,#13317));
#3343=EDGE_LOOP('',(#13318,#13319,#13320,#13321,#13322));
#3344=EDGE_LOOP('',(#13323,#13324));
#3345=EDGE_LOOP('',(#13325,#13326,#13327,#13328,#13329,#13330,#13331,#13332,
#13333,#13334,#13335,#13336,#13337,#13338,#13339,#13340,#13341,#13342,#13343,
#13344,#13345,#13346,#13347,#13348,#13349,#13350,#13351,#13352,#13353));
#3346=EDGE_LOOP('',(#13354,#13355,#13356,#13357,#13358));
#3347=EDGE_LOOP('',(#13359,#13360,#13361,#13362));
#3348=EDGE_LOOP('',(#13363,#13364,#13365,#13366,#13367,#13368,#13369,#13370,
#13371,#13372,#13373,#13374,#13375,#13376,#13377,#13378,#13379,#13380,#13381,
#13382,#13383,#13384,#13385,#13386,#13387,#13388,#13389,#13390,#13391,#13392));
#3349=EDGE_LOOP('',(#13393,#13394,#13395,#13396));
#3350=EDGE_LOOP('',(#13397,#13398,#13399,#13400,#13401,#13402,#13403,#13404,
#13405,#13406));
#3351=EDGE_LOOP('',(#13407,#13408,#13409,#13410));
#3352=EDGE_LOOP('',(#13411,#13412,#13413,#13414));
#3353=EDGE_LOOP('',(#13415,#13416,#13417,#13418));
#3354=EDGE_LOOP('',(#13419,#13420,#13421));
#3355=EDGE_LOOP('',(#13422,#13423,#13424,#13425));
#3356=EDGE_LOOP('',(#13426,#13427,#13428));
#3357=EDGE_LOOP('',(#13429,#13430,#13431,#13432));
#3358=EDGE_LOOP('',(#13433,#13434,#13435));
#3359=EDGE_LOOP('',(#13436,#13437,#13438,#13439));
#3360=EDGE_LOOP('',(#13440,#13441,#13442));
#3361=EDGE_LOOP('',(#13443,#13444,#13445,#13446));
#3362=EDGE_LOOP('',(#13447,#13448,#13449));
#3363=EDGE_LOOP('',(#13450,#13451,#13452,#13453));
#3364=EDGE_LOOP('',(#13454,#13455,#13456));
#3365=EDGE_LOOP('',(#13457,#13458,#13459,#13460));
#3366=EDGE_LOOP('',(#13461,#13462,#13463));
#3367=EDGE_LOOP('',(#13464,#13465,#13466,#13467));
#3368=EDGE_LOOP('',(#13468,#13469,#13470));
#3369=EDGE_LOOP('',(#13471,#13472,#13473,#13474));
#3370=EDGE_LOOP('',(#13475,#13476,#13477));
#3371=EDGE_LOOP('',(#13478,#13479,#13480,#13481));
#3372=EDGE_LOOP('',(#13482,#13483,#13484));
#3373=EDGE_LOOP('',(#13485,#13486,#13487,#13488));
#3374=EDGE_LOOP('',(#13489,#13490,#13491));
#3375=EDGE_LOOP('',(#13492,#13493,#13494,#13495));
#3376=EDGE_LOOP('',(#13496,#13497,#13498));
#3377=EDGE_LOOP('',(#13499,#13500,#13501,#13502));
#3378=EDGE_LOOP('',(#13503,#13504,#13505));
#3379=EDGE_LOOP('',(#13506,#13507,#13508,#13509));
#3380=EDGE_LOOP('',(#13510,#13511,#13512));
#3381=EDGE_LOOP('',(#13513,#13514,#13515,#13516));
#3382=EDGE_LOOP('',(#13517,#13518,#13519));
#3383=EDGE_LOOP('',(#13520,#13521,#13522,#13523));
#3384=EDGE_LOOP('',(#13524,#13525,#13526));
#3385=EDGE_LOOP('',(#13527,#13528,#13529,#13530));
#3386=EDGE_LOOP('',(#13531,#13532,#13533));
#3387=EDGE_LOOP('',(#13534,#13535,#13536,#13537));
#3388=EDGE_LOOP('',(#13538,#13539,#13540));
#3389=EDGE_LOOP('',(#13541,#13542,#13543,#13544));
#3390=EDGE_LOOP('',(#13545,#13546,#13547));
#3391=EDGE_LOOP('',(#13548,#13549,#13550,#13551));
#3392=EDGE_LOOP('',(#13552,#13553,#13554));
#3393=EDGE_LOOP('',(#13555,#13556,#13557,#13558));
#3394=EDGE_LOOP('',(#13559,#13560,#13561));
#3395=EDGE_LOOP('',(#13562,#13563,#13564,#13565));
#3396=EDGE_LOOP('',(#13566,#13567,#13568,#13569));
#3397=EDGE_LOOP('',(#13570,#13571,#13572,#13573));
#3398=EDGE_LOOP('',(#13574,#13575,#13576,#13577));
#3399=EDGE_LOOP('',(#13578,#13579,#13580,#13581));
#3400=EDGE_LOOP('',(#13582,#13583,#13584));
#3401=EDGE_LOOP('',(#13585,#13586,#13587,#13588));
#3402=EDGE_LOOP('',(#13589,#13590,#13591));
#3403=EDGE_LOOP('',(#13592,#13593,#13594,#13595));
#3404=EDGE_LOOP('',(#13596,#13597,#13598));
#3405=EDGE_LOOP('',(#13599,#13600,#13601,#13602));
#3406=EDGE_LOOP('',(#13603,#13604,#13605));
#3407=EDGE_LOOP('',(#13606,#13607,#13608,#13609));
#3408=EDGE_LOOP('',(#13610,#13611,#13612));
#3409=EDGE_LOOP('',(#13613,#13614,#13615,#13616));
#3410=EDGE_LOOP('',(#13617,#13618,#13619));
#3411=EDGE_LOOP('',(#13620,#13621,#13622,#13623));
#3412=EDGE_LOOP('',(#13624,#13625,#13626));
#3413=EDGE_LOOP('',(#13627,#13628,#13629,#13630));
#3414=EDGE_LOOP('',(#13631,#13632,#13633));
#3415=EDGE_LOOP('',(#13634,#13635,#13636,#13637));
#3416=EDGE_LOOP('',(#13638,#13639,#13640));
#3417=EDGE_LOOP('',(#13641,#13642,#13643,#13644));
#3418=EDGE_LOOP('',(#13645,#13646,#13647));
#3419=EDGE_LOOP('',(#13648,#13649,#13650,#13651));
#3420=EDGE_LOOP('',(#13652,#13653,#13654));
#3421=EDGE_LOOP('',(#13655,#13656,#13657,#13658));
#3422=EDGE_LOOP('',(#13659,#13660,#13661,#13662));
#3423=EDGE_LOOP('',(#13663,#13664,#13665));
#3424=EDGE_LOOP('',(#13666,#13667,#13668,#13669));
#3425=EDGE_LOOP('',(#13670,#13671,#13672));
#3426=EDGE_LOOP('',(#13673,#13674,#13675,#13676));
#3427=EDGE_LOOP('',(#13677,#13678,#13679));
#3428=EDGE_LOOP('',(#13680,#13681,#13682,#13683));
#3429=EDGE_LOOP('',(#13684,#13685,#13686));
#3430=EDGE_LOOP('',(#13687,#13688,#13689,#13690));
#3431=EDGE_LOOP('',(#13691,#13692,#13693));
#3432=EDGE_LOOP('',(#13694,#13695,#13696,#13697));
#3433=EDGE_LOOP('',(#13698,#13699,#13700));
#3434=EDGE_LOOP('',(#13701,#13702,#13703,#13704));
#3435=EDGE_LOOP('',(#13705,#13706,#13707));
#3436=EDGE_LOOP('',(#13708,#13709,#13710,#13711));
#3437=EDGE_LOOP('',(#13712,#13713,#13714));
#3438=EDGE_LOOP('',(#13715,#13716,#13717,#13718));
#3439=EDGE_LOOP('',(#13719,#13720,#13721));
#3440=EDGE_LOOP('',(#13722,#13723,#13724,#13725));
#3441=EDGE_LOOP('',(#13726,#13727,#13728));
#3442=EDGE_LOOP('',(#13729,#13730,#13731,#13732));
#3443=EDGE_LOOP('',(#13733,#13734,#13735));
#3444=EDGE_LOOP('',(#13736,#13737,#13738,#13739));
#3445=EDGE_LOOP('',(#13740,#13741,#13742));
#3446=EDGE_LOOP('',(#13743));
#3447=EDGE_LOOP('',(#13744,#13745,#13746,#13747,#13748,#13749));
#3448=EDGE_LOOP('',(#13750,#13751,#13752,#13753));
#3449=EDGE_LOOP('',(#13754));
#3450=EDGE_LOOP('',(#13755,#13756,#13757,#13758,#13759));
#3451=EDGE_LOOP('',(#13760,#13761,#13762,#13763));
#3452=EDGE_LOOP('',(#13764,#13765,#13766,#13767));
#3453=EDGE_LOOP('',(#13768,#13769,#13770,#13771,#13772));
#3454=EDGE_LOOP('',(#13773,#13774,#13775,#13776,#13777));
#3455=EDGE_LOOP('',(#13778));
#3456=EDGE_LOOP('',(#13779));
#3457=EDGE_LOOP('',(#13780,#13781,#13782,#13783));
#3458=EDGE_LOOP('',(#13784));
#3459=EDGE_LOOP('',(#13785));
#3460=EDGE_LOOP('',(#13786,#13787,#13788,#13789));
#3461=EDGE_LOOP('',(#13790,#13791,#13792,#13793));
#3462=EDGE_LOOP('',(#13794,#13795,#13796,#13797));
#3463=EDGE_LOOP('',(#13798));
#3464=EDGE_LOOP('',(#13799));
#3465=EDGE_LOOP('',(#13800,#13801,#13802,#13803,#13804));
#3466=EDGE_LOOP('',(#13805,#13806,#13807,#13808,#13809,#13810));
#3467=EDGE_LOOP('',(#13811));
#3468=EDGE_LOOP('',(#13812,#13813,#13814,#13815,#13816,#13817));
#3469=EDGE_LOOP('',(#13818,#13819,#13820,#13821,#13822,#13823));
#3470=EDGE_LOOP('',(#13824,#13825,#13826,#13827,#13828,#13829));
#3471=EDGE_LOOP('',(#13830,#13831,#13832,#13833,#13834));
#3472=EDGE_LOOP('',(#13835,#13836,#13837,#13838));
#3473=EDGE_LOOP('',(#13839));
#3474=EDGE_LOOP('',(#13840));
#3475=EDGE_LOOP('',(#13841,#13842,#13843,#13844));
#3476=EDGE_LOOP('',(#13845));
#3477=EDGE_LOOP('',(#13846,#13847,#13848,#13849));
#3478=EDGE_LOOP('',(#13850,#13851,#13852,#13853));
#3479=EDGE_LOOP('',(#13854,#13855,#13856,#13857));
#3480=EDGE_LOOP('',(#13858,#13859,#13860,#13861));
#3481=EDGE_LOOP('',(#13862,#13863,#13864,#13865));
#3482=EDGE_LOOP('',(#13866,#13867,#13868,#13869));
#3483=EDGE_LOOP('',(#13870,#13871,#13872,#13873));
#3484=EDGE_LOOP('',(#13874,#13875,#13876,#13877));
#3485=EDGE_LOOP('',(#13878,#13879,#13880,#13881));
#3486=EDGE_LOOP('',(#13882,#13883,#13884,#13885));
#3487=EDGE_LOOP('',(#13886,#13887,#13888,#13889));
#3488=EDGE_LOOP('',(#13890,#13891,#13892,#13893));
#3489=EDGE_LOOP('',(#13894,#13895,#13896,#13897));
#3490=EDGE_LOOP('',(#13898,#13899,#13900,#13901));
#3491=EDGE_LOOP('',(#13902,#13903,#13904,#13905));
#3492=EDGE_LOOP('',(#13906,#13907,#13908,#13909));
#3493=EDGE_LOOP('',(#13910,#13911,#13912,#13913));
#3494=EDGE_LOOP('',(#13914,#13915,#13916,#13917));
#3495=EDGE_LOOP('',(#13918,#13919,#13920,#13921));
#3496=EDGE_LOOP('',(#13922,#13923,#13924,#13925));
#3497=EDGE_LOOP('',(#13926,#13927,#13928,#13929));
#3498=EDGE_LOOP('',(#13930,#13931,#13932,#13933));
#3499=EDGE_LOOP('',(#13934,#13935,#13936,#13937));
#3500=EDGE_LOOP('',(#13938,#13939,#13940,#13941));
#3501=EDGE_LOOP('',(#13942,#13943,#13944,#13945));
#3502=EDGE_LOOP('',(#13946,#13947,#13948,#13949));
#3503=EDGE_LOOP('',(#13950,#13951,#13952,#13953,#13954,#13955,#13956,#13957,
#13958,#13959,#13960,#13961,#13962,#13963,#13964,#13965,#13966,#13967,#13968,
#13969,#13970,#13971,#13972,#13973,#13974,#13975,#13976,#13977,#13978));
#3504=EDGE_LOOP('',(#13979,#13980,#13981,#13982,#13983));
#3505=EDGE_LOOP('',(#13984,#13985,#13986,#13987));
#3506=EDGE_LOOP('',(#13988,#13989,#13990,#13991,#13992,#13993,#13994,#13995,
#13996,#13997,#13998,#13999,#14000,#14001,#14002,#14003,#14004,#14005,#14006,
#14007,#14008,#14009,#14010,#14011,#14012,#14013,#14014,#14015,#14016));
#3507=EDGE_LOOP('',(#14017,#14018,#14019,#14020));
#3508=EDGE_LOOP('',(#14021));
#3509=EDGE_LOOP('',(#14022,#14023,#14024,#14025));
#3510=EDGE_LOOP('',(#14026,#14027,#14028,#14029));
#3511=EDGE_LOOP('',(#14030,#14031,#14032,#14033));
#3512=EDGE_LOOP('',(#14034,#14035,#14036,#14037));
#3513=EDGE_LOOP('',(#14038,#14039,#14040,#14041));
#3514=EDGE_LOOP('',(#14042,#14043,#14044,#14045));
#3515=EDGE_LOOP('',(#14046,#14047,#14048,#14049));
#3516=EDGE_LOOP('',(#14050,#14051,#14052,#14053));
#3517=EDGE_LOOP('',(#14054,#14055,#14056,#14057));
#3518=EDGE_LOOP('',(#14058,#14059,#14060,#14061));
#3519=EDGE_LOOP('',(#14062,#14063,#14064,#14065));
#3520=EDGE_LOOP('',(#14066,#14067,#14068,#14069,#14070,#14071,#14072,#14073,
#14074,#14075,#14076));
#3521=EDGE_LOOP('',(#14077,#14078,#14079,#14080));
#3522=EDGE_LOOP('',(#14081,#14082,#14083,#14084));
#3523=EDGE_LOOP('',(#14085,#14086,#14087,#14088));
#3524=EDGE_LOOP('',(#14089,#14090,#14091,#14092));
#3525=EDGE_LOOP('',(#14093,#14094,#14095,#14096));
#3526=EDGE_LOOP('',(#14097,#14098,#14099,#14100));
#3527=EDGE_LOOP('',(#14101,#14102,#14103,#14104));
#3528=EDGE_LOOP('',(#14105,#14106,#14107,#14108));
#3529=EDGE_LOOP('',(#14109,#14110,#14111,#14112));
#3530=EDGE_LOOP('',(#14113,#14114,#14115,#14116));
#3531=EDGE_LOOP('',(#14117,#14118,#14119,#14120,#14121,#14122,#14123,#14124,
#14125,#14126));
#3532=EDGE_LOOP('',(#14127,#14128,#14129,#14130));
#3533=EDGE_LOOP('',(#14131,#14132,#14133,#14134));
#3534=EDGE_LOOP('',(#14135,#14136,#14137,#14138));
#3535=EDGE_LOOP('',(#14139,#14140,#14141,#14142));
#3536=EDGE_LOOP('',(#14143,#14144,#14145,#14146));
#3537=EDGE_LOOP('',(#14147,#14148,#14149,#14150));
#3538=EDGE_LOOP('',(#14151,#14152,#14153,#14154));
#3539=EDGE_LOOP('',(#14155,#14156,#14157,#14158));
#3540=EDGE_LOOP('',(#14159,#14160,#14161,#14162));
#3541=EDGE_LOOP('',(#14163,#14164,#14165,#14166));
#3542=EDGE_LOOP('',(#14167,#14168,#14169,#14170));
#3543=EDGE_LOOP('',(#14171,#14172,#14173,#14174,#14175,#14176,#14177,#14178,
#14179,#14180,#14181));
#3544=EDGE_LOOP('',(#14182,#14183,#14184,#14185));
#3545=EDGE_LOOP('',(#14186,#14187,#14188,#14189));
#3546=EDGE_LOOP('',(#14190,#14191,#14192,#14193));
#3547=EDGE_LOOP('',(#14194,#14195,#14196,#14197));
#3548=EDGE_LOOP('',(#14198,#14199,#14200,#14201));
#3549=EDGE_LOOP('',(#14202,#14203,#14204,#14205));
#3550=EDGE_LOOP('',(#14206,#14207,#14208,#14209));
#3551=EDGE_LOOP('',(#14210,#14211,#14212,#14213));
#3552=EDGE_LOOP('',(#14214,#14215,#14216,#14217));
#3553=EDGE_LOOP('',(#14218,#14219,#14220,#14221));
#3554=EDGE_LOOP('',(#14222,#14223,#14224,#14225,#14226,#14227,#14228,#14229,
#14230,#14231));
#3555=EDGE_LOOP('',(#14232,#14233,#14234,#14235));
#3556=EDGE_LOOP('',(#14236,#14237,#14238,#14239));
#3557=EDGE_LOOP('',(#14240,#14241,#14242,#14243));
#3558=EDGE_LOOP('',(#14244,#14245,#14246,#14247));
#3559=EDGE_LOOP('',(#14248,#14249,#14250,#14251));
#3560=EDGE_LOOP('',(#14252,#14253,#14254,#14255));
#3561=EDGE_LOOP('',(#14256,#14257,#14258,#14259));
#3562=EDGE_LOOP('',(#14260,#14261,#14262,#14263));
#3563=EDGE_LOOP('',(#14264,#14265,#14266,#14267));
#3564=EDGE_LOOP('',(#14268,#14269,#14270,#14271));
#3565=EDGE_LOOP('',(#14272,#14273,#14274,#14275,#14276,#14277,#14278,#14279,
#14280,#14281));
#3566=EDGE_LOOP('',(#14282));
#3567=EDGE_LOOP('',(#14283));
#3568=EDGE_LOOP('',(#14284,#14285,#14286,#14287));
#3569=EDGE_LOOP('',(#14288,#14289,#14290,#14291));
#3570=EDGE_LOOP('',(#14292));
#3571=EDGE_LOOP('',(#14293,#14294,#14295,#14296));
#3572=EDGE_LOOP('',(#14297,#14298,#14299));
#3573=EDGE_LOOP('',(#14300,#14301,#14302,#14303));
#3574=EDGE_LOOP('',(#14304,#14305,#14306));
#3575=EDGE_LOOP('',(#14307,#14308,#14309,#14310));
#3576=EDGE_LOOP('',(#14311,#14312,#14313));
#3577=EDGE_LOOP('',(#14314,#14315,#14316,#14317));
#3578=EDGE_LOOP('',(#14318,#14319,#14320));
#3579=EDGE_LOOP('',(#14321,#14322,#14323,#14324));
#3580=EDGE_LOOP('',(#14325,#14326,#14327));
#3581=EDGE_LOOP('',(#14328,#14329,#14330,#14331));
#3582=EDGE_LOOP('',(#14332,#14333,#14334));
#3583=EDGE_LOOP('',(#14335,#14336,#14337,#14338));
#3584=EDGE_LOOP('',(#14339,#14340,#14341));
#3585=EDGE_LOOP('',(#14342,#14343,#14344,#14345));
#3586=EDGE_LOOP('',(#14346,#14347,#14348));
#3587=EDGE_LOOP('',(#14349,#14350,#14351,#14352));
#3588=EDGE_LOOP('',(#14353,#14354,#14355));
#3589=EDGE_LOOP('',(#14356,#14357,#14358,#14359));
#3590=EDGE_LOOP('',(#14360,#14361,#14362));
#3591=EDGE_LOOP('',(#14363,#14364,#14365,#14366));
#3592=EDGE_LOOP('',(#14367,#14368,#14369));
#3593=EDGE_LOOP('',(#14370,#14371,#14372,#14373));
#3594=EDGE_LOOP('',(#14374,#14375,#14376));
#3595=EDGE_LOOP('',(#14377,#14378,#14379,#14380));
#3596=EDGE_LOOP('',(#14381,#14382,#14383));
#3597=EDGE_LOOP('',(#14384,#14385,#14386,#14387));
#3598=EDGE_LOOP('',(#14388,#14389,#14390));
#3599=EDGE_LOOP('',(#14391,#14392,#14393,#14394));
#3600=EDGE_LOOP('',(#14395,#14396,#14397));
#3601=EDGE_LOOP('',(#14398,#14399,#14400,#14401));
#3602=EDGE_LOOP('',(#14402,#14403,#14404));
#3603=EDGE_LOOP('',(#14405,#14406,#14407,#14408));
#3604=EDGE_LOOP('',(#14409,#14410,#14411));
#3605=EDGE_LOOP('',(#14412,#14413,#14414,#14415));
#3606=EDGE_LOOP('',(#14416,#14417,#14418));
#3607=EDGE_LOOP('',(#14419,#14420,#14421,#14422));
#3608=EDGE_LOOP('',(#14423,#14424,#14425));
#3609=EDGE_LOOP('',(#14426,#14427,#14428,#14429));
#3610=EDGE_LOOP('',(#14430,#14431,#14432));
#3611=EDGE_LOOP('',(#14433,#14434,#14435,#14436));
#3612=EDGE_LOOP('',(#14437,#14438,#14439));
#3613=EDGE_LOOP('',(#14440,#14441,#14442,#14443));
#3614=EDGE_LOOP('',(#14444,#14445,#14446));
#3615=EDGE_LOOP('',(#14447,#14448,#14449,#14450));
#3616=EDGE_LOOP('',(#14451,#14452,#14453));
#3617=EDGE_LOOP('',(#14454,#14455,#14456,#14457));
#3618=EDGE_LOOP('',(#14458,#14459,#14460));
#3619=EDGE_LOOP('',(#14461,#14462,#14463,#14464));
#3620=EDGE_LOOP('',(#14465,#14466,#14467));
#3621=EDGE_LOOP('',(#14468,#14469,#14470,#14471));
#3622=EDGE_LOOP('',(#14472,#14473,#14474));
#3623=EDGE_LOOP('',(#14475,#14476,#14477,#14478));
#3624=EDGE_LOOP('',(#14479,#14480,#14481));
#3625=EDGE_LOOP('',(#14482,#14483,#14484,#14485));
#3626=EDGE_LOOP('',(#14486,#14487,#14488));
#3627=EDGE_LOOP('',(#14489,#14490,#14491,#14492));
#3628=EDGE_LOOP('',(#14493,#14494,#14495,#14496));
#3629=EDGE_LOOP('',(#14497,#14498,#14499,#14500));
#3630=EDGE_LOOP('',(#14501,#14502,#14503,#14504));
#3631=EDGE_LOOP('',(#14505,#14506,#14507,#14508));
#3632=EDGE_LOOP('',(#14509,#14510,#14511));
#3633=EDGE_LOOP('',(#14512,#14513,#14514,#14515));
#3634=EDGE_LOOP('',(#14516,#14517,#14518));
#3635=EDGE_LOOP('',(#14519,#14520,#14521,#14522));
#3636=EDGE_LOOP('',(#14523,#14524,#14525));
#3637=EDGE_LOOP('',(#14526,#14527,#14528,#14529));
#3638=EDGE_LOOP('',(#14530,#14531,#14532));
#3639=EDGE_LOOP('',(#14533,#14534,#14535,#14536));
#3640=EDGE_LOOP('',(#14537,#14538,#14539));
#3641=EDGE_LOOP('',(#14540,#14541,#14542,#14543));
#3642=EDGE_LOOP('',(#14544,#14545,#14546));
#3643=EDGE_LOOP('',(#14547,#14548,#14549,#14550));
#3644=EDGE_LOOP('',(#14551,#14552,#14553));
#3645=EDGE_LOOP('',(#14554,#14555,#14556,#14557));
#3646=EDGE_LOOP('',(#14558,#14559,#14560));
#3647=EDGE_LOOP('',(#14561,#14562,#14563,#14564));
#3648=EDGE_LOOP('',(#14565,#14566,#14567));
#3649=EDGE_LOOP('',(#14568,#14569,#14570,#14571));
#3650=EDGE_LOOP('',(#14572,#14573,#14574));
#3651=EDGE_LOOP('',(#14575,#14576,#14577,#14578));
#3652=EDGE_LOOP('',(#14579,#14580,#14581));
#3653=EDGE_LOOP('',(#14582,#14583,#14584,#14585));
#3654=EDGE_LOOP('',(#14586,#14587,#14588));
#3655=EDGE_LOOP('',(#14589,#14590,#14591,#14592));
#3656=EDGE_LOOP('',(#14593,#14594,#14595));
#3657=EDGE_LOOP('',(#14596,#14597,#14598,#14599));
#3658=EDGE_LOOP('',(#14600,#14601,#14602));
#3659=EDGE_LOOP('',(#14603,#14604,#14605,#14606));
#3660=EDGE_LOOP('',(#14607,#14608,#14609));
#3661=EDGE_LOOP('',(#14610,#14611,#14612,#14613));
#3662=EDGE_LOOP('',(#14614,#14615,#14616));
#3663=EDGE_LOOP('',(#14617,#14618,#14619,#14620));
#3664=EDGE_LOOP('',(#14621,#14622,#14623));
#3665=EDGE_LOOP('',(#14624,#14625,#14626,#14627));
#3666=EDGE_LOOP('',(#14628,#14629,#14630));
#3667=EDGE_LOOP('',(#14631,#14632,#14633,#14634));
#3668=EDGE_LOOP('',(#14635,#14636,#14637));
#3669=EDGE_LOOP('',(#14638,#14639,#14640,#14641));
#3670=EDGE_LOOP('',(#14642,#14643,#14644));
#3671=EDGE_LOOP('',(#14645,#14646,#14647,#14648));
#3672=EDGE_LOOP('',(#14649,#14650,#14651));
#3673=EDGE_LOOP('',(#14652,#14653,#14654,#14655));
#3674=EDGE_LOOP('',(#14656,#14657,#14658));
#3675=EDGE_LOOP('',(#14659,#14660,#14661,#14662));
#3676=EDGE_LOOP('',(#14663,#14664,#14665));
#3677=EDGE_LOOP('',(#14666,#14667,#14668,#14669));
#3678=EDGE_LOOP('',(#14670,#14671,#14672));
#3679=EDGE_LOOP('',(#14673,#14674,#14675,#14676));
#3680=EDGE_LOOP('',(#14677,#14678,#14679));
#3681=EDGE_LOOP('',(#14680,#14681,#14682,#14683));
#3682=EDGE_LOOP('',(#14684,#14685,#14686));
#3683=EDGE_LOOP('',(#14687,#14688,#14689,#14690));
#3684=EDGE_LOOP('',(#14691,#14692,#14693));
#3685=EDGE_LOOP('',(#14694,#14695,#14696,#14697));
#3686=EDGE_LOOP('',(#14698,#14699,#14700));
#3687=EDGE_LOOP('',(#14701,#14702,#14703,#14704));
#3688=EDGE_LOOP('',(#14705,#14706,#14707));
#3689=EDGE_LOOP('',(#14708,#14709,#14710,#14711));
#3690=EDGE_LOOP('',(#14712,#14713,#14714));
#3691=EDGE_LOOP('',(#14715));
#3692=EDGE_LOOP('',(#14716,#14717,#14718,#14719));
#3693=EDGE_LOOP('',(#14720,#14721,#14722,#14723,#14724,#14725));
#3694=EDGE_LOOP('',(#14726,#14727,#14728,#14729));
#3695=EDGE_LOOP('',(#14730,#14731,#14732,#14733));
#3696=EDGE_LOOP('',(#14734));
#3697=EDGE_LOOP('',(#14735));
#3698=EDGE_LOOP('',(#14736,#14737,#14738,#14739));
#3699=EDGE_LOOP('',(#14740,#14741,#14742,#14743,#14744,#14745,#14746,#14747,
#14748,#14749,#14750,#14751));
#3700=EDGE_LOOP('',(#14752,#14753,#14754,#14755));
#3701=EDGE_LOOP('',(#14756,#14757,#14758,#14759));
#3702=EDGE_LOOP('',(#14760,#14761,#14762,#14763));
#3703=EDGE_LOOP('',(#14764,#14765,#14766,#14767));
#3704=EDGE_LOOP('',(#14768,#14769,#14770,#14771));
#3705=EDGE_LOOP('',(#14772,#14773,#14774,#14775));
#3706=EDGE_LOOP('',(#14776,#14777,#14778,#14779));
#3707=EDGE_LOOP('',(#14780,#14781,#14782,#14783));
#3708=EDGE_LOOP('',(#14784,#14785,#14786,#14787));
#3709=EDGE_LOOP('',(#14788,#14789,#14790,#14791));
#3710=EDGE_LOOP('',(#14792,#14793,#14794,#14795));
#3711=EDGE_LOOP('',(#14796,#14797,#14798,#14799));
#3712=EDGE_LOOP('',(#14800,#14801,#14802,#14803));
#3713=EDGE_LOOP('',(#14804,#14805,#14806,#14807));
#3714=EDGE_LOOP('',(#14808,#14809,#14810,#14811));
#3715=EDGE_LOOP('',(#14812,#14813,#14814,#14815));
#3716=EDGE_LOOP('',(#14816,#14817,#14818,#14819));
#3717=EDGE_LOOP('',(#14820,#14821,#14822,#14823));
#3718=EDGE_LOOP('',(#14824,#14825,#14826,#14827));
#3719=EDGE_LOOP('',(#14828,#14829,#14830,#14831));
#3720=EDGE_LOOP('',(#14832,#14833,#14834,#14835));
#3721=EDGE_LOOP('',(#14836,#14837,#14838,#14839));
#3722=EDGE_LOOP('',(#14840,#14841,#14842,#14843));
#3723=EDGE_LOOP('',(#14844,#14845,#14846,#14847));
#3724=EDGE_LOOP('',(#14848,#14849,#14850,#14851));
#3725=EDGE_LOOP('',(#14852,#14853,#14854,#14855));
#3726=EDGE_LOOP('',(#14856,#14857,#14858,#14859));
#3727=EDGE_LOOP('',(#14860,#14861,#14862,#14863));
#3728=EDGE_LOOP('',(#14864,#14865,#14866,#14867));
#3729=EDGE_LOOP('',(#14868,#14869,#14870,#14871));
#3730=EDGE_LOOP('',(#14872));
#3731=EDGE_LOOP('',(#14873,#14874,#14875,#14876,#14877,#14878,#14879,#14880,
#14881,#14882,#14883));
#3732=EDGE_LOOP('',(#14884,#14885,#14886,#14887,#14888,#14889,#14890,#14891,
#14892,#14893));
#3733=EDGE_LOOP('',(#14894,#14895,#14896,#14897,#14898,#14899,#14900,#14901,
#14902,#14903,#14904));
#3734=EDGE_LOOP('',(#14905,#14906,#14907,#14908,#14909,#14910,#14911,#14912,
#14913,#14914));
#3735=EDGE_LOOP('',(#14915,#14916,#14917,#14918,#14919,#14920,#14921,#14922,
#14923,#14924));
#3736=EDGE_LOOP('',(#14925));
#3737=EDGE_LOOP('',(#14926,#14927,#14928,#14929));
#3738=EDGE_LOOP('',(#14930,#14931,#14932,#14933));
#3739=EDGE_LOOP('',(#14934,#14935,#14936,#14937));
#3740=EDGE_LOOP('',(#14938,#14939,#14940,#14941));
#3741=EDGE_LOOP('',(#14942,#14943,#14944,#14945,#14946));
#3742=EDGE_LOOP('',(#14947,#14948,#14949,#14950));
#3743=EDGE_LOOP('',(#14951,#14952,#14953,#14954));
#3744=EDGE_LOOP('',(#14955,#14956,#14957));
#3745=EDGE_LOOP('',(#14958,#14959,#14960,#14961,#14962,#14963,#14964,#14965,
#14966));
#3746=EDGE_LOOP('',(#14967));
#3747=EDGE_LOOP('',(#14968));
#3748=EDGE_LOOP('',(#14969,#14970,#14971,#14972,#14973));
#3749=EDGE_LOOP('',(#14974,#14975,#14976));
#3750=EDGE_LOOP('',(#14977,#14978,#14979,#14980));
#3751=EDGE_LOOP('',(#14981,#14982,#14983,#14984));
#3752=EDGE_LOOP('',(#14985,#14986,#14987,#14988,#14989,#14990));
#3753=EDGE_LOOP('',(#14991,#14992,#14993,#14994));
#3754=EDGE_LOOP('',(#14995,#14996,#14997,#14998));
#3755=EDGE_LOOP('',(#14999,#15000,#15001,#15002));
#3756=EDGE_LOOP('',(#15003,#15004,#15005,#15006,#15007,#15008,#15009,#15010));
#3757=EDGE_LOOP('',(#15011,#15012,#15013,#15014));
#3758=EDGE_LOOP('',(#15015,#15016,#15017,#15018));
#3759=EDGE_LOOP('',(#15019,#15020,#15021,#15022));
#3760=EDGE_LOOP('',(#15023,#15024,#15025,#15026,#15027,#15028));
#3761=EDGE_LOOP('',(#15029,#15030,#15031,#15032,#15033,#15034,#15035));
#3762=EDGE_LOOP('',(#15036));
#3763=EDGE_LOOP('',(#15037));
#3764=EDGE_LOOP('',(#15038,#15039,#15040,#15041,#15042,#15043));
#3765=EDGE_LOOP('',(#15044,#15045,#15046,#15047,#15048,#15049,#15050));
#3766=EDGE_LOOP('',(#15051,#15052,#15053,#15054));
#3767=EDGE_LOOP('',(#15055,#15056,#15057,#15058));
#3768=EDGE_LOOP('',(#15059,#15060,#15061,#15062,#15063));
#3769=EDGE_LOOP('',(#15064,#15065,#15066,#15067,#15068,#15069,#15070,#15071,
#15072));
#3770=EDGE_LOOP('',(#15073));
#3771=EDGE_LOOP('',(#15074));
#3772=EDGE_LOOP('',(#15075,#15076,#15077,#15078,#15079,#15080,#15081,#15082,
#15083,#15084));
#3773=EDGE_LOOP('',(#15085,#15086,#15087,#15088));
#3774=EDGE_LOOP('',(#15089,#15090,#15091,#15092));
#3775=EDGE_LOOP('',(#15093,#15094,#15095,#15096));
#3776=EDGE_LOOP('',(#15097,#15098,#15099,#15100));
#3777=EDGE_LOOP('',(#15101,#15102,#15103,#15104));
#3778=EDGE_LOOP('',(#15105,#15106,#15107,#15108,#15109));
#3779=EDGE_LOOP('',(#15110,#15111,#15112,#15113,#15114));
#3780=EDGE_LOOP('',(#15115,#15116,#15117,#15118,#15119,#15120));
#3781=EDGE_LOOP('',(#15121,#15122,#15123,#15124));
#3782=EDGE_LOOP('',(#15125,#15126,#15127,#15128));
#3783=EDGE_LOOP('',(#15129,#15130,#15131,#15132,#15133,#15134,#15135));
#3784=EDGE_LOOP('',(#15136));
#3785=EDGE_LOOP('',(#15137));
#3786=EDGE_LOOP('',(#15138,#15139,#15140,#15141,#15142));
#3787=EDGE_LOOP('',(#15143,#15144,#15145,#15146));
#3788=EDGE_LOOP('',(#15147,#15148,#15149,#15150));
#3789=EDGE_LOOP('',(#15151,#15152,#15153,#15154));
#3790=EDGE_LOOP('',(#15155,#15156,#15157,#15158));
#3791=EDGE_LOOP('',(#15159,#15160,#15161,#15162));
#3792=EDGE_LOOP('',(#15163,#15164,#15165,#15166));
#3793=EDGE_LOOP('',(#15167,#15168,#15169,#15170));
#3794=EDGE_LOOP('',(#15171,#15172,#15173,#15174));
#3795=EDGE_LOOP('',(#15175,#15176,#15177,#15178,#15179,#15180,#15181,#15182,
#15183,#15184));
#3796=EDGE_LOOP('',(#15185,#15186,#15187,#15188));
#3797=EDGE_LOOP('',(#15189));
#3798=EDGE_LOOP('',(#15190,#15191));
#3799=EDGE_LOOP('',(#15192,#15193,#15194,#15195));
#3800=EDGE_LOOP('',(#15196,#15197,#15198,#15199));
#3801=EDGE_LOOP('',(#15200,#15201,#15202,#15203));
#3802=EDGE_LOOP('',(#15204,#15205,#15206,#15207));
#3803=EDGE_LOOP('',(#15208,#15209,#15210,#15211));
#3804=EDGE_LOOP('',(#15212,#15213,#15214,#15215));
#3805=EDGE_LOOP('',(#15216));
#3806=EDGE_LOOP('',(#15217));
#3807=EDGE_LOOP('',(#15218,#15219,#15220,#15221,#15222));
#3808=EDGE_LOOP('',(#15223,#15224,#15225,#15226,#15227,#15228));
#3809=EDGE_LOOP('',(#15229));
#3810=EDGE_LOOP('',(#15230));
#3811=EDGE_LOOP('',(#15231,#15232,#15233,#15234));
#3812=EDGE_LOOP('',(#15235,#15236,#15237,#15238));
#3813=EDGE_LOOP('',(#15239,#15240,#15241,#15242,#15243));
#3814=EDGE_LOOP('',(#15244,#15245,#15246,#15247));
#3815=EDGE_LOOP('',(#15248,#15249,#15250,#15251));
#3816=EDGE_LOOP('',(#15252,#15253,#15254,#15255));
#3817=EDGE_LOOP('',(#15256,#15257,#15258,#15259));
#3818=EDGE_LOOP('',(#15260,#15261,#15262,#15263));
#3819=EDGE_LOOP('',(#15264,#15265,#15266,#15267));
#3820=EDGE_LOOP('',(#15268,#15269,#15270,#15271));
#3821=EDGE_LOOP('',(#15272));
#3822=EDGE_LOOP('',(#15273));
#3823=EDGE_LOOP('',(#15274,#15275,#15276,#15277));
#3824=EDGE_LOOP('',(#15278,#15279,#15280,#15281));
#3825=EDGE_LOOP('',(#15282,#15283,#15284,#15285));
#3826=EDGE_LOOP('',(#15286,#15287,#15288,#15289));
#3827=EDGE_LOOP('',(#15290,#15291,#15292,#15293));
#3828=EDGE_LOOP('',(#15294,#15295,#15296,#15297));
#3829=EDGE_LOOP('',(#15298,#15299,#15300,#15301));
#3830=EDGE_LOOP('',(#15302,#15303,#15304,#15305));
#3831=EDGE_LOOP('',(#15306,#15307,#15308,#15309));
#3832=EDGE_LOOP('',(#15310,#15311,#15312,#15313));
#3833=EDGE_LOOP('',(#15314,#15315,#15316,#15317));
#3834=EDGE_LOOP('',(#15318,#15319,#15320,#15321));
#3835=EDGE_LOOP('',(#15322));
#3836=EDGE_LOOP('',(#15323));
#3837=EDGE_LOOP('',(#15324,#15325,#15326,#15327));
#3838=EDGE_LOOP('',(#15328,#15329,#15330,#15331));
#3839=EDGE_LOOP('',(#15332,#15333,#15334,#15335));
#3840=EDGE_LOOP('',(#15336,#15337,#15338,#15339));
#3841=EDGE_LOOP('',(#15340,#15341,#15342,#15343));
#3842=EDGE_LOOP('',(#15344));
#3843=EDGE_LOOP('',(#15345,#15346,#15347,#15348));
#3844=EDGE_LOOP('',(#15349,#15350,#15351,#15352));
#3845=EDGE_LOOP('',(#15353));
#3846=EDGE_LOOP('',(#15354));
#3847=EDGE_LOOP('',(#15355,#15356,#15357,#15358));
#3848=EDGE_LOOP('',(#15359));
#3849=EDGE_LOOP('',(#15360));
#3850=EDGE_LOOP('',(#15361,#15362,#15363,#15364));
#3851=EDGE_LOOP('',(#15365));
#3852=EDGE_LOOP('',(#15366));
#3853=EDGE_LOOP('',(#15367,#15368,#15369,#15370));
#3854=EDGE_LOOP('',(#15371));
#3855=EDGE_LOOP('',(#15372));
#3856=EDGE_LOOP('',(#15373,#15374,#15375,#15376));
#3857=EDGE_LOOP('',(#15377,#15378,#15379,#15380));
#3858=EDGE_LOOP('',(#15381));
#3859=EDGE_LOOP('',(#15382,#15383,#15384,#15385));
#3860=EDGE_LOOP('',(#15386,#15387,#15388,#15389));
#3861=EDGE_LOOP('',(#15390,#15391,#15392,#15393));
#3862=EDGE_LOOP('',(#15394,#15395,#15396,#15397));
#3863=EDGE_LOOP('',(#15398,#15399,#15400,#15401));
#3864=EDGE_LOOP('',(#15402,#15403,#15404,#15405));
#3865=EDGE_LOOP('',(#15406,#15407,#15408,#15409));
#3866=EDGE_LOOP('',(#15410));
#3867=EDGE_LOOP('',(#15411,#15412,#15413,#15414));
#3868=EDGE_LOOP('',(#15415,#15416,#15417,#15418));
#3869=EDGE_LOOP('',(#15419,#15420,#15421,#15422));
#3870=EDGE_LOOP('',(#15423,#15424,#15425,#15426));
#3871=EDGE_LOOP('',(#15427,#15428,#15429,#15430));
#3872=EDGE_LOOP('',(#15431,#15432,#15433,#15434));
#3873=EDGE_LOOP('',(#15435));
#3874=EDGE_LOOP('',(#15436,#15437,#15438,#15439));
#3875=EDGE_LOOP('',(#15440,#15441,#15442,#15443));
#3876=EDGE_LOOP('',(#15444));
#3877=EDGE_LOOP('',(#15445));
#3878=EDGE_LOOP('',(#15446,#15447,#15448,#15449));
#3879=EDGE_LOOP('',(#15450,#15451,#15452,#15453));
#3880=EDGE_LOOP('',(#15454,#15455,#15456,#15457));
#3881=EDGE_LOOP('',(#15458,#15459,#15460,#15461));
#3882=EDGE_LOOP('',(#15462,#15463,#15464,#15465));
#3883=EDGE_LOOP('',(#15466,#15467,#15468,#15469));
#3884=EDGE_LOOP('',(#15470,#15471,#15472,#15473));
#3885=EDGE_LOOP('',(#15474,#15475,#15476,#15477));
#3886=LINE('',#22172,#5197);
#3887=LINE('',#22177,#5198);
#3888=LINE('',#22184,#5199);
#3889=LINE('',#22190,#5200);
#3890=LINE('',#22192,#5201);
#3891=LINE('',#22194,#5202);
#3892=LINE('',#22198,#5203);
#3893=LINE('',#22200,#5204);
#3894=LINE('',#22204,#5205);
#3895=LINE('',#22205,#5206);
#3896=LINE('',#22348,#5207);
#3897=LINE('',#22376,#5208);
#3898=LINE('',#22386,#5209);
#3899=LINE('',#22387,#5210);
#3900=LINE('',#22390,#5211);
#3901=LINE('',#22392,#5212);
#3902=LINE('',#22394,#5213);
#3903=LINE('',#22396,#5214);
#3904=LINE('',#22398,#5215);
#3905=LINE('',#22400,#5216);
#3906=LINE('',#22402,#5217);
#3907=LINE('',#22406,#5218);
#3908=LINE('',#22410,#5219);
#3909=LINE('',#22412,#5220);
#3910=LINE('',#22413,#5221);
#3911=LINE('',#22416,#5222);
#3912=LINE('',#22422,#5223);
#3913=LINE('',#22424,#5224);
#3914=LINE('',#22425,#5225);
#3915=LINE('',#22568,#5226);
#3916=LINE('',#22711,#5227);
#3917=LINE('',#22734,#5228);
#3918=LINE('',#22757,#5229);
#3919=LINE('',#22764,#5230);
#3920=LINE('',#22796,#5231);
#3921=LINE('',#22798,#5232);
#3922=LINE('',#22800,#5233);
#3923=LINE('',#22801,#5234);
#3924=LINE('',#22844,#5235);
#3925=LINE('',#22851,#5236);
#3926=LINE('',#22902,#5237);
#3927=LINE('',#22933,#5238);
#3928=LINE('',#22936,#5239);
#3929=LINE('',#22939,#5240);
#3930=LINE('',#22941,#5241);
#3931=LINE('',#22942,#5242);
#3932=LINE('',#22945,#5243);
#3933=LINE('',#22949,#5244);
#3934=LINE('',#22950,#5245);
#3935=LINE('',#22956,#5246);
#3936=LINE('',#22959,#5247);
#3937=LINE('',#22969,#5248);
#3938=LINE('',#22983,#5249);
#3939=LINE('',#22986,#5250);
#3940=LINE('',#22998,#5251);
#3941=LINE('',#23001,#5252);
#3942=LINE('',#23002,#5253);
#3943=LINE('',#23019,#5254);
#3944=LINE('',#23035,#5255);
#3945=LINE('',#23036,#5256);
#3946=LINE('',#23048,#5257);
#3947=LINE('',#23050,#5258);
#3948=LINE('',#23065,#5259);
#3949=LINE('',#23066,#5260);
#3950=LINE('',#23068,#5261);
#3951=LINE('',#23069,#5262);
#3952=LINE('',#23080,#5263);
#3953=LINE('',#23082,#5264);
#3954=LINE('',#23083,#5265);
#3955=LINE('',#23092,#5266);
#3956=LINE('',#23100,#5267);
#3957=LINE('',#23109,#5268);
#3958=LINE('',#23110,#5269);
#3959=LINE('',#23114,#5270);
#3960=LINE('',#23161,#5271);
#3961=LINE('',#23163,#5272);
#3962=LINE('',#23165,#5273);
#3963=LINE('',#23167,#5274);
#3964=LINE('',#23169,#5275);
#3965=LINE('',#23171,#5276);
#3966=LINE('',#23173,#5277);
#3967=LINE('',#23174,#5278);
#3968=LINE('',#23241,#5279);
#3969=LINE('',#23243,#5280);
#3970=LINE('',#23245,#5281);
#3971=LINE('',#23247,#5282);
#3972=LINE('',#23249,#5283);
#3973=LINE('',#23251,#5284);
#3974=LINE('',#23253,#5285);
#3975=LINE('',#23255,#5286);
#3976=LINE('',#23257,#5287);
#3977=LINE('',#23258,#5288);
#3978=LINE('',#23260,#5289);
#3979=LINE('',#23265,#5290);
#3980=LINE('',#23268,#5291);
#3981=LINE('',#23270,#5292);
#3982=LINE('',#23273,#5293);
#3983=LINE('',#23276,#5294);
#3984=LINE('',#23292,#5295);
#3985=LINE('',#23299,#5296);
#3986=LINE('',#23330,#5297);
#3987=LINE('',#23353,#5298);
#3988=LINE('',#23370,#5299);
#3989=LINE('',#23379,#5300);
#3990=LINE('',#23380,#5301);
#3991=LINE('',#23383,#5302);
#3992=LINE('',#23384,#5303);
#3993=LINE('',#23387,#5304);
#3994=LINE('',#23400,#5305);
#3995=LINE('',#23414,#5306);
#3996=LINE('',#23427,#5307);
#3997=LINE('',#23442,#5308);
#3998=LINE('',#23445,#5309);
#3999=LINE('',#23448,#5310);
#4000=LINE('',#23457,#5311);
#4001=LINE('',#23460,#5312);
#4002=LINE('',#23468,#5313);
#4003=LINE('',#23497,#5314);
#4004=LINE('',#23514,#5315);
#4005=LINE('',#23518,#5316);
#4006=LINE('',#23520,#5317);
#4007=LINE('',#23529,#5318);
#4008=LINE('',#23534,#5319);
#4009=LINE('',#23542,#5320);
#4010=LINE('',#23553,#5321);
#4011=LINE('',#23564,#5322);
#4012=LINE('',#23575,#5323);
#4013=LINE('',#23586,#5324);
#4014=LINE('',#23597,#5325);
#4015=LINE('',#23608,#5326);
#4016=LINE('',#23619,#5327);
#4017=LINE('',#23630,#5328);
#4018=LINE('',#23646,#5329);
#4019=LINE('',#23648,#5330);
#4020=LINE('',#23649,#5331);
#4021=LINE('',#23652,#5332);
#4022=LINE('',#23653,#5333);
#4023=LINE('',#23656,#5334);
#4024=LINE('',#23657,#5335);
#4025=LINE('',#23660,#5336);
#4026=LINE('',#23661,#5337);
#4027=LINE('',#23664,#5338);
#4028=LINE('',#23665,#5339);
#4029=LINE('',#23668,#5340);
#4030=LINE('',#23669,#5341);
#4031=LINE('',#23672,#5342);
#4032=LINE('',#23673,#5343);
#4033=LINE('',#23675,#5344);
#4034=LINE('',#23684,#5345);
#4035=LINE('',#23689,#5346);
#4036=LINE('',#23697,#5347);
#4037=LINE('',#23708,#5348);
#4038=LINE('',#23719,#5349);
#4039=LINE('',#23730,#5350);
#4040=LINE('',#23741,#5351);
#4041=LINE('',#23752,#5352);
#4042=LINE('',#23763,#5353);
#4043=LINE('',#23774,#5354);
#4044=LINE('',#23785,#5355);
#4045=LINE('',#23796,#5356);
#4046=LINE('',#23807,#5357);
#4047=LINE('',#23818,#5358);
#4048=LINE('',#23829,#5359);
#4049=LINE('',#23840,#5360);
#4050=LINE('',#23856,#5361);
#4051=LINE('',#23858,#5362);
#4052=LINE('',#23859,#5363);
#4053=LINE('',#23862,#5364);
#4054=LINE('',#23863,#5365);
#4055=LINE('',#23866,#5366);
#4056=LINE('',#23867,#5367);
#4057=LINE('',#23870,#5368);
#4058=LINE('',#23871,#5369);
#4059=LINE('',#23874,#5370);
#4060=LINE('',#23875,#5371);
#4061=LINE('',#23878,#5372);
#4062=LINE('',#23879,#5373);
#4063=LINE('',#23882,#5374);
#4064=LINE('',#23883,#5375);
#4065=LINE('',#23886,#5376);
#4066=LINE('',#23887,#5377);
#4067=LINE('',#23890,#5378);
#4068=LINE('',#23891,#5379);
#4069=LINE('',#23893,#5380);
#4070=LINE('',#23897,#5381);
#4071=LINE('',#23903,#5382);
#4072=LINE('',#23905,#5383);
#4073=LINE('',#23913,#5384);
#4074=LINE('',#23946,#5385);
#4075=LINE('',#24030,#5386);
#4076=LINE('',#24120,#5387);
#4077=LINE('',#24210,#5388);
#4078=LINE('',#24294,#5389);
#4079=LINE('',#24384,#5390);
#4080=LINE('',#24468,#5391);
#4081=LINE('',#24558,#5392);
#4082=LINE('',#24648,#5393);
#4083=LINE('',#24732,#5394);
#4084=LINE('',#24822,#5395);
#4085=LINE('',#24912,#5396);
#4086=LINE('',#24996,#5397);
#4087=LINE('',#25086,#5398);
#4088=LINE('',#25170,#5399);
#4089=LINE('',#25260,#5400);
#4090=LINE('',#25294,#5401);
#4091=LINE('',#25331,#5402);
#4092=LINE('',#25368,#5403);
#4093=LINE('',#25405,#5404);
#4094=LINE('',#25442,#5405);
#4095=LINE('',#25480,#5406);
#4096=LINE('',#25517,#5407);
#4097=LINE('',#25554,#5408);
#4098=LINE('',#25592,#5409);
#4099=LINE('',#25629,#5410);
#4100=LINE('',#25666,#5411);
#4101=LINE('',#25703,#5412);
#4102=LINE('',#25740,#5413);
#4103=LINE('',#25778,#5414);
#4104=LINE('',#25815,#5415);
#4105=LINE('',#25848,#5416);
#4106=LINE('',#25938,#5417);
#4107=LINE('',#26022,#5418);
#4108=LINE('',#26112,#5419);
#4109=LINE('',#26202,#5420);
#4110=LINE('',#26292,#5421);
#4111=LINE('',#26376,#5422);
#4112=LINE('',#26466,#5423);
#4113=LINE('',#26556,#5424);
#4114=LINE('',#26643,#5425);
#4115=LINE('',#26726,#5426);
#4116=LINE('',#26751,#5427);
#4117=LINE('',#26789,#5428);
#4118=LINE('',#26826,#5429);
#4119=LINE('',#26864,#5430);
#4120=LINE('',#26901,#5431);
#4121=LINE('',#26938,#5432);
#4122=LINE('',#26976,#5433);
#4123=LINE('',#27014,#5434);
#4124=LINE('',#27051,#5435);
#4125=LINE('',#27089,#5436);
#4126=LINE('',#27098,#5437);
#4127=LINE('',#27104,#5438);
#4128=LINE('',#27113,#5439);
#4129=LINE('',#27119,#5440);
#4130=LINE('',#27407,#5441);
#4131=LINE('',#27426,#5442);
#4132=LINE('',#27429,#5443);
#4133=LINE('',#31073,#5444);
#4134=LINE('',#31085,#5445);
#4135=LINE('',#31088,#5446);
#4136=LINE('',#31141,#5447);
#4137=LINE('',#31154,#5448);
#4138=LINE('',#31168,#5449);
#4139=LINE('',#31169,#5450);
#4140=LINE('',#31172,#5451);
#4141=LINE('',#31184,#5452);
#4142=LINE('',#31189,#5453);
#4143=LINE('',#31196,#5454);
#4144=LINE('',#31200,#5455);
#4145=LINE('',#31204,#5456);
#4146=LINE('',#31208,#5457);
#4147=LINE('',#31212,#5458);
#4148=LINE('',#31304,#5459);
#4149=LINE('',#31308,#5460);
#4150=LINE('',#31310,#5461);
#4151=LINE('',#31311,#5462);
#4152=LINE('',#31316,#5463);
#4153=LINE('',#31322,#5464);
#4154=LINE('',#31329,#5465);
#4155=LINE('',#31331,#5466);
#4156=LINE('',#31337,#5467);
#4157=LINE('',#31346,#5468);
#4158=LINE('',#31350,#5469);
#4159=LINE('',#31357,#5470);
#4160=LINE('',#31361,#5471);
#4161=LINE('',#31368,#5472);
#4162=LINE('',#31375,#5473);
#4163=LINE('',#31382,#5474);
#4164=LINE('',#31389,#5475);
#4165=LINE('',#31393,#5476);
#4166=LINE('',#32237,#5477);
#4167=LINE('',#32245,#5478);
#4168=LINE('',#32254,#5479);
#4169=LINE('',#32258,#5480);
#4170=LINE('',#32262,#5481);
#4171=LINE('',#32268,#5482);
#4172=LINE('',#32270,#5483);
#4173=LINE('',#32272,#5484);
#4174=LINE('',#32273,#5485);
#4175=LINE('',#32276,#5486);
#4176=LINE('',#32278,#5487);
#4177=LINE('',#32280,#5488);
#4178=LINE('',#32282,#5489);
#4179=LINE('',#32283,#5490);
#4180=LINE('',#32286,#5491);
#4181=LINE('',#32287,#5492);
#4182=LINE('',#32291,#5493);
#4183=LINE('',#32293,#5494);
#4184=LINE('',#32295,#5495);
#4185=LINE('',#32296,#5496);
#4186=LINE('',#32299,#5497);
#4187=LINE('',#32301,#5498);
#4188=LINE('',#32302,#5499);
#4189=LINE('',#32304,#5500);
#4190=LINE('',#32306,#5501);
#4191=LINE('',#32308,#5502);
#4192=LINE('',#32309,#5503);
#4193=LINE('',#32313,#5504);
#4194=LINE('',#32315,#5505);
#4195=LINE('',#32317,#5506);
#4196=LINE('',#32319,#5507);
#4197=LINE('',#32321,#5508);
#4198=LINE('',#32322,#5509);
#4199=LINE('',#32325,#5510);
#4200=LINE('',#32327,#5511);
#4201=LINE('',#32328,#5512);
#4202=LINE('',#32331,#5513);
#4203=LINE('',#32333,#5514);
#4204=LINE('',#32335,#5515);
#4205=LINE('',#32336,#5516);
#4206=LINE('',#32339,#5517);
#4207=LINE('',#32341,#5518);
#4208=LINE('',#32342,#5519);
#4209=LINE('',#32346,#5520);
#4210=LINE('',#32348,#5521);
#4211=LINE('',#32350,#5522);
#4212=LINE('',#32352,#5523);
#4213=LINE('',#32353,#5524);
#4214=LINE('',#32356,#5525);
#4215=LINE('',#32358,#5526);
#4216=LINE('',#32359,#5527);
#4217=LINE('',#32362,#5528);
#4218=LINE('',#32363,#5529);
#4219=LINE('',#32364,#5530);
#4220=LINE('',#32367,#5531);
#4221=LINE('',#32369,#5532);
#4222=LINE('',#32371,#5533);
#4223=LINE('',#32373,#5534);
#4224=LINE('',#32374,#5535);
#4225=LINE('',#32377,#5536);
#4226=LINE('',#32379,#5537);
#4227=LINE('',#32381,#5538);
#4228=LINE('',#32382,#5539);
#4229=LINE('',#32385,#5540);
#4230=LINE('',#32386,#5541);
#4231=LINE('',#32390,#5542);
#4232=LINE('',#32392,#5543);
#4233=LINE('',#32394,#5544);
#4234=LINE('',#32395,#5545);
#4235=LINE('',#32398,#5546);
#4236=LINE('',#32400,#5547);
#4237=LINE('',#32401,#5548);
#4238=LINE('',#32402,#5549);
#4239=LINE('',#32403,#5550);
#4240=LINE('',#32406,#5551);
#4241=LINE('',#32407,#5552);
#4242=LINE('',#32410,#5553);
#4243=LINE('',#32411,#5554);
#4244=LINE('',#32413,#5555);
#4245=LINE('',#32416,#5556);
#4246=LINE('',#32417,#5557);
#4247=LINE('',#32419,#5558);
#4248=LINE('',#32423,#5559);
#4249=LINE('',#32425,#5560);
#4250=LINE('',#32427,#5561);
#4251=LINE('',#32429,#5562);
#4252=LINE('',#32430,#5563);
#4253=LINE('',#32432,#5564);
#4254=LINE('',#32433,#5565);
#4255=LINE('',#32435,#5566);
#4256=LINE('',#32442,#5567);
#4257=LINE('',#32444,#5568);
#4258=LINE('',#32446,#5569);
#4259=LINE('',#32448,#5570);
#4260=LINE('',#32450,#5571);
#4261=LINE('',#32460,#5572);
#4262=LINE('',#32462,#5573);
#4263=LINE('',#32464,#5574);
#4264=LINE('',#32474,#5575);
#4265=LINE('',#32476,#5576);
#4266=LINE('',#32478,#5577);
#4267=LINE('',#32480,#5578);
#4268=LINE('',#32482,#5579);
#4269=LINE('',#32488,#5580);
#4270=LINE('',#32490,#5581);
#4271=LINE('',#32492,#5582);
#4272=LINE('',#32494,#5583);
#4273=LINE('',#32496,#5584);
#4274=LINE('',#32498,#5585);
#4275=LINE('',#32500,#5586);
#4276=LINE('',#32501,#5587);
#4277=LINE('',#32556,#5588);
#4278=LINE('',#32558,#5589);
#4279=LINE('',#32560,#5590);
#4280=LINE('',#32562,#5591);
#4281=LINE('',#32572,#5592);
#4282=LINE('',#32582,#5593);
#4283=LINE('',#32584,#5594);
#4284=LINE('',#32586,#5595);
#4285=LINE('',#32588,#5596);
#4286=LINE('',#32590,#5597);
#4287=LINE('',#32636,#5598);
#4288=LINE('',#32682,#5599);
#4289=LINE('',#32684,#5600);
#4290=LINE('',#32686,#5601);
#4291=LINE('',#32687,#5602);
#4292=LINE('',#32689,#5603);
#4293=LINE('',#32690,#5604);
#4294=LINE('',#32692,#5605);
#4295=LINE('',#32695,#5606);
#4296=LINE('',#32696,#5607);
#4297=LINE('',#32698,#5608);
#4298=LINE('',#32699,#5609);
#4299=LINE('',#32701,#5610);
#4300=LINE('',#32710,#5611);
#4301=LINE('',#32715,#5612);
#4302=LINE('',#32723,#5613);
#4303=LINE('',#32729,#5614);
#4304=LINE('',#32730,#5615);
#4305=LINE('',#32733,#5616);
#4306=LINE('',#32734,#5617);
#4307=LINE('',#32737,#5618);
#4308=LINE('',#32738,#5619);
#4309=LINE('',#32741,#5620);
#4310=LINE('',#32742,#5621);
#4311=LINE('',#32745,#5622);
#4312=LINE('',#32746,#5623);
#4313=LINE('',#32754,#5624);
#4314=LINE('',#32765,#5625);
#4315=LINE('',#32771,#5626);
#4316=LINE('',#32772,#5627);
#4317=LINE('',#32775,#5628);
#4318=LINE('',#32776,#5629);
#4319=LINE('',#32779,#5630);
#4320=LINE('',#32780,#5631);
#4321=LINE('',#32788,#5632);
#4322=LINE('',#32799,#5633);
#4323=LINE('',#32805,#5634);
#4324=LINE('',#32806,#5635);
#4325=LINE('',#32809,#5636);
#4326=LINE('',#32810,#5637);
#4327=LINE('',#32813,#5638);
#4328=LINE('',#32814,#5639);
#4329=LINE('',#32817,#5640);
#4330=LINE('',#32818,#5641);
#4331=LINE('',#32820,#5642);
#4332=LINE('',#32824,#5643);
#4333=LINE('',#32826,#5644);
#4334=LINE('',#32827,#5645);
#4335=LINE('',#32830,#5646);
#4336=LINE('',#32831,#5647);
#4337=LINE('',#32834,#5648);
#4338=LINE('',#32835,#5649);
#4339=LINE('',#32838,#5650);
#4340=LINE('',#32839,#5651);
#4341=LINE('',#32842,#5652);
#4342=LINE('',#32843,#5653);
#4343=LINE('',#32846,#5654);
#4344=LINE('',#32847,#5655);
#4345=LINE('',#32850,#5656);
#4346=LINE('',#32851,#5657);
#4347=LINE('',#32853,#5658);
#4348=LINE('',#32862,#5659);
#4349=LINE('',#32867,#5660);
#4350=LINE('',#32875,#5661);
#4351=LINE('',#32886,#5662);
#4352=LINE('',#32897,#5663);
#4353=LINE('',#32908,#5664);
#4354=LINE('',#32919,#5665);
#4355=LINE('',#32930,#5666);
#4356=LINE('',#32941,#5667);
#4357=LINE('',#32952,#5668);
#4358=LINE('',#32963,#5669);
#4359=LINE('',#32974,#5670);
#4360=LINE('',#32995,#5671);
#4361=LINE('',#33000,#5672);
#4362=LINE('',#33008,#5673);
#4363=LINE('',#33014,#5674);
#4364=LINE('',#33015,#5675);
#4365=LINE('',#33023,#5676);
#4366=LINE('',#33034,#5677);
#4367=LINE('',#33040,#5678);
#4368=LINE('',#33041,#5679);
#4369=LINE('',#33044,#5680);
#4370=LINE('',#33045,#5681);
#4371=LINE('',#33048,#5682);
#4372=LINE('',#33049,#5683);
#4373=LINE('',#33051,#5684);
#4374=LINE('',#33060,#5685);
#4375=LINE('',#33065,#5686);
#4376=LINE('',#33073,#5687);
#4377=LINE('',#33084,#5688);
#4378=LINE('',#33095,#5689);
#4379=LINE('',#33106,#5690);
#4380=LINE('',#33117,#5691);
#4381=LINE('',#33128,#5692);
#4382=LINE('',#33139,#5693);
#4383=LINE('',#33150,#5694);
#4384=LINE('',#33161,#5695);
#4385=LINE('',#33172,#5696);
#4386=LINE('',#33183,#5697);
#4387=LINE('',#33189,#5698);
#4388=LINE('',#33190,#5699);
#4389=LINE('',#33198,#5700);
#4390=LINE('',#33209,#5701);
#4391=LINE('',#33220,#5702);
#4392=LINE('',#33231,#5703);
#4393=LINE('',#33242,#5704);
#4394=LINE('',#33253,#5705);
#4395=LINE('',#33264,#5706);
#4396=LINE('',#33275,#5707);
#4397=LINE('',#33286,#5708);
#4398=LINE('',#33297,#5709);
#4399=LINE('',#33308,#5710);
#4400=LINE('',#33314,#5711);
#4401=LINE('',#33315,#5712);
#4402=LINE('',#33318,#5713);
#4403=LINE('',#33319,#5714);
#4404=LINE('',#33322,#5715);
#4405=LINE('',#33323,#5716);
#4406=LINE('',#33326,#5717);
#4407=LINE('',#33327,#5718);
#4408=LINE('',#33329,#5719);
#4409=LINE('',#33332,#5720);
#4410=LINE('',#33333,#5721);
#4411=LINE('',#33335,#5722);
#4412=LINE('',#33338,#5723);
#4413=LINE('',#33341,#5724);
#4414=LINE('',#33350,#5725);
#4415=LINE('',#33354,#5726);
#4416=LINE('',#33361,#5727);
#4417=LINE('',#33368,#5728);
#4418=LINE('',#33375,#5729);
#4419=LINE('',#33382,#5730);
#4420=LINE('',#33386,#5731);
#4421=LINE('',#33392,#5732);
#4422=LINE('',#33425,#5733);
#4423=LINE('',#33509,#5734);
#4424=LINE('',#33599,#5735);
#4425=LINE('',#33689,#5736);
#4426=LINE('',#33773,#5737);
#4427=LINE('',#33863,#5738);
#4428=LINE('',#33953,#5739);
#4429=LINE('',#34037,#5740);
#4430=LINE('',#34127,#5741);
#4431=LINE('',#34217,#5742);
#4432=LINE('',#34301,#5743);
#4433=LINE('',#34391,#5744);
#4434=LINE('',#34425,#5745);
#4435=LINE('',#34462,#5746);
#4436=LINE('',#34499,#5747);
#4437=LINE('',#34537,#5748);
#4438=LINE('',#34574,#5749);
#4439=LINE('',#34611,#5750);
#4440=LINE('',#34649,#5751);
#4441=LINE('',#34686,#5752);
#4442=LINE('',#34723,#5753);
#4443=LINE('',#34761,#5754);
#4444=LINE('',#34799,#5755);
#4445=LINE('',#34805,#5756);
#4446=LINE('',#35075,#5757);
#4447=LINE('',#35081,#5758);
#4448=LINE('',#36632,#5759);
#4449=LINE('',#36638,#5760);
#4450=LINE('',#36642,#5761);
#4451=LINE('',#36648,#5762);
#4452=LINE('',#36655,#5763);
#4453=LINE('',#36662,#5764);
#4454=LINE('',#36695,#5765);
#4455=LINE('',#36779,#5766);
#4456=LINE('',#36869,#5767);
#4457=LINE('',#36959,#5768);
#4458=LINE('',#37043,#5769);
#4459=LINE('',#37133,#5770);
#4460=LINE('',#37220,#5771);
#4461=LINE('',#37307,#5772);
#4462=LINE('',#37397,#5773);
#4463=LINE('',#37481,#5774);
#4464=LINE('',#37571,#5775);
#4465=LINE('',#37661,#5776);
#4466=LINE('',#37745,#5777);
#4467=LINE('',#37755,#5778);
#4468=LINE('',#37791,#5779);
#4469=LINE('',#37828,#5780);
#4470=LINE('',#37866,#5781);
#4471=LINE('',#37903,#5782);
#4472=LINE('',#37940,#5783);
#4473=LINE('',#37978,#5784);
#4474=LINE('',#38014,#5785);
#4475=LINE('',#38052,#5786);
#4476=LINE('',#38089,#5787);
#4477=LINE('',#38126,#5788);
#4478=LINE('',#38164,#5789);
#4479=LINE('',#38205,#5790);
#4480=LINE('',#38213,#5791);
#4481=LINE('',#38224,#5792);
#4482=LINE('',#38232,#5793);
#4483=LINE('',#38237,#5794);
#4484=LINE('',#38241,#5795);
#4485=LINE('',#38245,#5796);
#4486=LINE('',#38248,#5797);
#4487=LINE('',#38252,#5798);
#4488=LINE('',#38256,#5799);
#4489=LINE('',#38260,#5800);
#4490=LINE('',#38265,#5801);
#4491=LINE('',#38269,#5802);
#4492=LINE('',#38273,#5803);
#4493=LINE('',#38277,#5804);
#4494=LINE('',#38280,#5805);
#4495=LINE('',#38283,#5806);
#4496=LINE('',#38287,#5807);
#4497=LINE('',#38291,#5808);
#4498=LINE('',#38295,#5809);
#4499=LINE('',#38299,#5810);
#4500=LINE('',#38303,#5811);
#4501=LINE('',#38307,#5812);
#4502=LINE('',#38311,#5813);
#4503=LINE('',#38315,#5814);
#4504=LINE('',#38319,#5815);
#4505=LINE('',#38323,#5816);
#4506=LINE('',#38327,#5817);
#4507=LINE('',#38331,#5818);
#4508=LINE('',#38335,#5819);
#4509=LINE('',#38339,#5820);
#4510=LINE('',#38343,#5821);
#4511=LINE('',#38347,#5822);
#4512=LINE('',#38351,#5823);
#4513=LINE('',#38355,#5824);
#4514=LINE('',#38359,#5825);
#4515=LINE('',#38363,#5826);
#4516=LINE('',#38367,#5827);
#4517=LINE('',#38371,#5828);
#4518=LINE('',#38375,#5829);
#4519=LINE('',#38379,#5830);
#4520=LINE('',#38383,#5831);
#4521=LINE('',#38387,#5832);
#4522=LINE('',#38391,#5833);
#4523=LINE('',#38395,#5834);
#4524=LINE('',#38399,#5835);
#4525=LINE('',#38403,#5836);
#4526=LINE('',#38407,#5837);
#4527=LINE('',#38411,#5838);
#4528=LINE('',#38415,#5839);
#4529=LINE('',#38419,#5840);
#4530=LINE('',#38423,#5841);
#4531=LINE('',#38427,#5842);
#4532=LINE('',#38431,#5843);
#4533=LINE('',#38435,#5844);
#4534=LINE('',#38439,#5845);
#4535=LINE('',#38443,#5846);
#4536=LINE('',#38447,#5847);
#4537=LINE('',#40269,#5848);
#4538=LINE('',#40271,#5849);
#4539=LINE('',#40273,#5850);
#4540=LINE('',#40274,#5851);
#4541=LINE('',#40276,#5852);
#4542=LINE('',#40277,#5853);
#4543=LINE('',#40281,#5854);
#4544=LINE('',#40282,#5855);
#4545=LINE('',#40285,#5856);
#4546=LINE('',#40287,#5857);
#4547=LINE('',#40288,#5858);
#4548=LINE('',#40290,#5859);
#4549=LINE('',#40292,#5860);
#4550=LINE('',#40296,#5861);
#4551=LINE('',#40298,#5862);
#4552=LINE('',#40299,#5863);
#4553=LINE('',#40301,#5864);
#4554=LINE('',#40303,#5865);
#4555=LINE('',#40307,#5866);
#4556=LINE('',#40309,#5867);
#4557=LINE('',#40310,#5868);
#4558=LINE('',#40312,#5869);
#4559=LINE('',#40314,#5870);
#4560=LINE('',#40318,#5871);
#4561=LINE('',#40320,#5872);
#4562=LINE('',#40321,#5873);
#4563=LINE('',#40323,#5874);
#4564=LINE('',#40325,#5875);
#4565=LINE('',#40329,#5876);
#4566=LINE('',#40331,#5877);
#4567=LINE('',#40332,#5878);
#4568=LINE('',#40334,#5879);
#4569=LINE('',#40336,#5880);
#4570=LINE('',#40339,#5881);
#4571=LINE('',#40343,#5882);
#4572=LINE('',#40345,#5883);
#4573=LINE('',#40346,#5884);
#4574=LINE('',#40348,#5885);
#4575=LINE('',#40350,#5886);
#4576=LINE('',#40354,#5887);
#4577=LINE('',#40356,#5888);
#4578=LINE('',#40357,#5889);
#4579=LINE('',#40359,#5890);
#4580=LINE('',#40361,#5891);
#4581=LINE('',#40365,#5892);
#4582=LINE('',#40367,#5893);
#4583=LINE('',#40368,#5894);
#4584=LINE('',#40370,#5895);
#4585=LINE('',#40372,#5896);
#4586=LINE('',#40376,#5897);
#4587=LINE('',#40378,#5898);
#4588=LINE('',#40379,#5899);
#4589=LINE('',#40381,#5900);
#4590=LINE('',#40383,#5901);
#4591=LINE('',#40387,#5902);
#4592=LINE('',#40389,#5903);
#4593=LINE('',#40390,#5904);
#4594=LINE('',#40392,#5905);
#4595=LINE('',#40394,#5906);
#4596=LINE('',#40398,#5907);
#4597=LINE('',#40400,#5908);
#4598=LINE('',#40401,#5909);
#4599=LINE('',#40403,#5910);
#4600=LINE('',#40405,#5911);
#4601=LINE('',#40409,#5912);
#4602=LINE('',#40411,#5913);
#4603=LINE('',#40412,#5914);
#4604=LINE('',#40414,#5915);
#4605=LINE('',#40416,#5916);
#4606=LINE('',#40420,#5917);
#4607=LINE('',#40422,#5918);
#4608=LINE('',#40423,#5919);
#4609=LINE('',#40425,#5920);
#4610=LINE('',#40427,#5921);
#4611=LINE('',#40431,#5922);
#4612=LINE('',#40433,#5923);
#4613=LINE('',#40434,#5924);
#4614=LINE('',#40436,#5925);
#4615=LINE('',#40438,#5926);
#4616=LINE('',#40442,#5927);
#4617=LINE('',#40444,#5928);
#4618=LINE('',#40445,#5929);
#4619=LINE('',#40447,#5930);
#4620=LINE('',#40449,#5931);
#4621=LINE('',#40453,#5932);
#4622=LINE('',#40455,#5933);
#4623=LINE('',#40456,#5934);
#4624=LINE('',#40458,#5935);
#4625=LINE('',#40460,#5936);
#4626=LINE('',#40464,#5937);
#4627=LINE('',#40465,#5938);
#4628=LINE('',#40467,#5939);
#4629=LINE('',#40471,#5940);
#4630=LINE('',#40473,#5941);
#4631=LINE('',#40474,#5942);
#4632=LINE('',#40476,#5943);
#4633=LINE('',#40478,#5944);
#4634=LINE('',#40482,#5945);
#4635=LINE('',#40484,#5946);
#4636=LINE('',#40485,#5947);
#4637=LINE('',#40487,#5948);
#4638=LINE('',#40489,#5949);
#4639=LINE('',#40493,#5950);
#4640=LINE('',#40495,#5951);
#4641=LINE('',#40496,#5952);
#4642=LINE('',#40498,#5953);
#4643=LINE('',#40500,#5954);
#4644=LINE('',#40504,#5955);
#4645=LINE('',#40506,#5956);
#4646=LINE('',#40507,#5957);
#4647=LINE('',#40509,#5958);
#4648=LINE('',#40511,#5959);
#4649=LINE('',#40515,#5960);
#4650=LINE('',#40517,#5961);
#4651=LINE('',#40518,#5962);
#4652=LINE('',#40520,#5963);
#4653=LINE('',#40522,#5964);
#4654=LINE('',#40526,#5965);
#4655=LINE('',#40528,#5966);
#4656=LINE('',#40529,#5967);
#4657=LINE('',#40531,#5968);
#4658=LINE('',#40533,#5969);
#4659=LINE('',#40539,#5970);
#4660=LINE('',#40546,#5971);
#4661=LINE('',#40553,#5972);
#4662=LINE('',#40560,#5973);
#4663=LINE('',#40566,#5974);
#4664=LINE('',#40574,#5975);
#4665=LINE('',#40578,#5976);
#4666=LINE('',#40582,#5977);
#4667=LINE('',#40590,#5978);
#4668=LINE('',#40596,#5979);
#4669=LINE('',#40603,#5980);
#4670=LINE('',#40609,#5981);
#4671=LINE('',#40615,#5982);
#4672=LINE('',#40621,#5983);
#4673=LINE('',#40627,#5984);
#4674=LINE('',#40633,#5985);
#4675=LINE('',#40638,#5986);
#4676=LINE('',#40643,#5987);
#4677=LINE('',#40670,#5988);
#4678=LINE('',#40718,#5989);
#4679=LINE('',#40766,#5990);
#4680=LINE('',#40814,#5991);
#4681=LINE('',#40868,#5992);
#4682=LINE('',#40916,#5993);
#4683=LINE('',#40964,#5994);
#4684=LINE('',#41018,#5995);
#4685=LINE('',#41066,#5996);
#4686=LINE('',#41114,#5997);
#4687=LINE('',#41162,#5998);
#4688=LINE('',#41216,#5999);
#4689=LINE('',#41264,#6000);
#4690=LINE('',#41289,#6001);
#4691=LINE('',#41314,#6002);
#4692=LINE('',#41339,#6003);
#4693=LINE('',#41363,#6004);
#4694=LINE('',#41387,#6005);
#4695=LINE('',#41412,#6006);
#4696=LINE('',#41437,#6007);
#4697=LINE('',#41461,#6008);
#4698=LINE('',#41486,#6009);
#4699=LINE('',#41511,#6010);
#4700=LINE('',#41535,#6011);
#4701=LINE('',#42741,#6012);
#4702=LINE('',#42746,#6013);
#4703=LINE('',#42758,#6014);
#4704=LINE('',#42773,#6015);
#4705=LINE('',#42788,#6016);
#4706=LINE('',#42803,#6017);
#4707=LINE('',#42818,#6018);
#4708=LINE('',#42833,#6019);
#4709=LINE('',#42848,#6020);
#4710=LINE('',#42863,#6021);
#4711=LINE('',#42878,#6022);
#4712=LINE('',#42898,#6023);
#4713=LINE('',#42900,#6024);
#4714=LINE('',#42902,#6025);
#4715=LINE('',#42903,#6026);
#4716=LINE('',#42906,#6027);
#4717=LINE('',#42908,#6028);
#4718=LINE('',#42909,#6029);
#4719=LINE('',#42912,#6030);
#4720=LINE('',#42914,#6031);
#4721=LINE('',#42915,#6032);
#4722=LINE('',#42918,#6033);
#4723=LINE('',#42920,#6034);
#4724=LINE('',#42921,#6035);
#4725=LINE('',#42924,#6036);
#4726=LINE('',#42926,#6037);
#4727=LINE('',#42927,#6038);
#4728=LINE('',#42930,#6039);
#4729=LINE('',#42932,#6040);
#4730=LINE('',#42933,#6041);
#4731=LINE('',#42936,#6042);
#4732=LINE('',#42938,#6043);
#4733=LINE('',#42939,#6044);
#4734=LINE('',#42942,#6045);
#4735=LINE('',#42944,#6046);
#4736=LINE('',#42945,#6047);
#4737=LINE('',#42948,#6048);
#4738=LINE('',#42950,#6049);
#4739=LINE('',#42951,#6050);
#4740=LINE('',#42953,#6051);
#4741=LINE('',#42954,#6052);
#4742=LINE('',#42968,#6053);
#4743=LINE('',#42973,#6054);
#4744=LINE('',#42985,#6055);
#4745=LINE('',#43000,#6056);
#4746=LINE('',#43015,#6057);
#4747=LINE('',#43030,#6058);
#4748=LINE('',#43045,#6059);
#4749=LINE('',#43060,#6060);
#4750=LINE('',#43075,#6061);
#4751=LINE('',#43090,#6062);
#4752=LINE('',#43105,#6063);
#4753=LINE('',#43125,#6064);
#4754=LINE('',#43127,#6065);
#4755=LINE('',#43129,#6066);
#4756=LINE('',#43130,#6067);
#4757=LINE('',#43133,#6068);
#4758=LINE('',#43135,#6069);
#4759=LINE('',#43136,#6070);
#4760=LINE('',#43139,#6071);
#4761=LINE('',#43141,#6072);
#4762=LINE('',#43142,#6073);
#4763=LINE('',#43145,#6074);
#4764=LINE('',#43147,#6075);
#4765=LINE('',#43148,#6076);
#4766=LINE('',#43151,#6077);
#4767=LINE('',#43153,#6078);
#4768=LINE('',#43154,#6079);
#4769=LINE('',#43157,#6080);
#4770=LINE('',#43159,#6081);
#4771=LINE('',#43160,#6082);
#4772=LINE('',#43163,#6083);
#4773=LINE('',#43165,#6084);
#4774=LINE('',#43166,#6085);
#4775=LINE('',#43169,#6086);
#4776=LINE('',#43171,#6087);
#4777=LINE('',#43172,#6088);
#4778=LINE('',#43175,#6089);
#4779=LINE('',#43177,#6090);
#4780=LINE('',#43178,#6091);
#4781=LINE('',#43180,#6092);
#4782=LINE('',#43181,#6093);
#4783=LINE('',#43186,#6094);
#4784=LINE('',#43188,#6095);
#4785=LINE('',#43190,#6096);
#4786=LINE('',#43191,#6097);
#4787=LINE('',#43194,#6098);
#4788=LINE('',#43196,#6099);
#4789=LINE('',#43197,#6100);
#4790=LINE('',#43200,#6101);
#4791=LINE('',#43202,#6102);
#4792=LINE('',#43203,#6103);
#4793=LINE('',#43206,#6104);
#4794=LINE('',#43208,#6105);
#4795=LINE('',#43209,#6106);
#4796=LINE('',#43212,#6107);
#4797=LINE('',#43214,#6108);
#4798=LINE('',#43215,#6109);
#4799=LINE('',#43218,#6110);
#4800=LINE('',#43220,#6111);
#4801=LINE('',#43221,#6112);
#4802=LINE('',#43224,#6113);
#4803=LINE('',#43226,#6114);
#4804=LINE('',#43227,#6115);
#4805=LINE('',#43230,#6116);
#4806=LINE('',#43232,#6117);
#4807=LINE('',#43233,#6118);
#4808=LINE('',#43236,#6119);
#4809=LINE('',#43238,#6120);
#4810=LINE('',#43239,#6121);
#4811=LINE('',#43241,#6122);
#4812=LINE('',#43242,#6123);
#4813=LINE('',#43251,#6124);
#4814=LINE('',#43255,#6125);
#4815=LINE('',#43261,#6126);
#4816=LINE('',#43263,#6127);
#4817=LINE('',#43265,#6128);
#4818=LINE('',#43266,#6129);
#4819=LINE('',#43270,#6130);
#4820=LINE('',#43273,#6131);
#4821=LINE('',#43274,#6132);
#4822=LINE('',#43280,#6133);
#4823=LINE('',#43282,#6134);
#4824=LINE('',#43284,#6135);
#4825=LINE('',#43285,#6136);
#4826=LINE('',#43289,#6137);
#4827=LINE('',#43292,#6138);
#4828=LINE('',#43293,#6139);
#4829=LINE('',#43299,#6140);
#4830=LINE('',#43301,#6141);
#4831=LINE('',#43303,#6142);
#4832=LINE('',#43304,#6143);
#4833=LINE('',#43308,#6144);
#4834=LINE('',#43311,#6145);
#4835=LINE('',#43312,#6146);
#4836=LINE('',#43318,#6147);
#4837=LINE('',#43320,#6148);
#4838=LINE('',#43322,#6149);
#4839=LINE('',#43323,#6150);
#4840=LINE('',#43327,#6151);
#4841=LINE('',#43330,#6152);
#4842=LINE('',#43331,#6153);
#4843=LINE('',#43337,#6154);
#4844=LINE('',#43339,#6155);
#4845=LINE('',#43341,#6156);
#4846=LINE('',#43342,#6157);
#4847=LINE('',#43346,#6158);
#4848=LINE('',#43349,#6159);
#4849=LINE('',#43350,#6160);
#4850=LINE('',#43356,#6161);
#4851=LINE('',#43358,#6162);
#4852=LINE('',#43360,#6163);
#4853=LINE('',#43361,#6164);
#4854=LINE('',#43365,#6165);
#4855=LINE('',#43368,#6166);
#4856=LINE('',#43369,#6167);
#4857=LINE('',#43375,#6168);
#4858=LINE('',#43377,#6169);
#4859=LINE('',#43379,#6170);
#4860=LINE('',#43380,#6171);
#4861=LINE('',#43384,#6172);
#4862=LINE('',#43387,#6173);
#4863=LINE('',#43388,#6174);
#4864=LINE('',#43394,#6175);
#4865=LINE('',#43396,#6176);
#4866=LINE('',#43398,#6177);
#4867=LINE('',#43399,#6178);
#4868=LINE('',#43403,#6179);
#4869=LINE('',#43406,#6180);
#4870=LINE('',#43407,#6181);
#4871=LINE('',#43413,#6182);
#4872=LINE('',#43415,#6183);
#4873=LINE('',#43417,#6184);
#4874=LINE('',#43418,#6185);
#4875=LINE('',#43422,#6186);
#4876=LINE('',#43425,#6187);
#4877=LINE('',#43426,#6188);
#4878=LINE('',#43432,#6189);
#4879=LINE('',#43434,#6190);
#4880=LINE('',#43436,#6191);
#4881=LINE('',#43437,#6192);
#4882=LINE('',#43441,#6193);
#4883=LINE('',#43444,#6194);
#4884=LINE('',#43445,#6195);
#4885=LINE('',#43451,#6196);
#4886=LINE('',#43453,#6197);
#4887=LINE('',#43455,#6198);
#4888=LINE('',#43456,#6199);
#4889=LINE('',#43460,#6200);
#4890=LINE('',#43463,#6201);
#4891=LINE('',#43464,#6202);
#4892=LINE('',#43470,#6203);
#4893=LINE('',#43472,#6204);
#4894=LINE('',#43474,#6205);
#4895=LINE('',#43475,#6206);
#4896=LINE('',#43479,#6207);
#4897=LINE('',#43482,#6208);
#4898=LINE('',#43483,#6209);
#4899=LINE('',#43489,#6210);
#4900=LINE('',#43491,#6211);
#4901=LINE('',#43493,#6212);
#4902=LINE('',#43494,#6213);
#4903=LINE('',#43498,#6214);
#4904=LINE('',#43501,#6215);
#4905=LINE('',#43502,#6216);
#4906=LINE('',#43508,#6217);
#4907=LINE('',#43510,#6218);
#4908=LINE('',#43512,#6219);
#4909=LINE('',#43513,#6220);
#4910=LINE('',#43517,#6221);
#4911=LINE('',#43520,#6222);
#4912=LINE('',#43521,#6223);
#4913=LINE('',#43527,#6224);
#4914=LINE('',#43529,#6225);
#4915=LINE('',#43531,#6226);
#4916=LINE('',#43532,#6227);
#4917=LINE('',#43537,#6228);
#4918=LINE('',#43541,#6229);
#4919=LINE('',#43542,#6230);
#4920=LINE('',#43550,#6231);
#4921=LINE('',#43552,#6232);
#4922=LINE('',#43554,#6233);
#4923=LINE('',#43555,#6234);
#4924=LINE('',#43559,#6235);
#4925=LINE('',#43562,#6236);
#4926=LINE('',#43563,#6237);
#4927=LINE('',#43569,#6238);
#4928=LINE('',#43571,#6239);
#4929=LINE('',#43573,#6240);
#4930=LINE('',#43574,#6241);
#4931=LINE('',#43578,#6242);
#4932=LINE('',#43581,#6243);
#4933=LINE('',#43582,#6244);
#4934=LINE('',#43588,#6245);
#4935=LINE('',#43590,#6246);
#4936=LINE('',#43592,#6247);
#4937=LINE('',#43593,#6248);
#4938=LINE('',#43597,#6249);
#4939=LINE('',#43600,#6250);
#4940=LINE('',#43601,#6251);
#4941=LINE('',#43607,#6252);
#4942=LINE('',#43609,#6253);
#4943=LINE('',#43611,#6254);
#4944=LINE('',#43612,#6255);
#4945=LINE('',#43616,#6256);
#4946=LINE('',#43619,#6257);
#4947=LINE('',#43620,#6258);
#4948=LINE('',#43626,#6259);
#4949=LINE('',#43628,#6260);
#4950=LINE('',#43630,#6261);
#4951=LINE('',#43631,#6262);
#4952=LINE('',#43635,#6263);
#4953=LINE('',#43638,#6264);
#4954=LINE('',#43639,#6265);
#4955=LINE('',#43645,#6266);
#4956=LINE('',#43647,#6267);
#4957=LINE('',#43649,#6268);
#4958=LINE('',#43650,#6269);
#4959=LINE('',#43654,#6270);
#4960=LINE('',#43657,#6271);
#4961=LINE('',#43658,#6272);
#4962=LINE('',#43664,#6273);
#4963=LINE('',#43666,#6274);
#4964=LINE('',#43668,#6275);
#4965=LINE('',#43669,#6276);
#4966=LINE('',#43673,#6277);
#4967=LINE('',#43676,#6278);
#4968=LINE('',#43677,#6279);
#4969=LINE('',#43683,#6280);
#4970=LINE('',#43685,#6281);
#4971=LINE('',#43687,#6282);
#4972=LINE('',#43688,#6283);
#4973=LINE('',#43692,#6284);
#4974=LINE('',#43695,#6285);
#4975=LINE('',#43696,#6286);
#4976=LINE('',#43702,#6287);
#4977=LINE('',#43704,#6288);
#4978=LINE('',#43706,#6289);
#4979=LINE('',#43707,#6290);
#4980=LINE('',#43711,#6291);
#4981=LINE('',#43714,#6292);
#4982=LINE('',#43715,#6293);
#4983=LINE('',#43721,#6294);
#4984=LINE('',#43723,#6295);
#4985=LINE('',#43725,#6296);
#4986=LINE('',#43726,#6297);
#4987=LINE('',#43730,#6298);
#4988=LINE('',#43733,#6299);
#4989=LINE('',#43734,#6300);
#4990=LINE('',#43740,#6301);
#4991=LINE('',#43742,#6302);
#4992=LINE('',#43744,#6303);
#4993=LINE('',#43745,#6304);
#4994=LINE('',#43749,#6305);
#4995=LINE('',#43752,#6306);
#4996=LINE('',#43753,#6307);
#4997=LINE('',#43759,#6308);
#4998=LINE('',#43761,#6309);
#4999=LINE('',#43763,#6310);
#5000=LINE('',#43764,#6311);
#5001=LINE('',#43768,#6312);
#5002=LINE('',#43771,#6313);
#5003=LINE('',#43772,#6314);
#5004=LINE('',#43778,#6315);
#5005=LINE('',#43780,#6316);
#5006=LINE('',#43782,#6317);
#5007=LINE('',#43783,#6318);
#5008=LINE('',#43787,#6319);
#5009=LINE('',#43790,#6320);
#5010=LINE('',#43791,#6321);
#5011=LINE('',#43797,#6322);
#5012=LINE('',#43799,#6323);
#5013=LINE('',#43801,#6324);
#5014=LINE('',#43802,#6325);
#5015=LINE('',#43806,#6326);
#5016=LINE('',#43809,#6327);
#5017=LINE('',#43810,#6328);
#5018=LINE('',#43816,#6329);
#5019=LINE('',#43818,#6330);
#5020=LINE('',#43820,#6331);
#5021=LINE('',#43821,#6332);
#5022=LINE('',#43825,#6333);
#5023=LINE('',#43828,#6334);
#5024=LINE('',#43829,#6335);
#5025=LINE('',#43838,#6336);
#5026=LINE('',#43840,#6337);
#5027=LINE('',#43845,#6338);
#5028=LINE('',#43852,#6339);
#5029=LINE('',#43856,#6340);
#5030=LINE('',#43857,#6341);
#5031=LINE('',#43861,#6342);
#5032=LINE('',#43867,#6343);
#5033=LINE('',#43869,#6344);
#5034=LINE('',#43871,#6345);
#5035=LINE('',#43872,#6346);
#5036=LINE('',#43875,#6347);
#5037=LINE('',#43877,#6348);
#5038=LINE('',#43878,#6349);
#5039=LINE('',#43882,#6350);
#5040=LINE('',#43884,#6351);
#5041=LINE('',#43886,#6352);
#5042=LINE('',#43887,#6353);
#5043=LINE('',#43890,#6354);
#5044=LINE('',#43892,#6355);
#5045=LINE('',#43893,#6356);
#5046=LINE('',#43897,#6357);
#5047=LINE('',#43899,#6358);
#5048=LINE('',#43901,#6359);
#5049=LINE('',#43903,#6360);
#5050=LINE('',#43904,#6361);
#5051=LINE('',#43907,#6362);
#5052=LINE('',#43909,#6363);
#5053=LINE('',#43910,#6364);
#5054=LINE('',#43913,#6365);
#5055=LINE('',#43918,#6366);
#5056=LINE('',#43919,#6367);
#5057=LINE('',#43921,#6368);
#5058=LINE('',#43922,#6369);
#5059=LINE('',#43930,#6370);
#5060=LINE('',#43932,#6371);
#5061=LINE('',#43934,#6372);
#5062=LINE('',#43936,#6373);
#5063=LINE('',#43937,#6374);
#5064=LINE('',#43940,#6375);
#5065=LINE('',#43942,#6376);
#5066=LINE('',#43943,#6377);
#5067=LINE('',#43948,#6378);
#5068=LINE('',#43951,#6379);
#5069=LINE('',#43952,#6380);
#5070=LINE('',#43955,#6381);
#5071=LINE('',#43957,#6382);
#5072=LINE('',#43959,#6383);
#5073=LINE('',#43961,#6384);
#5074=LINE('',#43965,#6385);
#5075=LINE('',#43966,#6386);
#5076=LINE('',#43969,#6387);
#5077=LINE('',#43970,#6388);
#5078=LINE('',#43973,#6389);
#5079=LINE('',#43977,#6390);
#5080=LINE('',#43979,#6391);
#5081=LINE('',#43981,#6392);
#5082=LINE('',#43982,#6393);
#5083=LINE('',#43983,#6394);
#5084=LINE('',#44135,#6395);
#5085=LINE('',#44168,#6396);
#5086=LINE('',#44177,#6397);
#5087=LINE('',#44180,#6398);
#5088=LINE('',#44181,#6399);
#5089=LINE('',#44184,#6400);
#5090=LINE('',#44186,#6401);
#5091=LINE('',#44188,#6402);
#5092=LINE('',#44192,#6403);
#5093=LINE('',#44193,#6404);
#5094=LINE('',#44200,#6405);
#5095=LINE('',#44269,#6406);
#5096=LINE('',#44270,#6407);
#5097=LINE('',#44421,#6408);
#5098=LINE('',#44461,#6409);
#5099=LINE('',#44463,#6410);
#5100=LINE('',#44464,#6411);
#5101=LINE('',#44471,#6412);
#5102=LINE('',#44473,#6413);
#5103=LINE('',#44474,#6414);
#5104=LINE('',#44717,#6415);
#5105=LINE('',#44753,#6416);
#5106=LINE('',#44762,#6417);
#5107=LINE('',#44802,#6418);
#5108=LINE('',#44805,#6419);
#5109=LINE('',#44809,#6420);
#5110=LINE('',#44820,#6421);
#5111=LINE('',#44826,#6422);
#5112=LINE('',#44828,#6423);
#5113=LINE('',#44829,#6424);
#5114=LINE('',#44832,#6425);
#5115=LINE('',#44834,#6426);
#5116=LINE('',#44836,#6427);
#5117=LINE('',#44838,#6428);
#5118=LINE('',#44842,#6429);
#5119=LINE('',#44857,#6430);
#5120=LINE('',#44861,#6431);
#5121=LINE('',#44866,#6432);
#5122=LINE('',#44869,#6433);
#5123=LINE('',#44884,#6434);
#5124=LINE('',#44897,#6435);
#5125=LINE('',#44904,#6436);
#5126=LINE('',#44908,#6437);
#5127=LINE('',#44913,#6438);
#5128=LINE('',#44914,#6439);
#5129=LINE('',#44915,#6440);
#5130=LINE('',#44919,#6441);
#5131=LINE('',#44923,#6442);
#5132=LINE('',#44924,#6443);
#5133=LINE('',#44927,#6444);
#5134=LINE('',#44929,#6445);
#5135=LINE('',#44930,#6446);
#5136=LINE('',#44933,#6447);
#5137=LINE('',#44942,#6448);
#5138=LINE('',#44944,#6449);
#5139=LINE('',#44945,#6450);
#5140=LINE('',#44948,#6451);
#5141=LINE('',#44953,#6452);
#5142=LINE('',#44954,#6453);
#5143=LINE('',#44955,#6454);
#5144=LINE('',#44961,#6455);
#5145=LINE('',#44964,#6456);
#5146=LINE('',#44967,#6457);
#5147=LINE('',#44968,#6458);
#5148=LINE('',#44971,#6459);
#5149=LINE('',#44973,#6460);
#5150=LINE('',#44974,#6461);
#5151=LINE('',#44977,#6462);
#5152=LINE('',#44982,#6463);
#5153=LINE('',#44983,#6464);
#5154=LINE('',#44984,#6465);
#5155=LINE('',#44989,#6466);
#5156=LINE('',#44997,#6467);
#5157=LINE('',#44999,#6468);
#5158=LINE('',#45001,#6469);
#5159=LINE('',#45010,#6470);
#5160=LINE('',#45014,#6471);
#5161=LINE('',#45021,#6472);
#5162=LINE('',#45028,#6473);
#5163=LINE('',#45035,#6474);
#5164=LINE('',#45042,#6475);
#5165=LINE('',#45046,#6476);
#5166=LINE('',#45066,#6477);
#5167=LINE('',#45068,#6478);
#5168=LINE('',#45069,#6479);
#5169=LINE('',#45072,#6480);
#5170=LINE('',#45074,#6481);
#5171=LINE('',#45075,#6482);
#5172=LINE('',#45077,#6483);
#5173=LINE('',#45078,#6484);
#5174=LINE('',#45081,#6485);
#5175=LINE('',#45083,#6486);
#5176=LINE('',#45084,#6487);
#5177=LINE('',#45087,#6488);
#5178=LINE('',#45106,#6489);
#5179=LINE('',#45107,#6490);
#5180=LINE('',#45110,#6491);
#5181=LINE('',#45112,#6492);
#5182=LINE('',#45113,#6493);
#5183=LINE('',#45115,#6494);
#5184=LINE('',#45116,#6495);
#5185=LINE('',#45118,#6496);
#5186=LINE('',#45123,#6497);
#5187=LINE('',#45133,#6498);
#5188=LINE('',#45135,#6499);
#5189=LINE('',#45142,#6500);
#5190=LINE('',#45145,#6501);
#5191=LINE('',#45148,#6502);
#5192=LINE('',#45150,#6503);
#5193=LINE('',#45151,#6504);
#5194=LINE('',#45157,#6505);
#5195=LINE('',#45159,#6506);
#5196=LINE('',#45160,#6507);
#5197=VECTOR('',#18133,15.45);
#5198=VECTOR('',#18140,15.2);
#5199=VECTOR('',#18149,15.45);
#5200=VECTOR('',#18154,10.);
#5201=VECTOR('',#18155,10.);
#5202=VECTOR('',#18156,10.);
#5203=VECTOR('',#18159,10.);
#5204=VECTOR('',#18160,10.);
#5205=VECTOR('',#18163,10.);
#5206=VECTOR('',#18164,10.);
#5207=VECTOR('',#18165,10.);
#5208=VECTOR('',#18166,10.);
#5209=VECTOR('',#18171,10.);
#5210=VECTOR('',#18172,10.);
#5211=VECTOR('',#18175,10.);
#5212=VECTOR('',#18176,10.);
#5213=VECTOR('',#18177,10.);
#5214=VECTOR('',#18178,10.);
#5215=VECTOR('',#18179,10.);
#5216=VECTOR('',#18180,10.);
#5217=VECTOR('',#18181,10.);
#5218=VECTOR('',#18184,10.);
#5219=VECTOR('',#18187,10.);
#5220=VECTOR('',#18188,10.);
#5221=VECTOR('',#18189,10.);
#5222=VECTOR('',#18192,10.);
#5223=VECTOR('',#18199,10.);
#5224=VECTOR('',#18200,10.);
#5225=VECTOR('',#18201,10.);
#5226=VECTOR('',#18202,10.);
#5227=VECTOR('',#18203,10.);
#5228=VECTOR('',#18204,10.);
#5229=VECTOR('',#18205,10.);
#5230=VECTOR('',#18206,10.);
#5231=VECTOR('',#18209,10.);
#5232=VECTOR('',#18210,10.);
#5233=VECTOR('',#18211,10.);
#5234=VECTOR('',#18212,10.);
#5235=VECTOR('',#18213,10.);
#5236=VECTOR('',#18214,10.);
#5237=VECTOR('',#18215,10.);
#5238=VECTOR('',#18218,10.);
#5239=VECTOR('',#18221,10.);
#5240=VECTOR('',#18224,10.);
#5241=VECTOR('',#18225,10.);
#5242=VECTOR('',#18226,10.);
#5243=VECTOR('',#18229,10.);
#5244=VECTOR('',#18234,10.);
#5245=VECTOR('',#18235,10.);
#5246=VECTOR('',#18240,10.);
#5247=VECTOR('',#18243,10.);
#5248=VECTOR('',#18258,10.);
#5249=VECTOR('',#18259,10.);
#5250=VECTOR('',#18262,10.);
#5251=VECTOR('',#18263,10.);
#5252=VECTOR('',#18266,10.);
#5253=VECTOR('',#18267,10.);
#5254=VECTOR('',#18278,10.);
#5255=VECTOR('',#18281,10.);
#5256=VECTOR('',#18282,10.);
#5257=VECTOR('',#18299,10.);
#5258=VECTOR('',#18302,10.);
#5259=VECTOR('',#18321,10.);
#5260=VECTOR('',#18322,10.);
#5261=VECTOR('',#18325,10.);
#5262=VECTOR('',#18326,10.);
#5263=VECTOR('',#18343,10.);
#5264=VECTOR('',#18346,10.);
#5265=VECTOR('',#18347,10.);
#5266=VECTOR('',#18360,10.);
#5267=VECTOR('',#18373,10.);
#5268=VECTOR('',#18384,10.);
#5269=VECTOR('',#18385,10.);
#5270=VECTOR('',#18392,10.);
#5271=VECTOR('',#18393,10.);
#5272=VECTOR('',#18394,10.);
#5273=VECTOR('',#18395,10.);
#5274=VECTOR('',#18396,10.);
#5275=VECTOR('',#18397,10.);
#5276=VECTOR('',#18398,10.);
#5277=VECTOR('',#18399,10.);
#5278=VECTOR('',#18400,10.);
#5279=VECTOR('',#18401,10.);
#5280=VECTOR('',#18402,10.);
#5281=VECTOR('',#18403,10.);
#5282=VECTOR('',#18404,10.);
#5283=VECTOR('',#18405,10.);
#5284=VECTOR('',#18406,10.);
#5285=VECTOR('',#18407,10.);
#5286=VECTOR('',#18408,10.);
#5287=VECTOR('',#18409,10.);
#5288=VECTOR('',#18410,10.);
#5289=VECTOR('',#18413,10.);
#5290=VECTOR('',#18420,10.);
#5291=VECTOR('',#18425,10.);
#5292=VECTOR('',#18428,10.);
#5293=VECTOR('',#18431,10.);
#5294=VECTOR('',#18434,10.);
#5295=VECTOR('',#18439,10.);
#5296=VECTOR('',#18450,10.);
#5297=VECTOR('',#18455,10.);
#5298=VECTOR('',#18466,10.);
#5299=VECTOR('',#18469,10.);
#5300=VECTOR('',#18480,10.);
#5301=VECTOR('',#18481,10.);
#5302=VECTOR('',#18484,10.);
#5303=VECTOR('',#18485,10.);
#5304=VECTOR('',#18488,10.);
#5305=VECTOR('',#18491,10.);
#5306=VECTOR('',#18492,10.);
#5307=VECTOR('',#18509,26.5);
#5308=VECTOR('',#18528,27.);
#5309=VECTOR('',#18533,10.);
#5310=VECTOR('',#18536,10.);
#5311=VECTOR('',#18547,10.);
#5312=VECTOR('',#18550,10.);
#5313=VECTOR('',#18561,10.);
#5314=VECTOR('',#18588,10.);
#5315=VECTOR('',#18593,10.);
#5316=VECTOR('',#18598,10.);
#5317=VECTOR('',#18601,10.);
#5318=VECTOR('',#18604,10.);
#5319=VECTOR('',#18605,10.);
#5320=VECTOR('',#18606,10.);
#5321=VECTOR('',#18607,10.);
#5322=VECTOR('',#18608,10.);
#5323=VECTOR('',#18609,10.);
#5324=VECTOR('',#18610,10.);
#5325=VECTOR('',#18611,10.);
#5326=VECTOR('',#18612,10.);
#5327=VECTOR('',#18613,10.);
#5328=VECTOR('',#18614,10.);
#5329=VECTOR('',#18619,10.);
#5330=VECTOR('',#18620,10.);
#5331=VECTOR('',#18621,10.);
#5332=VECTOR('',#18624,10.);
#5333=VECTOR('',#18625,10.);
#5334=VECTOR('',#18628,10.);
#5335=VECTOR('',#18629,10.);
#5336=VECTOR('',#18632,10.);
#5337=VECTOR('',#18633,10.);
#5338=VECTOR('',#18636,10.);
#5339=VECTOR('',#18637,10.);
#5340=VECTOR('',#18640,10.);
#5341=VECTOR('',#18641,10.);
#5342=VECTOR('',#18644,10.);
#5343=VECTOR('',#18645,10.);
#5344=VECTOR('',#18648,10.);
#5345=VECTOR('',#18651,10.);
#5346=VECTOR('',#18652,10.);
#5347=VECTOR('',#18653,10.);
#5348=VECTOR('',#18654,10.);
#5349=VECTOR('',#18655,10.);
#5350=VECTOR('',#18656,10.);
#5351=VECTOR('',#18657,10.);
#5352=VECTOR('',#18658,10.);
#5353=VECTOR('',#18659,10.);
#5354=VECTOR('',#18660,10.);
#5355=VECTOR('',#18661,10.);
#5356=VECTOR('',#18662,10.);
#5357=VECTOR('',#18663,10.);
#5358=VECTOR('',#18664,10.);
#5359=VECTOR('',#18665,10.);
#5360=VECTOR('',#18666,10.);
#5361=VECTOR('',#18671,10.);
#5362=VECTOR('',#18672,10.);
#5363=VECTOR('',#18673,10.);
#5364=VECTOR('',#18676,10.);
#5365=VECTOR('',#18677,10.);
#5366=VECTOR('',#18680,10.);
#5367=VECTOR('',#18681,10.);
#5368=VECTOR('',#18684,10.);
#5369=VECTOR('',#18685,10.);
#5370=VECTOR('',#18688,10.);
#5371=VECTOR('',#18689,10.);
#5372=VECTOR('',#18692,10.);
#5373=VECTOR('',#18693,10.);
#5374=VECTOR('',#18696,10.);
#5375=VECTOR('',#18697,10.);
#5376=VECTOR('',#18700,10.);
#5377=VECTOR('',#18701,10.);
#5378=VECTOR('',#18704,10.);
#5379=VECTOR('',#18705,10.);
#5380=VECTOR('',#18708,10.);
#5381=VECTOR('',#18713,3.05);
#5382=VECTOR('',#18722,21.525);
#5383=VECTOR('',#18725,21.05);
#5384=VECTOR('',#18736,21.);
#5385=VECTOR('',#18741,21.);
#5386=VECTOR('',#18744,21.);
#5387=VECTOR('',#18747,21.);
#5388=VECTOR('',#18750,21.);
#5389=VECTOR('',#18753,21.);
#5390=VECTOR('',#18756,21.);
#5391=VECTOR('',#18759,21.);
#5392=VECTOR('',#18762,21.);
#5393=VECTOR('',#18765,21.);
#5394=VECTOR('',#18768,21.);
#5395=VECTOR('',#18771,21.);
#5396=VECTOR('',#18774,21.);
#5397=VECTOR('',#18777,21.);
#5398=VECTOR('',#18780,21.);
#5399=VECTOR('',#18783,21.);
#5400=VECTOR('',#18786,20.06595);
#5401=VECTOR('',#18791,20.06595);
#5402=VECTOR('',#18794,20.06595);
#5403=VECTOR('',#18797,20.06595);
#5404=VECTOR('',#18800,20.06595);
#5405=VECTOR('',#18803,20.06595);
#5406=VECTOR('',#18806,20.06595);
#5407=VECTOR('',#18809,20.06595);
#5408=VECTOR('',#18812,20.06595);
#5409=VECTOR('',#18815,20.06595);
#5410=VECTOR('',#18818,20.06595);
#5411=VECTOR('',#18821,20.06595);
#5412=VECTOR('',#18824,20.06595);
#5413=VECTOR('',#18827,20.06595);
#5414=VECTOR('',#18830,20.06595);
#5415=VECTOR('',#18833,16.5);
#5416=VECTOR('',#18838,16.5);
#5417=VECTOR('',#18841,16.5);
#5418=VECTOR('',#18844,16.5);
#5419=VECTOR('',#18847,16.5);
#5420=VECTOR('',#18850,16.5);
#5421=VECTOR('',#18853,16.5);
#5422=VECTOR('',#18856,16.5);
#5423=VECTOR('',#18859,16.5);
#5424=VECTOR('',#18862,16.5);
#5425=VECTOR('',#18865,16.5);
#5426=VECTOR('',#18870,15.56595);
#5427=VECTOR('',#18875,15.56595);
#5428=VECTOR('',#18878,15.56595);
#5429=VECTOR('',#18881,15.56595);
#5430=VECTOR('',#18884,15.56595);
#5431=VECTOR('',#18887,15.56595);
#5432=VECTOR('',#18890,15.56595);
#5433=VECTOR('',#18893,15.56595);
#5434=VECTOR('',#18896,15.56595);
#5435=VECTOR('',#18899,15.56595);
#5436=VECTOR('',#18904,4.25);
#5437=VECTOR('',#18915,4.);
#5438=VECTOR('',#18922,4.25);
#5439=VECTOR('',#18933,24.9267766952966);
#5440=VECTOR('',#18940,25.5);
#5441=VECTOR('',#18951,9.82322330470337);
#5442=VECTOR('',#18958,9.6);
#5443=VECTOR('',#18961,9.12677669529663);
#5444=VECTOR('',#18990,10.);
#5445=VECTOR('',#18991,10.);
#5446=VECTOR('',#18994,10.);
#5447=VECTOR('',#19003,10.);
#5448=VECTOR('',#19006,10.);
#5449=VECTOR('',#19009,0.6);
#5450=VECTOR('',#19010,10.);
#5451=VECTOR('',#19013,0.6);
#5452=VECTOR('',#19014,10.);
#5453=VECTOR('',#19019,5.25);
#5454=VECTOR('',#19028,5.05000000000001);
#5455=VECTOR('',#19033,4.20999999999999);
#5456=VECTOR('',#19038,4.01);
#5457=VECTOR('',#19043,12.6);
#5458=VECTOR('',#19048,13.);
#5459=VECTOR('',#19059,3.05);
#5460=VECTOR('',#19064,26.);
#5461=VECTOR('',#19067,10.);
#5462=VECTOR('',#19068,10.);
#5463=VECTOR('',#19075,18.);
#5464=VECTOR('',#19084,20.6);
#5465=VECTOR('',#19095,25.5);
#5466=VECTOR('',#19098,16.1);
#5467=VECTOR('',#19105,3.05);
#5468=VECTOR('',#19118,14.6);
#5469=VECTOR('',#19123,15.);
#5470=VECTOR('',#19132,17.71);
#5471=VECTOR('',#19137,17.96);
#5472=VECTOR('',#19146,15.05);
#5473=VECTOR('',#19155,17.96);
#5474=VECTOR('',#19164,15.05);
#5475=VECTOR('',#19173,17.96);
#5476=VECTOR('',#19178,17.71);
#5477=VECTOR('',#19205,15.06);
#5478=VECTOR('',#19216,17.97);
#5479=VECTOR('',#19229,2.9);
#5480=VECTOR('',#19234,3.);
#5481=VECTOR('',#19239,2.9);
#5482=VECTOR('',#19246,10.);
#5483=VECTOR('',#19247,10.);
#5484=VECTOR('',#19248,10.);
#5485=VECTOR('',#19249,10.);
#5486=VECTOR('',#19252,10.);
#5487=VECTOR('',#19253,10.);
#5488=VECTOR('',#19254,10.);
#5489=VECTOR('',#19255,10.);
#5490=VECTOR('',#19256,10.);
#5491=VECTOR('',#19259,10.);
#5492=VECTOR('',#19260,10.);
#5493=VECTOR('',#19263,10.);
#5494=VECTOR('',#19264,10.);
#5495=VECTOR('',#19265,10.);
#5496=VECTOR('',#19266,10.);
#5497=VECTOR('',#19269,10.);
#5498=VECTOR('',#19270,10.);
#5499=VECTOR('',#19271,10.);
#5500=VECTOR('',#19274,10.);
#5501=VECTOR('',#19275,10.);
#5502=VECTOR('',#19276,10.);
#5503=VECTOR('',#19277,10.);
#5504=VECTOR('',#19280,10.);
#5505=VECTOR('',#19281,10.);
#5506=VECTOR('',#19282,10.);
#5507=VECTOR('',#19283,10.);
#5508=VECTOR('',#19284,10.);
#5509=VECTOR('',#19285,10.);
#5510=VECTOR('',#19288,10.);
#5511=VECTOR('',#19289,10.);
#5512=VECTOR('',#19290,10.);
#5513=VECTOR('',#19293,10.);
#5514=VECTOR('',#19294,10.);
#5515=VECTOR('',#19295,10.);
#5516=VECTOR('',#19296,10.);
#5517=VECTOR('',#19299,10.);
#5518=VECTOR('',#19300,10.);
#5519=VECTOR('',#19301,10.);
#5520=VECTOR('',#19304,10.);
#5521=VECTOR('',#19305,10.);
#5522=VECTOR('',#19306,10.);
#5523=VECTOR('',#19307,10.);
#5524=VECTOR('',#19308,10.);
#5525=VECTOR('',#19311,10.);
#5526=VECTOR('',#19312,10.);
#5527=VECTOR('',#19313,10.);
#5528=VECTOR('',#19316,10.);
#5529=VECTOR('',#19317,10.);
#5530=VECTOR('',#19318,10.);
#5531=VECTOR('',#19321,10.);
#5532=VECTOR('',#19322,10.);
#5533=VECTOR('',#19323,10.);
#5534=VECTOR('',#19324,10.);
#5535=VECTOR('',#19325,10.);
#5536=VECTOR('',#19328,10.);
#5537=VECTOR('',#19329,10.);
#5538=VECTOR('',#19330,10.);
#5539=VECTOR('',#19331,10.);
#5540=VECTOR('',#19334,10.);
#5541=VECTOR('',#19335,10.);
#5542=VECTOR('',#19338,10.);
#5543=VECTOR('',#19339,10.);
#5544=VECTOR('',#19340,10.);
#5545=VECTOR('',#19341,10.);
#5546=VECTOR('',#19344,10.);
#5547=VECTOR('',#19345,10.);
#5548=VECTOR('',#19346,10.);
#5549=VECTOR('',#19347,10.);
#5550=VECTOR('',#19348,10.);
#5551=VECTOR('',#19351,10.);
#5552=VECTOR('',#19352,10.);
#5553=VECTOR('',#19355,10.);
#5554=VECTOR('',#19356,10.);
#5555=VECTOR('',#19359,10.);
#5556=VECTOR('',#19362,10.);
#5557=VECTOR('',#19363,10.);
#5558=VECTOR('',#19366,10.);
#5559=VECTOR('',#19369,10.);
#5560=VECTOR('',#19370,10.);
#5561=VECTOR('',#19371,10.);
#5562=VECTOR('',#19372,10.);
#5563=VECTOR('',#19373,10.);
#5564=VECTOR('',#19376,10.);
#5565=VECTOR('',#19377,10.);
#5566=VECTOR('',#19380,10.);
#5567=VECTOR('',#19381,10.);
#5568=VECTOR('',#19382,10.);
#5569=VECTOR('',#19383,10.);
#5570=VECTOR('',#19384,10.);
#5571=VECTOR('',#19385,10.);
#5572=VECTOR('',#19386,10.);
#5573=VECTOR('',#19387,10.);
#5574=VECTOR('',#19388,10.);
#5575=VECTOR('',#19389,10.);
#5576=VECTOR('',#19390,10.);
#5577=VECTOR('',#19391,10.);
#5578=VECTOR('',#19392,10.);
#5579=VECTOR('',#19393,10.);
#5580=VECTOR('',#19394,10.);
#5581=VECTOR('',#19395,10.);
#5582=VECTOR('',#19396,10.);
#5583=VECTOR('',#19397,10.);
#5584=VECTOR('',#19398,10.);
#5585=VECTOR('',#19399,10.);
#5586=VECTOR('',#19400,10.);
#5587=VECTOR('',#19401,10.);
#5588=VECTOR('',#19402,10.);
#5589=VECTOR('',#19403,10.);
#5590=VECTOR('',#19404,10.);
#5591=VECTOR('',#19405,10.);
#5592=VECTOR('',#19406,10.);
#5593=VECTOR('',#19407,10.);
#5594=VECTOR('',#19408,10.);
#5595=VECTOR('',#19409,10.);
#5596=VECTOR('',#19410,10.);
#5597=VECTOR('',#19411,10.);
#5598=VECTOR('',#19412,10.);
#5599=VECTOR('',#19415,10.);
#5600=VECTOR('',#19416,10.);
#5601=VECTOR('',#19417,10.);
#5602=VECTOR('',#19418,10.);
#5603=VECTOR('',#19421,10.);
#5604=VECTOR('',#19422,10.);
#5605=VECTOR('',#19425,10.);
#5606=VECTOR('',#19428,10.);
#5607=VECTOR('',#19429,10.);
#5608=VECTOR('',#19432,10.);
#5609=VECTOR('',#19433,10.);
#5610=VECTOR('',#19436,10.);
#5611=VECTOR('',#19439,10.);
#5612=VECTOR('',#19440,10.);
#5613=VECTOR('',#19441,10.);
#5614=VECTOR('',#19444,10.);
#5615=VECTOR('',#19445,10.);
#5616=VECTOR('',#19448,10.);
#5617=VECTOR('',#19449,10.);
#5618=VECTOR('',#19452,10.);
#5619=VECTOR('',#19453,10.);
#5620=VECTOR('',#19456,10.);
#5621=VECTOR('',#19457,10.);
#5622=VECTOR('',#19460,10.);
#5623=VECTOR('',#19461,10.);
#5624=VECTOR('',#19462,10.);
#5625=VECTOR('',#19463,10.);
#5626=VECTOR('',#19466,10.);
#5627=VECTOR('',#19467,10.);
#5628=VECTOR('',#19470,10.);
#5629=VECTOR('',#19471,10.);
#5630=VECTOR('',#19474,10.);
#5631=VECTOR('',#19475,10.);
#5632=VECTOR('',#19476,10.);
#5633=VECTOR('',#19477,10.);
#5634=VECTOR('',#19480,10.);
#5635=VECTOR('',#19481,10.);
#5636=VECTOR('',#19484,10.);
#5637=VECTOR('',#19485,10.);
#5638=VECTOR('',#19488,10.);
#5639=VECTOR('',#19489,10.);
#5640=VECTOR('',#19492,10.);
#5641=VECTOR('',#19493,10.);
#5642=VECTOR('',#19496,10.);
#5643=VECTOR('',#19501,10.);
#5644=VECTOR('',#19502,10.);
#5645=VECTOR('',#19503,10.);
#5646=VECTOR('',#19506,10.);
#5647=VECTOR('',#19507,10.);
#5648=VECTOR('',#19510,10.);
#5649=VECTOR('',#19511,10.);
#5650=VECTOR('',#19514,10.);
#5651=VECTOR('',#19515,10.);
#5652=VECTOR('',#19518,10.);
#5653=VECTOR('',#19519,10.);
#5654=VECTOR('',#19522,10.);
#5655=VECTOR('',#19523,10.);
#5656=VECTOR('',#19526,10.);
#5657=VECTOR('',#19527,10.);
#5658=VECTOR('',#19530,10.);
#5659=VECTOR('',#19533,10.);
#5660=VECTOR('',#19534,10.);
#5661=VECTOR('',#19535,10.);
#5662=VECTOR('',#19536,10.);
#5663=VECTOR('',#19537,10.);
#5664=VECTOR('',#19538,10.);
#5665=VECTOR('',#19539,10.);
#5666=VECTOR('',#19540,10.);
#5667=VECTOR('',#19541,10.);
#5668=VECTOR('',#19542,10.);
#5669=VECTOR('',#19543,10.);
#5670=VECTOR('',#19544,10.);
#5671=VECTOR('',#19547,10.);
#5672=VECTOR('',#19548,10.);
#5673=VECTOR('',#19549,10.);
#5674=VECTOR('',#19552,10.);
#5675=VECTOR('',#19553,10.);
#5676=VECTOR('',#19554,10.);
#5677=VECTOR('',#19555,10.);
#5678=VECTOR('',#19558,10.);
#5679=VECTOR('',#19559,10.);
#5680=VECTOR('',#19562,10.);
#5681=VECTOR('',#19563,10.);
#5682=VECTOR('',#19566,10.);
#5683=VECTOR('',#19567,10.);
#5684=VECTOR('',#19570,10.);
#5685=VECTOR('',#19573,10.);
#5686=VECTOR('',#19574,10.);
#5687=VECTOR('',#19575,10.);
#5688=VECTOR('',#19576,10.);
#5689=VECTOR('',#19577,10.);
#5690=VECTOR('',#19578,10.);
#5691=VECTOR('',#19579,10.);
#5692=VECTOR('',#19580,10.);
#5693=VECTOR('',#19581,10.);
#5694=VECTOR('',#19582,10.);
#5695=VECTOR('',#19583,10.);
#5696=VECTOR('',#19584,10.);
#5697=VECTOR('',#19585,10.);
#5698=VECTOR('',#19588,10.);
#5699=VECTOR('',#19589,10.);
#5700=VECTOR('',#19590,10.);
#5701=VECTOR('',#19591,10.);
#5702=VECTOR('',#19592,10.);
#5703=VECTOR('',#19593,10.);
#5704=VECTOR('',#19594,10.);
#5705=VECTOR('',#19595,10.);
#5706=VECTOR('',#19596,10.);
#5707=VECTOR('',#19597,10.);
#5708=VECTOR('',#19598,10.);
#5709=VECTOR('',#19599,10.);
#5710=VECTOR('',#19600,10.);
#5711=VECTOR('',#19603,10.);
#5712=VECTOR('',#19604,10.);
#5713=VECTOR('',#19607,10.);
#5714=VECTOR('',#19608,10.);
#5715=VECTOR('',#19611,10.);
#5716=VECTOR('',#19612,10.);
#5717=VECTOR('',#19615,10.);
#5718=VECTOR('',#19616,10.);
#5719=VECTOR('',#19619,10.);
#5720=VECTOR('',#19624,10.);
#5721=VECTOR('',#19625,10.);
#5722=VECTOR('',#19628,10.);
#5723=VECTOR('',#19633,10.);
#5724=VECTOR('',#19638,10.);
#5725=VECTOR('',#19651,2.8);
#5726=VECTOR('',#19656,3.);
#5727=VECTOR('',#19665,2.5);
#5728=VECTOR('',#19674,3.);
#5729=VECTOR('',#19683,2.5);
#5730=VECTOR('',#19692,3.);
#5731=VECTOR('',#19697,2.8);
#5732=VECTOR('',#19704,12.);
#5733=VECTOR('',#19709,12.);
#5734=VECTOR('',#19712,12.);
#5735=VECTOR('',#19715,12.);
#5736=VECTOR('',#19718,12.);
#5737=VECTOR('',#19721,12.);
#5738=VECTOR('',#19724,12.);
#5739=VECTOR('',#19727,12.);
#5740=VECTOR('',#19730,12.);
#5741=VECTOR('',#19733,12.);
#5742=VECTOR('',#19736,12.);
#5743=VECTOR('',#19739,12.);
#5744=VECTOR('',#19742,11.06595);
#5745=VECTOR('',#19747,11.06595);
#5746=VECTOR('',#19750,11.06595);
#5747=VECTOR('',#19753,11.06595);
#5748=VECTOR('',#19756,11.06595);
#5749=VECTOR('',#19759,11.06595);
#5750=VECTOR('',#19762,11.06595);
#5751=VECTOR('',#19765,11.06595);
#5752=VECTOR('',#19768,11.06595);
#5753=VECTOR('',#19771,11.06595);
#5754=VECTOR('',#19774,11.06595);
#5755=VECTOR('',#19779,14.9061737618886);
#5756=VECTOR('',#19786,19.);
#5757=VECTOR('',#19797,22.8438262381114);
#5758=VECTOR('',#19804,23.);
#5759=VECTOR('',#19823,16.55);
#5760=VECTOR('',#19832,22.6);
#5761=VECTOR('',#19837,11.6);
#5762=VECTOR('',#19844,5.05);
#5763=VECTOR('',#19853,17.5);
#5764=VECTOR('',#19862,5.);
#5765=VECTOR('',#19867,5.);
#5766=VECTOR('',#19870,5.);
#5767=VECTOR('',#19873,5.);
#5768=VECTOR('',#19876,5.);
#5769=VECTOR('',#19879,5.);
#5770=VECTOR('',#19882,5.);
#5771=VECTOR('',#19885,5.);
#5772=VECTOR('',#19888,5.);
#5773=VECTOR('',#19891,5.);
#5774=VECTOR('',#19894,5.);
#5775=VECTOR('',#19897,5.);
#5776=VECTOR('',#19900,5.);
#5777=VECTOR('',#19903,4.372);
#5778=VECTOR('',#19908,4.372);
#5779=VECTOR('',#19913,4.372);
#5780=VECTOR('',#19916,4.372);
#5781=VECTOR('',#19919,4.372);
#5782=VECTOR('',#19922,4.372);
#5783=VECTOR('',#19925,4.372);
#5784=VECTOR('',#19928,4.372);
#5785=VECTOR('',#19931,4.372);
#5786=VECTOR('',#19934,4.372);
#5787=VECTOR('',#19937,4.372);
#5788=VECTOR('',#19940,4.372);
#5789=VECTOR('',#19943,4.372);
#5790=VECTOR('',#19946,10.);
#5791=VECTOR('',#19949,10.);
#5792=VECTOR('',#19958,10.);
#5793=VECTOR('',#19961,10.);
#5794=VECTOR('',#19968,10.);
#5795=VECTOR('',#19971,10.);
#5796=VECTOR('',#19974,10.);
#5797=VECTOR('',#19977,10.);
#5798=VECTOR('',#19980,7.);
#5799=VECTOR('',#19983,10.);
#5800=VECTOR('',#19986,7.);
#5801=VECTOR('',#19991,10.);
#5802=VECTOR('',#19996,10.);
#5803=VECTOR('',#19999,10.);
#5804=VECTOR('',#20002,10.);
#5805=VECTOR('',#20005,10.);
#5806=VECTOR('',#20006,10.);
#5807=VECTOR('',#20009,10.);
#5808=VECTOR('',#20012,10.);
#5809=VECTOR('',#20015,10.);
#5810=VECTOR('',#20018,10.);
#5811=VECTOR('',#20021,10.);
#5812=VECTOR('',#20024,10.);
#5813=VECTOR('',#20027,10.);
#5814=VECTOR('',#20030,10.);
#5815=VECTOR('',#20033,10.);
#5816=VECTOR('',#20036,10.);
#5817=VECTOR('',#20039,10.);
#5818=VECTOR('',#20042,10.);
#5819=VECTOR('',#20045,10.);
#5820=VECTOR('',#20048,10.);
#5821=VECTOR('',#20051,10.);
#5822=VECTOR('',#20054,10.);
#5823=VECTOR('',#20057,10.);
#5824=VECTOR('',#20060,10.);
#5825=VECTOR('',#20063,10.);
#5826=VECTOR('',#20066,10.);
#5827=VECTOR('',#20069,10.);
#5828=VECTOR('',#20072,10.);
#5829=VECTOR('',#20075,10.);
#5830=VECTOR('',#20078,10.);
#5831=VECTOR('',#20081,10.);
#5832=VECTOR('',#20084,10.);
#5833=VECTOR('',#20087,10.);
#5834=VECTOR('',#20090,10.);
#5835=VECTOR('',#20093,10.);
#5836=VECTOR('',#20096,10.);
#5837=VECTOR('',#20099,10.);
#5838=VECTOR('',#20102,10.);
#5839=VECTOR('',#20105,10.);
#5840=VECTOR('',#20108,10.);
#5841=VECTOR('',#20111,10.);
#5842=VECTOR('',#20114,10.);
#5843=VECTOR('',#20117,10.);
#5844=VECTOR('',#20120,10.);
#5845=VECTOR('',#20123,10.);
#5846=VECTOR('',#20126,10.);
#5847=VECTOR('',#20129,10.);
#5848=VECTOR('',#20150,10.);
#5849=VECTOR('',#20153,10.);
#5850=VECTOR('',#20154,10.);
#5851=VECTOR('',#20155,10.);
#5852=VECTOR('',#20156,10.);
#5853=VECTOR('',#20157,10.);
#5854=VECTOR('',#20162,10.);
#5855=VECTOR('',#20163,10.);
#5856=VECTOR('',#20166,10.);
#5857=VECTOR('',#20167,10.);
#5858=VECTOR('',#20168,10.);
#5859=VECTOR('',#20171,10.);
#5860=VECTOR('',#20174,10.);
#5861=VECTOR('',#20179,10.);
#5862=VECTOR('',#20180,10.);
#5863=VECTOR('',#20181,10.);
#5864=VECTOR('',#20184,10.);
#5865=VECTOR('',#20187,10.);
#5866=VECTOR('',#20192,10.);
#5867=VECTOR('',#20193,10.);
#5868=VECTOR('',#20194,10.);
#5869=VECTOR('',#20197,10.);
#5870=VECTOR('',#20200,10.);
#5871=VECTOR('',#20205,10.);
#5872=VECTOR('',#20206,10.);
#5873=VECTOR('',#20207,10.);
#5874=VECTOR('',#20210,10.);
#5875=VECTOR('',#20213,10.);
#5876=VECTOR('',#20218,10.);
#5877=VECTOR('',#20219,10.);
#5878=VECTOR('',#20220,10.);
#5879=VECTOR('',#20223,10.);
#5880=VECTOR('',#20226,10.);
#5881=VECTOR('',#20231,10.);
#5882=VECTOR('',#20236,10.);
#5883=VECTOR('',#20237,10.);
#5884=VECTOR('',#20238,10.);
#5885=VECTOR('',#20241,10.);
#5886=VECTOR('',#20244,10.);
#5887=VECTOR('',#20249,10.);
#5888=VECTOR('',#20250,10.);
#5889=VECTOR('',#20251,10.);
#5890=VECTOR('',#20254,10.);
#5891=VECTOR('',#20257,10.);
#5892=VECTOR('',#20262,10.);
#5893=VECTOR('',#20263,10.);
#5894=VECTOR('',#20264,10.);
#5895=VECTOR('',#20267,10.);
#5896=VECTOR('',#20270,10.);
#5897=VECTOR('',#20275,10.);
#5898=VECTOR('',#20276,10.);
#5899=VECTOR('',#20277,10.);
#5900=VECTOR('',#20280,10.);
#5901=VECTOR('',#20283,10.);
#5902=VECTOR('',#20288,10.);
#5903=VECTOR('',#20289,10.);
#5904=VECTOR('',#20290,10.);
#5905=VECTOR('',#20293,10.);
#5906=VECTOR('',#20296,10.);
#5907=VECTOR('',#20301,10.);
#5908=VECTOR('',#20302,10.);
#5909=VECTOR('',#20303,10.);
#5910=VECTOR('',#20306,10.);
#5911=VECTOR('',#20309,10.);
#5912=VECTOR('',#20314,10.);
#5913=VECTOR('',#20315,10.);
#5914=VECTOR('',#20316,10.);
#5915=VECTOR('',#20319,10.);
#5916=VECTOR('',#20322,10.);
#5917=VECTOR('',#20327,10.);
#5918=VECTOR('',#20328,10.);
#5919=VECTOR('',#20329,10.);
#5920=VECTOR('',#20332,10.);
#5921=VECTOR('',#20335,10.);
#5922=VECTOR('',#20340,10.);
#5923=VECTOR('',#20341,10.);
#5924=VECTOR('',#20342,10.);
#5925=VECTOR('',#20345,10.);
#5926=VECTOR('',#20348,10.);
#5927=VECTOR('',#20353,10.);
#5928=VECTOR('',#20354,10.);
#5929=VECTOR('',#20355,10.);
#5930=VECTOR('',#20358,10.);
#5931=VECTOR('',#20361,10.);
#5932=VECTOR('',#20366,10.);
#5933=VECTOR('',#20367,10.);
#5934=VECTOR('',#20368,10.);
#5935=VECTOR('',#20371,10.);
#5936=VECTOR('',#20374,10.);
#5937=VECTOR('',#20379,10.);
#5938=VECTOR('',#20380,10.);
#5939=VECTOR('',#20383,10.);
#5940=VECTOR('',#20388,10.);
#5941=VECTOR('',#20389,10.);
#5942=VECTOR('',#20390,10.);
#5943=VECTOR('',#20393,10.);
#5944=VECTOR('',#20396,10.);
#5945=VECTOR('',#20401,10.);
#5946=VECTOR('',#20402,10.);
#5947=VECTOR('',#20403,10.);
#5948=VECTOR('',#20406,10.);
#5949=VECTOR('',#20409,10.);
#5950=VECTOR('',#20414,10.);
#5951=VECTOR('',#20415,10.);
#5952=VECTOR('',#20416,10.);
#5953=VECTOR('',#20419,10.);
#5954=VECTOR('',#20422,10.);
#5955=VECTOR('',#20427,10.);
#5956=VECTOR('',#20428,10.);
#5957=VECTOR('',#20429,10.);
#5958=VECTOR('',#20432,10.);
#5959=VECTOR('',#20435,10.);
#5960=VECTOR('',#20440,10.);
#5961=VECTOR('',#20441,10.);
#5962=VECTOR('',#20442,10.);
#5963=VECTOR('',#20445,10.);
#5964=VECTOR('',#20448,10.);
#5965=VECTOR('',#20453,10.);
#5966=VECTOR('',#20454,10.);
#5967=VECTOR('',#20455,10.);
#5968=VECTOR('',#20458,10.);
#5969=VECTOR('',#20461,10.);
#5970=VECTOR('',#20470,4.8);
#5971=VECTOR('',#20481,6.8);
#5972=VECTOR('',#20490,9.75);
#5973=VECTOR('',#20499,9.5);
#5974=VECTOR('',#20506,12.05);
#5975=VECTOR('',#20517,12.8);
#5976=VECTOR('',#20522,13.);
#5977=VECTOR('',#20527,11.5);
#5978=VECTOR('',#20538,7.98717082451265);
#5979=VECTOR('',#20545,10.25);
#5980=VECTOR('',#20554,12.4081387239171);
#5981=VECTOR('',#20561,13.75);
#5982=VECTOR('',#20568,14.8546904515702);
#5983=VECTOR('',#20575,15.);
#5984=VECTOR('',#20582,13.);
#5985=VECTOR('',#20591,14.65);
#5986=VECTOR('',#20598,11.5);
#5987=VECTOR('',#20603,5.);
#5988=VECTOR('',#20608,5.);
#5989=VECTOR('',#20611,5.);
#5990=VECTOR('',#20614,5.);
#5991=VECTOR('',#20617,5.);
#5992=VECTOR('',#20620,5.);
#5993=VECTOR('',#20623,5.);
#5994=VECTOR('',#20626,5.);
#5995=VECTOR('',#20629,5.);
#5996=VECTOR('',#20632,5.);
#5997=VECTOR('',#20635,5.);
#5998=VECTOR('',#20638,5.);
#5999=VECTOR('',#20641,5.);
#6000=VECTOR('',#20644,4.372);
#6001=VECTOR('',#20649,4.372);
#6002=VECTOR('',#20652,4.372);
#6003=VECTOR('',#20655,4.372);
#6004=VECTOR('',#20658,4.372);
#6005=VECTOR('',#20661,4.372);
#6006=VECTOR('',#20664,4.372);
#6007=VECTOR('',#20667,4.372);
#6008=VECTOR('',#20670,4.372);
#6009=VECTOR('',#20673,4.372);
#6010=VECTOR('',#20676,4.372);
#6011=VECTOR('',#20679,4.372);
#6012=VECTOR('',#20696,10.);
#6013=VECTOR('',#20697,10.);
#6014=VECTOR('',#20698,10.);
#6015=VECTOR('',#20699,10.);
#6016=VECTOR('',#20700,10.);
#6017=VECTOR('',#20701,10.);
#6018=VECTOR('',#20702,10.);
#6019=VECTOR('',#20703,10.);
#6020=VECTOR('',#20704,10.);
#6021=VECTOR('',#20705,10.);
#6022=VECTOR('',#20706,10.);
#6023=VECTOR('',#20711,10.);
#6024=VECTOR('',#20712,10.);
#6025=VECTOR('',#20713,10.);
#6026=VECTOR('',#20714,10.);
#6027=VECTOR('',#20717,10.);
#6028=VECTOR('',#20718,10.);
#6029=VECTOR('',#20719,10.);
#6030=VECTOR('',#20722,10.);
#6031=VECTOR('',#20723,10.);
#6032=VECTOR('',#20724,10.);
#6033=VECTOR('',#20727,10.);
#6034=VECTOR('',#20728,10.);
#6035=VECTOR('',#20729,10.);
#6036=VECTOR('',#20732,10.);
#6037=VECTOR('',#20733,10.);
#6038=VECTOR('',#20734,10.);
#6039=VECTOR('',#20737,10.);
#6040=VECTOR('',#20738,10.);
#6041=VECTOR('',#20739,10.);
#6042=VECTOR('',#20742,10.);
#6043=VECTOR('',#20743,10.);
#6044=VECTOR('',#20744,10.);
#6045=VECTOR('',#20747,10.);
#6046=VECTOR('',#20748,10.);
#6047=VECTOR('',#20749,10.);
#6048=VECTOR('',#20752,10.);
#6049=VECTOR('',#20753,10.);
#6050=VECTOR('',#20754,10.);
#6051=VECTOR('',#20757,10.);
#6052=VECTOR('',#20758,10.);
#6053=VECTOR('',#20761,10.);
#6054=VECTOR('',#20762,10.);
#6055=VECTOR('',#20763,10.);
#6056=VECTOR('',#20764,10.);
#6057=VECTOR('',#20765,10.);
#6058=VECTOR('',#20766,10.);
#6059=VECTOR('',#20767,10.);
#6060=VECTOR('',#20768,10.);
#6061=VECTOR('',#20769,10.);
#6062=VECTOR('',#20770,10.);
#6063=VECTOR('',#20771,10.);
#6064=VECTOR('',#20776,10.);
#6065=VECTOR('',#20777,10.);
#6066=VECTOR('',#20778,10.);
#6067=VECTOR('',#20779,10.);
#6068=VECTOR('',#20782,10.);
#6069=VECTOR('',#20783,10.);
#6070=VECTOR('',#20784,10.);
#6071=VECTOR('',#20787,10.);
#6072=VECTOR('',#20788,10.);
#6073=VECTOR('',#20789,10.);
#6074=VECTOR('',#20792,10.);
#6075=VECTOR('',#20793,10.);
#6076=VECTOR('',#20794,10.);
#6077=VECTOR('',#20797,10.);
#6078=VECTOR('',#20798,10.);
#6079=VECTOR('',#20799,10.);
#6080=VECTOR('',#20802,10.);
#6081=VECTOR('',#20803,10.);
#6082=VECTOR('',#20804,10.);
#6083=VECTOR('',#20807,10.);
#6084=VECTOR('',#20808,10.);
#6085=VECTOR('',#20809,10.);
#6086=VECTOR('',#20812,10.);
#6087=VECTOR('',#20813,10.);
#6088=VECTOR('',#20814,10.);
#6089=VECTOR('',#20817,10.);
#6090=VECTOR('',#20818,10.);
#6091=VECTOR('',#20819,10.);
#6092=VECTOR('',#20822,10.);
#6093=VECTOR('',#20823,10.);
#6094=VECTOR('',#20828,10.);
#6095=VECTOR('',#20829,10.);
#6096=VECTOR('',#20830,10.);
#6097=VECTOR('',#20831,10.);
#6098=VECTOR('',#20834,10.);
#6099=VECTOR('',#20835,10.);
#6100=VECTOR('',#20836,10.);
#6101=VECTOR('',#20839,10.);
#6102=VECTOR('',#20840,10.);
#6103=VECTOR('',#20841,10.);
#6104=VECTOR('',#20844,10.);
#6105=VECTOR('',#20845,10.);
#6106=VECTOR('',#20846,10.);
#6107=VECTOR('',#20849,10.);
#6108=VECTOR('',#20850,10.);
#6109=VECTOR('',#20851,10.);
#6110=VECTOR('',#20854,10.);
#6111=VECTOR('',#20855,10.);
#6112=VECTOR('',#20856,10.);
#6113=VECTOR('',#20859,10.);
#6114=VECTOR('',#20860,10.);
#6115=VECTOR('',#20861,10.);
#6116=VECTOR('',#20864,10.);
#6117=VECTOR('',#20865,10.);
#6118=VECTOR('',#20866,10.);
#6119=VECTOR('',#20869,10.);
#6120=VECTOR('',#20870,10.);
#6121=VECTOR('',#20871,10.);
#6122=VECTOR('',#20874,10.);
#6123=VECTOR('',#20875,10.);
#6124=VECTOR('',#20886,3.6);
#6125=VECTOR('',#20891,3.);
#6126=VECTOR('',#20898,10.);
#6127=VECTOR('',#20899,10.);
#6128=VECTOR('',#20900,10.);
#6129=VECTOR('',#20901,10.);
#6130=VECTOR('',#20906,10.);
#6131=VECTOR('',#20909,10.);
#6132=VECTOR('',#20910,10.);
#6133=VECTOR('',#20917,10.);
#6134=VECTOR('',#20918,10.);
#6135=VECTOR('',#20919,10.);
#6136=VECTOR('',#20920,10.);
#6137=VECTOR('',#20925,10.);
#6138=VECTOR('',#20928,10.);
#6139=VECTOR('',#20929,10.);
#6140=VECTOR('',#20936,10.);
#6141=VECTOR('',#20937,10.);
#6142=VECTOR('',#20938,10.);
#6143=VECTOR('',#20939,10.);
#6144=VECTOR('',#20944,10.);
#6145=VECTOR('',#20947,10.);
#6146=VECTOR('',#20948,10.);
#6147=VECTOR('',#20955,10.);
#6148=VECTOR('',#20956,10.);
#6149=VECTOR('',#20957,10.);
#6150=VECTOR('',#20958,10.);
#6151=VECTOR('',#20963,10.);
#6152=VECTOR('',#20966,10.);
#6153=VECTOR('',#20967,10.);
#6154=VECTOR('',#20974,10.);
#6155=VECTOR('',#20975,10.);
#6156=VECTOR('',#20976,10.);
#6157=VECTOR('',#20977,10.);
#6158=VECTOR('',#20982,10.);
#6159=VECTOR('',#20985,10.);
#6160=VECTOR('',#20986,10.);
#6161=VECTOR('',#20993,10.);
#6162=VECTOR('',#20994,10.);
#6163=VECTOR('',#20995,10.);
#6164=VECTOR('',#20996,10.);
#6165=VECTOR('',#21001,10.);
#6166=VECTOR('',#21004,10.);
#6167=VECTOR('',#21005,10.);
#6168=VECTOR('',#21012,10.);
#6169=VECTOR('',#21013,10.);
#6170=VECTOR('',#21014,10.);
#6171=VECTOR('',#21015,10.);
#6172=VECTOR('',#21020,10.);
#6173=VECTOR('',#21023,10.);
#6174=VECTOR('',#21024,10.);
#6175=VECTOR('',#21031,10.);
#6176=VECTOR('',#21032,10.);
#6177=VECTOR('',#21033,10.);
#6178=VECTOR('',#21034,10.);
#6179=VECTOR('',#21039,10.);
#6180=VECTOR('',#21042,10.);
#6181=VECTOR('',#21043,10.);
#6182=VECTOR('',#21050,10.);
#6183=VECTOR('',#21051,10.);
#6184=VECTOR('',#21052,10.);
#6185=VECTOR('',#21053,10.);
#6186=VECTOR('',#21058,10.);
#6187=VECTOR('',#21061,10.);
#6188=VECTOR('',#21062,10.);
#6189=VECTOR('',#21069,10.);
#6190=VECTOR('',#21070,10.);
#6191=VECTOR('',#21071,10.);
#6192=VECTOR('',#21072,10.);
#6193=VECTOR('',#21077,10.);
#6194=VECTOR('',#21080,10.);
#6195=VECTOR('',#21081,10.);
#6196=VECTOR('',#21088,10.);
#6197=VECTOR('',#21089,10.);
#6198=VECTOR('',#21090,10.);
#6199=VECTOR('',#21091,10.);
#6200=VECTOR('',#21096,10.);
#6201=VECTOR('',#21099,10.);
#6202=VECTOR('',#21100,10.);
#6203=VECTOR('',#21107,10.);
#6204=VECTOR('',#21108,10.);
#6205=VECTOR('',#21109,10.);
#6206=VECTOR('',#21110,10.);
#6207=VECTOR('',#21115,10.);
#6208=VECTOR('',#21118,10.);
#6209=VECTOR('',#21119,10.);
#6210=VECTOR('',#21126,10.);
#6211=VECTOR('',#21127,10.);
#6212=VECTOR('',#21128,10.);
#6213=VECTOR('',#21129,10.);
#6214=VECTOR('',#21134,10.);
#6215=VECTOR('',#21137,10.);
#6216=VECTOR('',#21138,10.);
#6217=VECTOR('',#21145,10.);
#6218=VECTOR('',#21146,10.);
#6219=VECTOR('',#21147,10.);
#6220=VECTOR('',#21148,10.);
#6221=VECTOR('',#21153,10.);
#6222=VECTOR('',#21156,10.);
#6223=VECTOR('',#21157,10.);
#6224=VECTOR('',#21164,10.);
#6225=VECTOR('',#21165,10.);
#6226=VECTOR('',#21166,10.);
#6227=VECTOR('',#21167,10.);
#6228=VECTOR('',#21172,10.);
#6229=VECTOR('',#21177,10.);
#6230=VECTOR('',#21178,10.);
#6231=VECTOR('',#21187,10.);
#6232=VECTOR('',#21188,10.);
#6233=VECTOR('',#21189,10.);
#6234=VECTOR('',#21190,10.);
#6235=VECTOR('',#21195,10.);
#6236=VECTOR('',#21198,10.);
#6237=VECTOR('',#21199,10.);
#6238=VECTOR('',#21206,10.);
#6239=VECTOR('',#21207,10.);
#6240=VECTOR('',#21208,10.);
#6241=VECTOR('',#21209,10.);
#6242=VECTOR('',#21214,10.);
#6243=VECTOR('',#21217,10.);
#6244=VECTOR('',#21218,10.);
#6245=VECTOR('',#21225,10.);
#6246=VECTOR('',#21226,10.);
#6247=VECTOR('',#21227,10.);
#6248=VECTOR('',#21228,10.);
#6249=VECTOR('',#21233,10.);
#6250=VECTOR('',#21236,10.);
#6251=VECTOR('',#21237,10.);
#6252=VECTOR('',#21244,10.);
#6253=VECTOR('',#21245,10.);
#6254=VECTOR('',#21246,10.);
#6255=VECTOR('',#21247,10.);
#6256=VECTOR('',#21252,10.);
#6257=VECTOR('',#21255,10.);
#6258=VECTOR('',#21256,10.);
#6259=VECTOR('',#21263,10.);
#6260=VECTOR('',#21264,10.);
#6261=VECTOR('',#21265,10.);
#6262=VECTOR('',#21266,10.);
#6263=VECTOR('',#21271,10.);
#6264=VECTOR('',#21274,10.);
#6265=VECTOR('',#21275,10.);
#6266=VECTOR('',#21282,10.);
#6267=VECTOR('',#21283,10.);
#6268=VECTOR('',#21284,10.);
#6269=VECTOR('',#21285,10.);
#6270=VECTOR('',#21290,10.);
#6271=VECTOR('',#21293,10.);
#6272=VECTOR('',#21294,10.);
#6273=VECTOR('',#21301,10.);
#6274=VECTOR('',#21302,10.);
#6275=VECTOR('',#21303,10.);
#6276=VECTOR('',#21304,10.);
#6277=VECTOR('',#21309,10.);
#6278=VECTOR('',#21312,10.);
#6279=VECTOR('',#21313,10.);
#6280=VECTOR('',#21320,10.);
#6281=VECTOR('',#21321,10.);
#6282=VECTOR('',#21322,10.);
#6283=VECTOR('',#21323,10.);
#6284=VECTOR('',#21328,10.);
#6285=VECTOR('',#21331,10.);
#6286=VECTOR('',#21332,10.);
#6287=VECTOR('',#21339,10.);
#6288=VECTOR('',#21340,10.);
#6289=VECTOR('',#21341,10.);
#6290=VECTOR('',#21342,10.);
#6291=VECTOR('',#21347,10.);
#6292=VECTOR('',#21350,10.);
#6293=VECTOR('',#21351,10.);
#6294=VECTOR('',#21358,10.);
#6295=VECTOR('',#21359,10.);
#6296=VECTOR('',#21360,10.);
#6297=VECTOR('',#21361,10.);
#6298=VECTOR('',#21366,10.);
#6299=VECTOR('',#21369,10.);
#6300=VECTOR('',#21370,10.);
#6301=VECTOR('',#21377,10.);
#6302=VECTOR('',#21378,10.);
#6303=VECTOR('',#21379,10.);
#6304=VECTOR('',#21380,10.);
#6305=VECTOR('',#21385,10.);
#6306=VECTOR('',#21388,10.);
#6307=VECTOR('',#21389,10.);
#6308=VECTOR('',#21396,10.);
#6309=VECTOR('',#21397,10.);
#6310=VECTOR('',#21398,10.);
#6311=VECTOR('',#21399,10.);
#6312=VECTOR('',#21404,10.);
#6313=VECTOR('',#21407,10.);
#6314=VECTOR('',#21408,10.);
#6315=VECTOR('',#21415,10.);
#6316=VECTOR('',#21416,10.);
#6317=VECTOR('',#21417,10.);
#6318=VECTOR('',#21418,10.);
#6319=VECTOR('',#21423,10.);
#6320=VECTOR('',#21426,10.);
#6321=VECTOR('',#21427,10.);
#6322=VECTOR('',#21434,10.);
#6323=VECTOR('',#21435,10.);
#6324=VECTOR('',#21436,10.);
#6325=VECTOR('',#21437,10.);
#6326=VECTOR('',#21442,10.);
#6327=VECTOR('',#21445,10.);
#6328=VECTOR('',#21446,10.);
#6329=VECTOR('',#21453,10.);
#6330=VECTOR('',#21454,10.);
#6331=VECTOR('',#21455,10.);
#6332=VECTOR('',#21456,10.);
#6333=VECTOR('',#21461,10.);
#6334=VECTOR('',#21464,10.);
#6335=VECTOR('',#21465,10.);
#6336=VECTOR('',#21478,3.);
#6337=VECTOR('',#21481,4.75);
#6338=VECTOR('',#21488,4.);
#6339=VECTOR('',#21497,12.7);
#6340=VECTOR('',#21502,13.);
#6341=VECTOR('',#21503,13.);
#6342=VECTOR('',#21508,12.7);
#6343=VECTOR('',#21515,10.);
#6344=VECTOR('',#21516,10.);
#6345=VECTOR('',#21517,10.);
#6346=VECTOR('',#21518,10.);
#6347=VECTOR('',#21521,10.);
#6348=VECTOR('',#21522,10.);
#6349=VECTOR('',#21523,10.);
#6350=VECTOR('',#21526,10.);
#6351=VECTOR('',#21527,10.);
#6352=VECTOR('',#21528,10.);
#6353=VECTOR('',#21529,10.);
#6354=VECTOR('',#21532,10.);
#6355=VECTOR('',#21533,10.);
#6356=VECTOR('',#21534,10.);
#6357=VECTOR('',#21537,10.);
#6358=VECTOR('',#21538,10.);
#6359=VECTOR('',#21539,10.);
#6360=VECTOR('',#21540,10.);
#6361=VECTOR('',#21541,10.);
#6362=VECTOR('',#21544,10.);
#6363=VECTOR('',#21545,10.);
#6364=VECTOR('',#21546,10.);
#6365=VECTOR('',#21549,10.);
#6366=VECTOR('',#21556,10.);
#6367=VECTOR('',#21557,10.);
#6368=VECTOR('',#21560,10.);
#6369=VECTOR('',#21561,10.);
#6370=VECTOR('',#21568,10.);
#6371=VECTOR('',#21569,10.);
#6372=VECTOR('',#21570,10.);
#6373=VECTOR('',#21571,10.);
#6374=VECTOR('',#21572,10.);
#6375=VECTOR('',#21575,10.);
#6376=VECTOR('',#21576,10.);
#6377=VECTOR('',#21577,10.);
#6378=VECTOR('',#21582,10.);
#6379=VECTOR('',#21587,10.);
#6380=VECTOR('',#21588,10.);
#6381=VECTOR('',#21591,10.);
#6382=VECTOR('',#21592,10.);
#6383=VECTOR('',#21593,10.);
#6384=VECTOR('',#21594,10.);
#6385=VECTOR('',#21599,10.);
#6386=VECTOR('',#21600,10.);
#6387=VECTOR('',#21603,10.);
#6388=VECTOR('',#21604,10.);
#6389=VECTOR('',#21607,10.);
#6390=VECTOR('',#21612,10.);
#6391=VECTOR('',#21613,10.);
#6392=VECTOR('',#21614,10.);
#6393=VECTOR('',#21615,10.);
#6394=VECTOR('',#21616,10.);
#6395=VECTOR('',#21619,10.);
#6396=VECTOR('',#21620,10.);
#6397=VECTOR('',#21623,10.);
#6398=VECTOR('',#21626,10.);
#6399=VECTOR('',#21627,10.);
#6400=VECTOR('',#21630,10.);
#6401=VECTOR('',#21631,10.);
#6402=VECTOR('',#21632,10.);
#6403=VECTOR('',#21635,10.);
#6404=VECTOR('',#21636,10.);
#6405=VECTOR('',#21643,10.);
#6406=VECTOR('',#21650,10.);
#6407=VECTOR('',#21651,10.);
#6408=VECTOR('',#21652,10.);
#6409=VECTOR('',#21657,10.);
#6410=VECTOR('',#21660,10.);
#6411=VECTOR('',#21661,10.);
#6412=VECTOR('',#21668,10.);
#6413=VECTOR('',#21669,10.);
#6414=VECTOR('',#21670,10.);
#6415=VECTOR('',#21671,10.);
#6416=VECTOR('',#21672,10.);
#6417=VECTOR('',#21675,10.);
#6418=VECTOR('',#21682,10.);
#6419=VECTOR('',#21687,10.);
#6420=VECTOR('',#21692,10.);
#6421=VECTOR('',#21707,10.);
#6422=VECTOR('',#21716,10.);
#6423=VECTOR('',#21719,10.);
#6424=VECTOR('',#21720,10.);
#6425=VECTOR('',#21725,3.05);
#6426=VECTOR('',#21728,3.05);
#6427=VECTOR('',#21731,3.05);
#6428=VECTOR('',#21734,3.05);
#6429=VECTOR('',#21739,8.);
#6430=VECTOR('',#21762,10.8232233047034);
#6431=VECTOR('',#21767,10.5);
#6432=VECTOR('',#21774,11.);
#6433=VECTOR('',#21777,9.92677669529664);
#6434=VECTOR('',#21796,11.);
#6435=VECTOR('',#21815,8.);
#6436=VECTOR('',#21824,10.);
#6437=VECTOR('',#21827,10.);
#6438=VECTOR('',#21832,10.);
#6439=VECTOR('',#21833,10.);
#6440=VECTOR('',#21834,10.);
#6441=VECTOR('',#21837,10.);
#6442=VECTOR('',#21844,10.);
#6443=VECTOR('',#21845,10.);
#6444=VECTOR('',#21848,10.);
#6445=VECTOR('',#21849,10.);
#6446=VECTOR('',#21850,10.);
#6447=VECTOR('',#21853,10.);
#6448=VECTOR('',#21864,10.);
#6449=VECTOR('',#21865,10.);
#6450=VECTOR('',#21866,10.);
#6451=VECTOR('',#21869,10.);
#6452=VECTOR('',#21874,10.);
#6453=VECTOR('',#21875,10.);
#6454=VECTOR('',#21876,10.);
#6455=VECTOR('',#21885,10.);
#6456=VECTOR('',#21888,10.);
#6457=VECTOR('',#21891,10.);
#6458=VECTOR('',#21892,10.);
#6459=VECTOR('',#21895,10.);
#6460=VECTOR('',#21896,10.);
#6461=VECTOR('',#21897,10.);
#6462=VECTOR('',#21900,10.);
#6463=VECTOR('',#21905,10.);
#6464=VECTOR('',#21906,10.);
#6465=VECTOR('',#21907,10.);
#6466=VECTOR('',#21916,10.);
#6467=VECTOR('',#21927,3.05);
#6468=VECTOR('',#21930,3.05);
#6469=VECTOR('',#21933,10.);
#6470=VECTOR('',#21946,2.8);
#6471=VECTOR('',#21951,3.);
#6472=VECTOR('',#21960,2.5);
#6473=VECTOR('',#21969,3.);
#6474=VECTOR('',#21978,2.5);
#6475=VECTOR('',#21987,3.);
#6476=VECTOR('',#21992,2.8);
#6477=VECTOR('',#22005,10.);
#6478=VECTOR('',#22006,10.);
#6479=VECTOR('',#22007,10.);
#6480=VECTOR('',#22010,10.);
#6481=VECTOR('',#22011,10.);
#6482=VECTOR('',#22012,10.);
#6483=VECTOR('',#22015,10.);
#6484=VECTOR('',#22016,10.);
#6485=VECTOR('',#22019,10.);
#6486=VECTOR('',#22020,10.);
#6487=VECTOR('',#22021,10.);
#6488=VECTOR('',#22024,10.);
#6489=VECTOR('',#22037,10.);
#6490=VECTOR('',#22038,10.);
#6491=VECTOR('',#22041,10.);
#6492=VECTOR('',#22042,10.);
#6493=VECTOR('',#22043,10.);
#6494=VECTOR('',#22046,10.);
#6495=VECTOR('',#22047,10.);
#6496=VECTOR('',#22050,10.);
#6497=VECTOR('',#22057,3.05);
#6498=VECTOR('',#22070,3.74);
#6499=VECTOR('',#22073,3.99);
#6500=VECTOR('',#22080,10.);
#6501=VECTOR('',#22083,10.);
#6502=VECTOR('',#22086,10.);
#6503=VECTOR('',#22087,10.);
#6504=VECTOR('',#22088,10.);
#6505=VECTOR('',#22095,10.);
#6506=VECTOR('',#22098,10.);
#6507=VECTOR('',#22099,10.);
#6508=CIRCLE('',#16761,15.2);
#6509=CIRCLE('',#16762,15.2);
#6510=CIRCLE('',#16763,15.7);
#6511=CIRCLE('',#16765,15.2);
#6512=CIRCLE('',#16767,21.05);
#6513=CIRCLE('',#16769,15.7);
#6514=CIRCLE('',#16771,25.5);
#6515=CIRCLE('',#16772,25.5);
#6516=CIRCLE('',#16773,25.5);
#6517=CIRCLE('',#16777,4.5);
#6518=CIRCLE('',#16778,4.5);
#6519=CIRCLE('',#16780,1.5);
#6520=CIRCLE('',#16785,1.5);
#6521=CIRCLE('',#16788,1.5);
#6522=CIRCLE('',#16791,1.5);
#6523=CIRCLE('',#16792,1.5);
#6524=CIRCLE('',#16794,1.5);
#6525=CIRCLE('',#16795,1.5);
#6526=CIRCLE('',#16797,1.5);
#6527=CIRCLE('',#16798,1.5);
#6528=CIRCLE('',#16803,1.5);
#6529=CIRCLE('',#16804,1.5);
#6530=CIRCLE('',#16805,1.5);
#6531=CIRCLE('',#16809,1.5);
#6532=CIRCLE('',#16810,1.5);
#6533=CIRCLE('',#16811,1.5);
#6534=CIRCLE('',#16813,1.49999999999999);
#6535=CIRCLE('',#16814,1.5);
#6536=CIRCLE('',#16818,1.50000000000001);
#6537=CIRCLE('',#16819,1.5);
#6538=CIRCLE('',#16820,1.5);
#6539=CIRCLE('',#16822,1.49999999999999);
#6540=CIRCLE('',#16823,1.5);
#6541=CIRCLE('',#16824,1.5);
#6542=CIRCLE('',#16828,1.5);
#6543=CIRCLE('',#16829,1.5);
#6544=CIRCLE('',#16831,1.5);
#6545=CIRCLE('',#16832,1.5);
#6546=CIRCLE('',#16833,1.5);
#6547=CIRCLE('',#16837,1.5);
#6548=CIRCLE('',#16838,1.5);
#6549=CIRCLE('',#16839,1.5);
#6550=CIRCLE('',#16841,1.5);
#6551=CIRCLE('',#16843,1.5);
#6552=CIRCLE('',#16844,1.5);
#6553=CIRCLE('',#16846,1.5);
#6554=CIRCLE('',#16849,1.5);
#6555=CIRCLE('',#16850,1.5);
#6556=CIRCLE('',#16851,1.5);
#6557=CIRCLE('',#16854,1.5);
#6558=CIRCLE('',#16860,1.5);
#6559=CIRCLE('',#16864,1.5);
#6560=CIRCLE('',#16868,27.);
#6561=CIRCLE('',#16870,27.);
#6562=CIRCLE('',#16875,1.5);
#6563=CIRCLE('',#16876,1.5);
#6564=CIRCLE('',#16877,1.5);
#6565=CIRCLE('',#16881,1.5);
#6566=CIRCLE('',#16882,1.5);
#6567=CIRCLE('',#16883,1.5);
#6568=CIRCLE('',#16889,27.);
#6569=CIRCLE('',#16891,25.3786796564404);
#6570=CIRCLE('',#16892,1.5);
#6571=CIRCLE('',#16893,26.4393398282202);
#6572=CIRCLE('',#16894,26.4393398282202);
#6573=CIRCLE('',#16896,26.5606601717798);
#6574=CIRCLE('',#16897,26.5606601717798);
#6575=CIRCLE('',#16899,21.905);
#6576=CIRCLE('',#16901,1.5);
#6577=CIRCLE('',#16902,27.);
#6578=CIRCLE('',#16903,27.);
#6579=CIRCLE('',#16905,27.);
#6580=CIRCLE('',#16906,27.);
#6581=CIRCLE('',#16907,27.);
#6582=CIRCLE('',#16908,27.);
#6583=CIRCLE('',#16909,27.);
#6584=CIRCLE('',#16912,1.5);
#6585=CIRCLE('',#16913,1.5);
#6586=CIRCLE('',#16915,4.5);
#6587=CIRCLE('',#16916,3.);
#6588=CIRCLE('',#16918,1.5);
#6589=CIRCLE('',#16919,1.5);
#6590=CIRCLE('',#16921,1.5);
#6591=CIRCLE('',#16922,3.);
#6592=CIRCLE('',#16925,3.);
#6593=CIRCLE('',#16928,1.5);
#6594=CIRCLE('',#16929,3.);
#6595=CIRCLE('',#16930,4.5);
#6596=CIRCLE('',#16934,3.05);
#6597=CIRCLE('',#16961,3.05);
#6598=CIRCLE('',#16964,21.05);
#6599=CIRCLE('',#16971,20.925);
#6600=CIRCLE('',#16988,20.06595);
#6601=CIRCLE('',#17004,16.425);
#6602=CIRCLE('',#17015,16.425);
#6603=CIRCLE('',#17017,15.56595);
#6604=CIRCLE('',#17028,4.5);
#6605=CIRCLE('',#17029,4.);
#6606=CIRCLE('',#17030,4.);
#6607=CIRCLE('',#17032,4.);
#6608=CIRCLE('',#17033,4.);
#6609=CIRCLE('',#17035,18.);
#6610=CIRCLE('',#17037,4.5);
#6611=CIRCLE('',#17039,15.7);
#6612=CIRCLE('',#17041,24.5);
#6613=CIRCLE('',#17042,25.3535533905933);
#6614=CIRCLE('',#17043,25.3535533905933);
#6615=CIRCLE('',#17045,26.);
#6616=CIRCLE('',#17047,15.56595);
#6617=CIRCLE('',#17049,9.64644660940673);
#6618=CIRCLE('',#17050,10.);
#6619=CIRCLE('',#17052,9.55355339059327);
#6620=CIRCLE('',#17054,8.7);
#6621=CIRCLE('',#17056,4.40999999999999);
#6622=CIRCLE('',#17058,16.425);
#6623=CIRCLE('',#17061,16.425);
#6624=CIRCLE('',#17063,20.925);
#6625=CIRCLE('',#17064,20.925);
#6626=CIRCLE('',#17065,20.06595);
#6627=CIRCLE('',#17069,6.99999999999999);
#6628=CIRCLE('',#17070,6.99999999999999);
#6629=CIRCLE('',#17072,26.);
#6630=CIRCLE('',#17077,5.45);
#6631=CIRCLE('',#17078,5.05000000000001);
#6632=CIRCLE('',#17080,12.2);
#6633=CIRCLE('',#17082,5.05000000000001);
#6634=CIRCLE('',#17084,4.01);
#6635=CIRCLE('',#17086,4.01);
#6636=CIRCLE('',#17088,13.);
#6637=CIRCLE('',#17094,3.05);
#6638=CIRCLE('',#17095,3.05);
#6639=CIRCLE('',#17097,26.);
#6640=CIRCLE('',#17101,18.);
#6641=CIRCLE('',#17103,20.2);
#6642=CIRCLE('',#17106,20.925);
#6643=CIRCLE('',#17108,25.);
#6644=CIRCLE('',#17113,3.05);
#6645=CIRCLE('',#17114,3.05);
#6646=CIRCLE('',#17117,14.2);
#6647=CIRCLE('',#17119,15.);
#6648=CIRCLE('',#17121,15.);
#6649=CIRCLE('',#17123,17.46);
#6650=CIRCLE('',#17125,17.96);
#6651=CIRCLE('',#17127,17.96);
#6652=CIRCLE('',#17129,15.05);
#6653=CIRCLE('',#17131,15.05);
#6654=CIRCLE('',#17133,17.96);
#6655=CIRCLE('',#17135,17.96);
#6656=CIRCLE('',#17137,15.05);
#6657=CIRCLE('',#17139,15.05);
#6658=CIRCLE('',#17141,17.96);
#6659=CIRCLE('',#17143,17.96);
#6660=CIRCLE('',#17145,17.46);
#6661=CIRCLE('',#17148,0.8);
#6662=CIRCLE('',#17149,0.8);
#6663=CIRCLE('',#17154,1.465);
#6664=CIRCLE('',#17155,15.055);
#6665=CIRCLE('',#17158,15.06);
#6666=CIRCLE('',#17159,15.06);
#6667=CIRCLE('',#17161,17.97);
#6668=CIRCLE('',#17163,17.97);
#6669=CIRCLE('',#17167,2.8);
#6670=CIRCLE('',#17169,3.);
#6671=CIRCLE('',#17171,3.);
#6672=CIRCLE('',#17173,2.8);
#6673=CIRCLE('',#17255,2.6);
#6674=CIRCLE('',#17257,3.);
#6675=CIRCLE('',#17259,3.);
#6676=CIRCLE('',#17261,2.5);
#6677=CIRCLE('',#17263,2.5);
#6678=CIRCLE('',#17265,3.);
#6679=CIRCLE('',#17267,3.);
#6680=CIRCLE('',#17269,2.5);
#6681=CIRCLE('',#17271,2.5);
#6682=CIRCLE('',#17273,3.);
#6683=CIRCLE('',#17275,3.);
#6684=CIRCLE('',#17277,2.6);
#6685=CIRCLE('',#17281,11.925);
#6686=CIRCLE('',#17294,11.06595);
#6687=CIRCLE('',#17306,14.5);
#6688=CIRCLE('',#17307,15.3123475237772);
#6689=CIRCLE('',#17308,15.3123475237772);
#6690=CIRCLE('',#17310,22.6876524762228);
#6691=CIRCLE('',#17311,22.6876524762228);
#6692=CIRCLE('',#17313,11.06595);
#6693=CIRCLE('',#17315,23.);
#6694=CIRCLE('',#17316,23.);
#6695=CIRCLE('',#17318,23.);
#6696=CIRCLE('',#17320,11.925);
#6697=CIRCLE('',#17321,11.925);
#6698=CIRCLE('',#17324,11.925);
#6699=CIRCLE('',#17326,16.55);
#6700=CIRCLE('',#17327,16.55);
#6701=CIRCLE('',#17329,22.2);
#6702=CIRCLE('',#17332,11.2);
#6703=CIRCLE('',#17334,5.05);
#6704=CIRCLE('',#17336,5.05);
#6705=CIRCLE('',#17338,17.5);
#6706=CIRCLE('',#17340,17.5);
#6707=CIRCLE('',#17344,4.942);
#6708=CIRCLE('',#17358,4.372);
#6709=CIRCLE('',#17360,4.372);
#6710=CIRCLE('',#17376,6.6);
#6711=CIRCLE('',#17381,7.);
#6712=CIRCLE('',#17382,7.);
#6713=CIRCLE('',#17383,7.);
#6714=CIRCLE('',#17384,7.);
#6715=CIRCLE('',#17385,7.);
#6716=CIRCLE('',#17386,7.);
#6717=CIRCLE('',#17387,7.);
#6718=CIRCLE('',#17388,7.);
#6719=CIRCLE('',#17389,7.);
#6720=CIRCLE('',#17390,7.);
#6721=CIRCLE('',#17391,7.);
#6722=CIRCLE('',#17392,7.);
#6723=CIRCLE('',#17393,7.);
#6724=CIRCLE('',#17394,7.);
#6725=CIRCLE('',#17395,7.);
#6726=CIRCLE('',#17396,7.);
#6727=CIRCLE('',#17397,7.);
#6728=CIRCLE('',#17398,7.);
#6729=CIRCLE('',#17399,7.);
#6730=CIRCLE('',#17400,7.);
#6731=CIRCLE('',#17401,7.);
#6732=CIRCLE('',#17402,7.);
#6733=CIRCLE('',#17403,7.);
#6734=CIRCLE('',#17404,7.);
#6735=CIRCLE('',#17405,7.);
#6736=CIRCLE('',#17406,7.);
#6737=CIRCLE('',#17407,7.);
#6738=CIRCLE('',#17408,7.);
#6739=CIRCLE('',#17409,7.);
#6740=CIRCLE('',#17410,7.);
#6741=CIRCLE('',#17411,7.);
#6742=CIRCLE('',#17412,7.);
#6743=CIRCLE('',#17413,7.);
#6744=CIRCLE('',#17414,7.);
#6745=CIRCLE('',#17415,7.);
#6746=CIRCLE('',#17416,7.);
#6747=CIRCLE('',#17417,7.);
#6748=CIRCLE('',#17418,7.);
#6749=CIRCLE('',#17419,7.);
#6750=CIRCLE('',#17420,7.);
#6751=CIRCLE('',#17421,7.);
#6752=CIRCLE('',#17422,7.);
#6753=CIRCLE('',#17423,7.);
#6754=CIRCLE('',#17424,7.);
#6755=CIRCLE('',#17425,7.);
#6756=CIRCLE('',#17426,7.);
#6757=CIRCLE('',#17427,7.);
#6758=CIRCLE('',#17428,7.);
#6759=CIRCLE('',#17429,7.);
#6760=CIRCLE('',#17430,7.);
#6761=CIRCLE('',#17431,7.);
#6762=CIRCLE('',#17432,7.);
#6763=CIRCLE('',#17433,7.);
#6764=CIRCLE('',#17434,7.);
#6765=CIRCLE('',#17435,7.);
#6766=CIRCLE('',#17436,7.);
#6767=CIRCLE('',#17438,6.6);
#6768=CIRCLE('',#17441,4.942);
#6769=CIRCLE('',#17442,4.942);
#6770=CIRCLE('',#17443,4.372);
#6771=CIRCLE('',#17543,4.6);
#6772=CIRCLE('',#17546,4.942);
#6773=CIRCLE('',#17548,6.6);
#6774=CIRCLE('',#17553,10.);
#6775=CIRCLE('',#17554,9.5);
#6776=CIRCLE('',#17555,9.5);
#6777=CIRCLE('',#17557,9.5);
#6778=CIRCLE('',#17559,12.05);
#6779=CIRCLE('',#17561,12.05);
#6780=CIRCLE('',#17563,12.6);
#6781=CIRCLE('',#17565,13.);
#6782=CIRCLE('',#17567,13.);
#6783=CIRCLE('',#17569,10.);
#6784=CIRCLE('',#17574,7.50000000000002);
#6785=CIRCLE('',#17575,8.47434164902529);
#6786=CIRCLE('',#17576,8.47434164902529);
#6787=CIRCLE('',#17578,12.0256583509747);
#6788=CIRCLE('',#17579,12.0256583509747);
#6789=CIRCLE('',#17582,12.7906190968596);
#6790=CIRCLE('',#17583,12.7906190968596);
#6791=CIRCLE('',#17585,14.7093809031404);
#6792=CIRCLE('',#17586,14.7093809031404);
#6793=CIRCLE('',#17588,15.);
#6794=CIRCLE('',#17589,15.);
#6795=CIRCLE('',#17591,15.);
#6796=CIRCLE('',#17593,13.);
#6797=CIRCLE('',#17594,13.);
#6798=CIRCLE('',#17596,14.3);
#6799=CIRCLE('',#17599,10.);
#6800=CIRCLE('',#17603,4.942);
#6801=CIRCLE('',#17617,4.372);
#6802=CIRCLE('',#17630,4.942);
#6803=CIRCLE('',#17631,4.942);
#6804=CIRCLE('',#17632,4.372);
#6805=CIRCLE('',#17635,4.942);
#6806=CIRCLE('',#17636,4.);
#6807=CIRCLE('',#17673,3.6);
#6808=CIRCLE('',#17674,3.);
#6809=CIRCLE('',#17676,3.6);
#6810=CIRCLE('',#17678,3.);
#6811=CIRCLE('',#17682,13.);
#6812=CIRCLE('',#17685,13.);
#6813=CIRCLE('',#17688,13.);
#6814=CIRCLE('',#17691,13.);
#6815=CIRCLE('',#17694,13.);
#6816=CIRCLE('',#17697,13.);
#6817=CIRCLE('',#17700,13.);
#6818=CIRCLE('',#17703,13.);
#6819=CIRCLE('',#17706,13.);
#6820=CIRCLE('',#17709,13.);
#6821=CIRCLE('',#17712,13.);
#6822=CIRCLE('',#17715,13.);
#6823=CIRCLE('',#17718,13.);
#6824=CIRCLE('',#17721,13.);
#6825=CIRCLE('',#17724,13.);
#6826=CIRCLE('',#17727,13.);
#6827=CIRCLE('',#17730,13.);
#6828=CIRCLE('',#17733,13.);
#6829=CIRCLE('',#17736,13.);
#6830=CIRCLE('',#17739,13.);
#6831=CIRCLE('',#17742,13.);
#6832=CIRCLE('',#17745,13.);
#6833=CIRCLE('',#17748,13.);
#6834=CIRCLE('',#17751,13.);
#6835=CIRCLE('',#17754,13.);
#6836=CIRCLE('',#17757,13.);
#6837=CIRCLE('',#17760,13.);
#6838=CIRCLE('',#17763,13.);
#6839=CIRCLE('',#17766,13.);
#6840=CIRCLE('',#17767,13.);
#6841=CIRCLE('',#17770,13.);
#6842=CIRCLE('',#17771,13.);
#6843=CIRCLE('',#17774,13.);
#6844=CIRCLE('',#17777,13.);
#6845=CIRCLE('',#17780,13.);
#6846=CIRCLE('',#17783,13.);
#6847=CIRCLE('',#17786,13.);
#6848=CIRCLE('',#17789,13.);
#6849=CIRCLE('',#17792,13.);
#6850=CIRCLE('',#17795,13.);
#6851=CIRCLE('',#17798,13.);
#6852=CIRCLE('',#17801,13.);
#6853=CIRCLE('',#17804,13.);
#6854=CIRCLE('',#17807,13.);
#6855=CIRCLE('',#17810,13.);
#6856=CIRCLE('',#17813,13.);
#6857=CIRCLE('',#17816,13.);
#6858=CIRCLE('',#17819,13.);
#6859=CIRCLE('',#17822,13.);
#6860=CIRCLE('',#17825,13.);
#6861=CIRCLE('',#17828,13.);
#6862=CIRCLE('',#17831,13.);
#6863=CIRCLE('',#17834,13.);
#6864=CIRCLE('',#17837,13.);
#6865=CIRCLE('',#17840,13.);
#6866=CIRCLE('',#17843,13.);
#6867=CIRCLE('',#17846,13.);
#6868=CIRCLE('',#17849,13.);
#6869=CIRCLE('',#17852,13.);
#6870=CIRCLE('',#17855,13.);
#6871=CIRCLE('',#17858,13.);
#6872=CIRCLE('',#17861,13.);
#6873=CIRCLE('',#17863,1.5);
#6874=CIRCLE('',#17865,4.5);
#6875=CIRCLE('',#17869,4.);
#6876=CIRCLE('',#17871,12.4);
#6877=CIRCLE('',#17873,13.);
#6878=CIRCLE('',#17875,13.);
#6879=CIRCLE('',#17877,12.4);
#6880=CIRCLE('',#17887,8.5);
#6881=CIRCLE('',#17888,9.);
#6882=CIRCLE('',#17891,3.05);
#6883=CIRCLE('',#17892,3.05);
#6884=CIRCLE('',#17896,9.);
#6885=CIRCLE('',#17897,8.5);
#6886=CIRCLE('',#17904,9.);
#6887=CIRCLE('',#17910,8.);
#6888=CIRCLE('',#17911,3.05);
#6889=CIRCLE('',#17912,3.05);
#6890=CIRCLE('',#17915,8.);
#6891=CIRCLE('',#17916,8.);
#6892=CIRCLE('',#17920,3.05);
#6893=CIRCLE('',#17921,3.05);
#6894=CIRCLE('',#17925,1.);
#6895=CIRCLE('',#17927,1.);
#6896=CIRCLE('',#17930,1.);
#6897=CIRCLE('',#17932,8.);
#6898=CIRCLE('',#17934,3.05);
#6899=CIRCLE('',#17935,3.05);
#6900=CIRCLE('',#17939,1.);
#6901=CIRCLE('',#17940,9.);
#6902=CIRCLE('',#17949,8.);
#6903=CIRCLE('',#17950,8.);
#6904=CIRCLE('',#17952,8.);
#6905=CIRCLE('',#17953,71.9999999999995);
#6906=CIRCLE('',#17960,10.6464466094067);
#6907=CIRCLE('',#17961,11.);
#6908=CIRCLE('',#17963,10.3535533905933);
#6909=CIRCLE('',#17965,11.);
#6910=CIRCLE('',#17967,9.5);
#6911=CIRCLE('',#17969,8.);
#6912=CIRCLE('',#17971,7.);
#6913=CIRCLE('',#17972,4.);
#6914=CIRCLE('',#17973,11.);
#6915=CIRCLE('',#17974,11.);
#6916=CIRCLE('',#17976,11.);
#6917=CIRCLE('',#17977,11.);
#6918=CIRCLE('',#17980,8.);
#6919=CIRCLE('',#17982,8.);
#6920=CIRCLE('',#17983,71.9999999999995);
#6921=CIRCLE('',#17986,68.9999999999995);
#6922=CIRCLE('',#17989,6.);
#6923=CIRCLE('',#17990,5.8);
#6924=CIRCLE('',#17993,6.);
#6925=CIRCLE('',#17994,5.8);
#6926=CIRCLE('',#17998,6.);
#6927=CIRCLE('',#18000,3.05);
#6928=CIRCLE('',#18001,3.05);
#6929=CIRCLE('',#18004,5.85857864376269);
#6930=CIRCLE('',#18007,5.85857864376269);
#6931=CIRCLE('',#18008,6.);
#6932=CIRCLE('',#18010,5.74142135623731);
#6933=CIRCLE('',#18014,5.4);
#6934=CIRCLE('',#18017,5.74142135623731);
#6935=CIRCLE('',#18018,5.4);
#6936=CIRCLE('',#18021,3.05);
#6937=CIRCLE('',#18022,3.05);
#6938=CIRCLE('',#18030,2.6);
#6939=CIRCLE('',#18032,3.);
#6940=CIRCLE('',#18034,3.);
#6941=CIRCLE('',#18036,2.5);
#6942=CIRCLE('',#18038,2.5);
#6943=CIRCLE('',#18040,3.);
#6944=CIRCLE('',#18042,3.);
#6945=CIRCLE('',#18044,2.5);
#6946=CIRCLE('',#18046,2.5);
#6947=CIRCLE('',#18048,3.);
#6948=CIRCLE('',#18050,3.);
#6949=CIRCLE('',#18052,2.6);
#6950=CIRCLE('',#18056,5.11);
#6951=CIRCLE('',#18057,5.5);
#6952=CIRCLE('',#18063,5.5);
#6953=CIRCLE('',#18065,3.05);
#6954=CIRCLE('',#18067,5.11);
#6955=CIRCLE('',#18073,3.05);
#6956=CIRCLE('',#18076,3.99);
#6957=CIRCLE('',#18078,3.49);
#6958=CIRCLE('',#18080,3.99);
#6959=CIRCLE('',#18084,5.5);
#6960=CIRCLE('',#18085,5.5);
#6961=CIRCLE('',#18088,2.5);
#6962=CIRCLE('',#18089,2.5);
#6963=VERTEX_POINT('',#22167);
#6964=VERTEX_POINT('',#22168);
#6965=VERTEX_POINT('',#22171);
#6966=VERTEX_POINT('',#22175);
#6967=VERTEX_POINT('',#22179);
#6968=VERTEX_POINT('',#22182);
#6969=VERTEX_POINT('',#22186);
#6970=VERTEX_POINT('',#22187);
#6971=VERTEX_POINT('',#22189);
#6972=VERTEX_POINT('',#22191);
#6973=VERTEX_POINT('',#22193);
#6974=VERTEX_POINT('',#22195);
#6975=VERTEX_POINT('',#22197);
#6976=VERTEX_POINT('',#22199);
#6977=VERTEX_POINT('',#22201);
#6978=VERTEX_POINT('',#22203);
#6979=VERTEX_POINT('',#22230);
#6980=VERTEX_POINT('',#22231);
#6981=VERTEX_POINT('',#22287);
#6982=VERTEX_POINT('',#22292);
#6983=VERTEX_POINT('',#22369);
#6984=VERTEX_POINT('',#22375);
#6985=VERTEX_POINT('',#22383);
#6986=VERTEX_POINT('',#22384);
#6987=VERTEX_POINT('',#22389);
#6988=VERTEX_POINT('',#22391);
#6989=VERTEX_POINT('',#22393);
#6990=VERTEX_POINT('',#22395);
#6991=VERTEX_POINT('',#22397);
#6992=VERTEX_POINT('',#22399);
#6993=VERTEX_POINT('',#22401);
#6994=VERTEX_POINT('',#22403);
#6995=VERTEX_POINT('',#22405);
#6996=VERTEX_POINT('',#22407);
#6997=VERTEX_POINT('',#22409);
#6998=VERTEX_POINT('',#22411);
#6999=VERTEX_POINT('',#22415);
#7000=VERTEX_POINT('',#22419);
#7001=VERTEX_POINT('',#22421);
#7002=VERTEX_POINT('',#22423);
#7003=VERTEX_POINT('',#22450);
#7004=VERTEX_POINT('',#22451);
#7005=VERTEX_POINT('',#22507);
#7006=VERTEX_POINT('',#22512);
#7007=VERTEX_POINT('',#22593);
#7008=VERTEX_POINT('',#22594);
#7009=VERTEX_POINT('',#22650);
#7010=VERTEX_POINT('',#22655);
#7011=VERTEX_POINT('',#22728);
#7012=VERTEX_POINT('',#22733);
#7013=VERTEX_POINT('',#22755);
#7014=VERTEX_POINT('',#22756);
#7015=VERTEX_POINT('',#22758);
#7016=VERTEX_POINT('',#22763);
#7017=VERTEX_POINT('',#22794);
#7018=VERTEX_POINT('',#22795);
#7019=VERTEX_POINT('',#22797);
#7020=VERTEX_POINT('',#22799);
#7021=VERTEX_POINT('',#22842);
#7022=VERTEX_POINT('',#22843);
#7023=VERTEX_POINT('',#22845);
#7024=VERTEX_POINT('',#22850);
#7025=VERTEX_POINT('',#22896);
#7026=VERTEX_POINT('',#22901);
#7027=VERTEX_POINT('',#22932);
#7028=VERTEX_POINT('',#22934);
#7029=VERTEX_POINT('',#22938);
#7030=VERTEX_POINT('',#22940);
#7031=VERTEX_POINT('',#22944);
#7032=VERTEX_POINT('',#22948);
#7033=VERTEX_POINT('',#22952);
#7034=VERTEX_POINT('',#22953);
#7035=VERTEX_POINT('',#22955);
#7036=VERTEX_POINT('',#22957);
#7037=VERTEX_POINT('',#22961);
#7038=VERTEX_POINT('',#22968);
#7039=VERTEX_POINT('',#22970);
#7040=VERTEX_POINT('',#22985);
#7041=VERTEX_POINT('',#22987);
#7042=VERTEX_POINT('',#23000);
#7043=VERTEX_POINT('',#23004);
#7044=VERTEX_POINT('',#23006);
#7045=VERTEX_POINT('',#23010);
#7046=VERTEX_POINT('',#23021);
#7047=VERTEX_POINT('',#23022);
#7048=VERTEX_POINT('',#23038);
#7049=VERTEX_POINT('',#23039);
#7050=VERTEX_POINT('',#23044);
#7051=VERTEX_POINT('',#23052);
#7052=VERTEX_POINT('',#23053);
#7053=VERTEX_POINT('',#23055);
#7054=VERTEX_POINT('',#23059);
#7055=VERTEX_POINT('',#23060);
#7056=VERTEX_POINT('',#23071);
#7057=VERTEX_POINT('',#23075);
#7058=VERTEX_POINT('',#23085);
#7059=VERTEX_POINT('',#23090);
#7060=VERTEX_POINT('',#23094);
#7061=VERTEX_POINT('',#23102);
#7062=VERTEX_POINT('',#23103);
#7063=VERTEX_POINT('',#23105);
#7064=VERTEX_POINT('',#23115);
#7065=VERTEX_POINT('',#23116);
#7066=VERTEX_POINT('',#23120);
#7067=VERTEX_POINT('',#23124);
#7068=VERTEX_POINT('',#23128);
#7069=VERTEX_POINT('',#23132);
#7070=VERTEX_POINT('',#23136);
#7071=VERTEX_POINT('',#23140);
#7072=VERTEX_POINT('',#23144);
#7073=VERTEX_POINT('',#23148);
#7074=VERTEX_POINT('',#23152);
#7075=VERTEX_POINT('',#23159);
#7076=VERTEX_POINT('',#23160);
#7077=VERTEX_POINT('',#23162);
#7078=VERTEX_POINT('',#23164);
#7079=VERTEX_POINT('',#23166);
#7080=VERTEX_POINT('',#23168);
#7081=VERTEX_POINT('',#23170);
#7082=VERTEX_POINT('',#23172);
#7083=VERTEX_POINT('',#23175);
#7084=VERTEX_POINT('',#23176);
#7085=VERTEX_POINT('',#23180);
#7086=VERTEX_POINT('',#23184);
#7087=VERTEX_POINT('',#23188);
#7088=VERTEX_POINT('',#23192);
#7089=VERTEX_POINT('',#23196);
#7090=VERTEX_POINT('',#23200);
#7091=VERTEX_POINT('',#23204);
#7092=VERTEX_POINT('',#23208);
#7093=VERTEX_POINT('',#23212);
#7094=VERTEX_POINT('',#23216);
#7095=VERTEX_POINT('',#23220);
#7096=VERTEX_POINT('',#23224);
#7097=VERTEX_POINT('',#23228);
#7098=VERTEX_POINT('',#23232);
#7099=VERTEX_POINT('',#23239);
#7100=VERTEX_POINT('',#23240);
#7101=VERTEX_POINT('',#23242);
#7102=VERTEX_POINT('',#23244);
#7103=VERTEX_POINT('',#23246);
#7104=VERTEX_POINT('',#23248);
#7105=VERTEX_POINT('',#23250);
#7106=VERTEX_POINT('',#23252);
#7107=VERTEX_POINT('',#23254);
#7108=VERTEX_POINT('',#23256);
#7109=VERTEX_POINT('',#23264);
#7110=VERTEX_POINT('',#23272);
#7111=VERTEX_POINT('',#23274);
#7112=VERTEX_POINT('',#23279);
#7113=VERTEX_POINT('',#23298);
#7114=VERTEX_POINT('',#23332);
#7115=VERTEX_POINT('',#23333);
#7116=VERTEX_POINT('',#23338);
#7117=VERTEX_POINT('',#23355);
#7118=VERTEX_POINT('',#23372);
#7119=VERTEX_POINT('',#23373);
#7120=VERTEX_POINT('',#23375);
#7121=VERTEX_POINT('',#23382);
#7122=VERTEX_POINT('',#23386);
#7123=VERTEX_POINT('',#23399);
#7124=VERTEX_POINT('',#23401);
#7125=VERTEX_POINT('',#23418);
#7126=VERTEX_POINT('',#23420);
#7127=VERTEX_POINT('',#23422);
#7128=VERTEX_POINT('',#23426);
#7129=VERTEX_POINT('',#23428);
#7130=VERTEX_POINT('',#23432);
#7131=VERTEX_POINT('',#23435);
#7132=VERTEX_POINT('',#23437);
#7133=VERTEX_POINT('',#23441);
#7134=VERTEX_POINT('',#23446);
#7135=VERTEX_POINT('',#23453);
#7136=VERTEX_POINT('',#23454);
#7137=VERTEX_POINT('',#23456);
#7138=VERTEX_POINT('',#23458);
#7139=VERTEX_POINT('',#23465);
#7140=VERTEX_POINT('',#23467);
#7141=VERTEX_POINT('',#23492);
#7142=VERTEX_POINT('',#23515);
#7143=VERTEX_POINT('',#23528);
#7144=VERTEX_POINT('',#23530);
#7145=VERTEX_POINT('',#23541);
#7146=VERTEX_POINT('',#23552);
#7147=VERTEX_POINT('',#23563);
#7148=VERTEX_POINT('',#23574);
#7149=VERTEX_POINT('',#23585);
#7150=VERTEX_POINT('',#23596);
#7151=VERTEX_POINT('',#23607);
#7152=VERTEX_POINT('',#23618);
#7153=VERTEX_POINT('',#23629);
#7154=VERTEX_POINT('',#23645);
#7155=VERTEX_POINT('',#23647);
#7156=VERTEX_POINT('',#23651);
#7157=VERTEX_POINT('',#23655);
#7158=VERTEX_POINT('',#23659);
#7159=VERTEX_POINT('',#23663);
#7160=VERTEX_POINT('',#23667);
#7161=VERTEX_POINT('',#23671);
#7162=VERTEX_POINT('',#23683);
#7163=VERTEX_POINT('',#23685);
#7164=VERTEX_POINT('',#23696);
#7165=VERTEX_POINT('',#23707);
#7166=VERTEX_POINT('',#23718);
#7167=VERTEX_POINT('',#23729);
#7168=VERTEX_POINT('',#23740);
#7169=VERTEX_POINT('',#23751);
#7170=VERTEX_POINT('',#23762);
#7171=VERTEX_POINT('',#23773);
#7172=VERTEX_POINT('',#23784);
#7173=VERTEX_POINT('',#23795);
#7174=VERTEX_POINT('',#23806);
#7175=VERTEX_POINT('',#23817);
#7176=VERTEX_POINT('',#23828);
#7177=VERTEX_POINT('',#23839);
#7178=VERTEX_POINT('',#23855);
#7179=VERTEX_POINT('',#23857);
#7180=VERTEX_POINT('',#23861);
#7181=VERTEX_POINT('',#23865);
#7182=VERTEX_POINT('',#23869);
#7183=VERTEX_POINT('',#23873);
#7184=VERTEX_POINT('',#23877);
#7185=VERTEX_POINT('',#23881);
#7186=VERTEX_POINT('',#23885);
#7187=VERTEX_POINT('',#23889);
#7188=VERTEX_POINT('',#23896);
#7189=VERTEX_POINT('',#23901);
#7190=VERTEX_POINT('',#23911);
#7191=VERTEX_POINT('',#23912);
#7192=VERTEX_POINT('',#23914);
#7193=VERTEX_POINT('',#23931);
#7194=VERTEX_POINT('',#23944);
#7195=VERTEX_POINT('',#23945);
#7196=VERTEX_POINT('',#24028);
#7197=VERTEX_POINT('',#24029);
#7198=VERTEX_POINT('',#24118);
#7199=VERTEX_POINT('',#24119);
#7200=VERTEX_POINT('',#24208);
#7201=VERTEX_POINT('',#24209);
#7202=VERTEX_POINT('',#24292);
#7203=VERTEX_POINT('',#24293);
#7204=VERTEX_POINT('',#24382);
#7205=VERTEX_POINT('',#24383);
#7206=VERTEX_POINT('',#24466);
#7207=VERTEX_POINT('',#24467);
#7208=VERTEX_POINT('',#24556);
#7209=VERTEX_POINT('',#24557);
#7210=VERTEX_POINT('',#24646);
#7211=VERTEX_POINT('',#24647);
#7212=VERTEX_POINT('',#24730);
#7213=VERTEX_POINT('',#24731);
#7214=VERTEX_POINT('',#24820);
#7215=VERTEX_POINT('',#24821);
#7216=VERTEX_POINT('',#24910);
#7217=VERTEX_POINT('',#24911);
#7218=VERTEX_POINT('',#24994);
#7219=VERTEX_POINT('',#24995);
#7220=VERTEX_POINT('',#25084);
#7221=VERTEX_POINT('',#25085);
#7222=VERTEX_POINT('',#25168);
#7223=VERTEX_POINT('',#25169);
#7224=VERTEX_POINT('',#25258);
#7225=VERTEX_POINT('',#25259);
#7226=VERTEX_POINT('',#25261);
#7227=VERTEX_POINT('',#25277);
#7228=VERTEX_POINT('',#25292);
#7229=VERTEX_POINT('',#25293);
#7230=VERTEX_POINT('',#25329);
#7231=VERTEX_POINT('',#25330);
#7232=VERTEX_POINT('',#25366);
#7233=VERTEX_POINT('',#25367);
#7234=VERTEX_POINT('',#25403);
#7235=VERTEX_POINT('',#25404);
#7236=VERTEX_POINT('',#25440);
#7237=VERTEX_POINT('',#25441);
#7238=VERTEX_POINT('',#25478);
#7239=VERTEX_POINT('',#25479);
#7240=VERTEX_POINT('',#25515);
#7241=VERTEX_POINT('',#25516);
#7242=VERTEX_POINT('',#25552);
#7243=VERTEX_POINT('',#25553);
#7244=VERTEX_POINT('',#25590);
#7245=VERTEX_POINT('',#25591);
#7246=VERTEX_POINT('',#25627);
#7247=VERTEX_POINT('',#25628);
#7248=VERTEX_POINT('',#25664);
#7249=VERTEX_POINT('',#25665);
#7250=VERTEX_POINT('',#25701);
#7251=VERTEX_POINT('',#25702);
#7252=VERTEX_POINT('',#25738);
#7253=VERTEX_POINT('',#25739);
#7254=VERTEX_POINT('',#25776);
#7255=VERTEX_POINT('',#25777);
#7256=VERTEX_POINT('',#25813);
#7257=VERTEX_POINT('',#25814);
#7258=VERTEX_POINT('',#25816);
#7259=VERTEX_POINT('',#25833);
#7260=VERTEX_POINT('',#25846);
#7261=VERTEX_POINT('',#25847);
#7262=VERTEX_POINT('',#25936);
#7263=VERTEX_POINT('',#25937);
#7264=VERTEX_POINT('',#26020);
#7265=VERTEX_POINT('',#26021);
#7266=VERTEX_POINT('',#26110);
#7267=VERTEX_POINT('',#26111);
#7268=VERTEX_POINT('',#26200);
#7269=VERTEX_POINT('',#26201);
#7270=VERTEX_POINT('',#26290);
#7271=VERTEX_POINT('',#26291);
#7272=VERTEX_POINT('',#26374);
#7273=VERTEX_POINT('',#26375);
#7274=VERTEX_POINT('',#26464);
#7275=VERTEX_POINT('',#26465);
#7276=VERTEX_POINT('',#26554);
#7277=VERTEX_POINT('',#26555);
#7278=VERTEX_POINT('',#26641);
#7279=VERTEX_POINT('',#26642);
#7280=VERTEX_POINT('',#26644);
#7281=VERTEX_POINT('',#26724);
#7282=VERTEX_POINT('',#26725);
#7283=VERTEX_POINT('',#26727);
#7284=VERTEX_POINT('',#26738);
#7285=VERTEX_POINT('',#26749);
#7286=VERTEX_POINT('',#26750);
#7287=VERTEX_POINT('',#26787);
#7288=VERTEX_POINT('',#26788);
#7289=VERTEX_POINT('',#26824);
#7290=VERTEX_POINT('',#26825);
#7291=VERTEX_POINT('',#26862);
#7292=VERTEX_POINT('',#26863);
#7293=VERTEX_POINT('',#26899);
#7294=VERTEX_POINT('',#26900);
#7295=VERTEX_POINT('',#26936);
#7296=VERTEX_POINT('',#26937);
#7297=VERTEX_POINT('',#26974);
#7298=VERTEX_POINT('',#26975);
#7299=VERTEX_POINT('',#27012);
#7300=VERTEX_POINT('',#27013);
#7301=VERTEX_POINT('',#27049);
#7302=VERTEX_POINT('',#27050);
#7303=VERTEX_POINT('',#27086);
#7304=VERTEX_POINT('',#27088);
#7305=VERTEX_POINT('',#27090);
#7306=VERTEX_POINT('',#27094);
#7307=VERTEX_POINT('',#27095);
#7308=VERTEX_POINT('',#27100);
#7309=VERTEX_POINT('',#27103);
#7310=VERTEX_POINT('',#27107);
#7311=VERTEX_POINT('',#27110);
#7312=VERTEX_POINT('',#27112);
#7313=VERTEX_POINT('',#27114);
#7314=VERTEX_POINT('',#27118);
#7315=VERTEX_POINT('',#27122);
#7316=VERTEX_POINT('',#27262);
#7317=VERTEX_POINT('',#27404);
#7318=VERTEX_POINT('',#27406);
#7319=VERTEX_POINT('',#27408);
#7320=VERTEX_POINT('',#27415);
#7321=VERTEX_POINT('',#27424);
#7322=VERTEX_POINT('',#27428);
#7323=VERTEX_POINT('',#27432);
#7324=VERTEX_POINT('',#27574);
#7325=VERTEX_POINT('',#29657);
#7326=VERTEX_POINT('',#29810);
#7327=VERTEX_POINT('',#29956);
#7328=VERTEX_POINT('',#29959);
#7329=VERTEX_POINT('',#30922);
#7330=VERTEX_POINT('',#31064);
#7331=VERTEX_POINT('',#31065);
#7332=VERTEX_POINT('',#31072);
#7333=VERTEX_POINT('',#31074);
#7334=VERTEX_POINT('',#31087);
#7335=VERTEX_POINT('',#31089);
#7336=VERTEX_POINT('',#31096);
#7337=VERTEX_POINT('',#31098);
#7338=VERTEX_POINT('',#31117);
#7339=VERTEX_POINT('',#31126);
#7340=VERTEX_POINT('',#31139);
#7341=VERTEX_POINT('',#31143);
#7342=VERTEX_POINT('',#31156);
#7343=VERTEX_POINT('',#31157);
#7344=VERTEX_POINT('',#31171);
#7345=VERTEX_POINT('',#31173);
#7346=VERTEX_POINT('',#31186);
#7347=VERTEX_POINT('',#31188);
#7348=VERTEX_POINT('',#31192);
#7349=VERTEX_POINT('',#31195);
#7350=VERTEX_POINT('',#31199);
#7351=VERTEX_POINT('',#31203);
#7352=VERTEX_POINT('',#31207);
#7353=VERTEX_POINT('',#31211);
#7354=VERTEX_POINT('',#31301);
#7355=VERTEX_POINT('',#31303);
#7356=VERTEX_POINT('',#31307);
#7357=VERTEX_POINT('',#31315);
#7358=VERTEX_POINT('',#31319);
#7359=VERTEX_POINT('',#31326);
#7360=VERTEX_POINT('',#31334);
#7361=VERTEX_POINT('',#31336);
#7362=VERTEX_POINT('',#31341);
#7363=VERTEX_POINT('',#31344);
#7364=VERTEX_POINT('',#31348);
#7365=VERTEX_POINT('',#31352);
#7366=VERTEX_POINT('',#31355);
#7367=VERTEX_POINT('',#31359);
#7368=VERTEX_POINT('',#31363);
#7369=VERTEX_POINT('',#31366);
#7370=VERTEX_POINT('',#31370);
#7371=VERTEX_POINT('',#31373);
#7372=VERTEX_POINT('',#31377);
#7373=VERTEX_POINT('',#31380);
#7374=VERTEX_POINT('',#31384);
#7375=VERTEX_POINT('',#31387);
#7376=VERTEX_POINT('',#31391);
#7377=VERTEX_POINT('',#32146);
#7378=VERTEX_POINT('',#32148);
#7379=VERTEX_POINT('',#32229);
#7380=VERTEX_POINT('',#32234);
#7381=VERTEX_POINT('',#32236);
#7382=VERTEX_POINT('',#32240);
#7383=VERTEX_POINT('',#32243);
#7384=VERTEX_POINT('',#32249);
#7385=VERTEX_POINT('',#32252);
#7386=VERTEX_POINT('',#32256);
#7387=VERTEX_POINT('',#32260);
#7388=VERTEX_POINT('',#32266);
#7389=VERTEX_POINT('',#32267);
#7390=VERTEX_POINT('',#32269);
#7391=VERTEX_POINT('',#32271);
#7392=VERTEX_POINT('',#32275);
#7393=VERTEX_POINT('',#32277);
#7394=VERTEX_POINT('',#32279);
#7395=VERTEX_POINT('',#32281);
#7396=VERTEX_POINT('',#32285);
#7397=VERTEX_POINT('',#32289);
#7398=VERTEX_POINT('',#32290);
#7399=VERTEX_POINT('',#32292);
#7400=VERTEX_POINT('',#32294);
#7401=VERTEX_POINT('',#32298);
#7402=VERTEX_POINT('',#32300);
#7403=VERTEX_POINT('',#32305);
#7404=VERTEX_POINT('',#32307);
#7405=VERTEX_POINT('',#32311);
#7406=VERTEX_POINT('',#32312);
#7407=VERTEX_POINT('',#32314);
#7408=VERTEX_POINT('',#32316);
#7409=VERTEX_POINT('',#32318);
#7410=VERTEX_POINT('',#32320);
#7411=VERTEX_POINT('',#32324);
#7412=VERTEX_POINT('',#32326);
#7413=VERTEX_POINT('',#32330);
#7414=VERTEX_POINT('',#32332);
#7415=VERTEX_POINT('',#32334);
#7416=VERTEX_POINT('',#32338);
#7417=VERTEX_POINT('',#32340);
#7418=VERTEX_POINT('',#32344);
#7419=VERTEX_POINT('',#32345);
#7420=VERTEX_POINT('',#32347);
#7421=VERTEX_POINT('',#32349);
#7422=VERTEX_POINT('',#32351);
#7423=VERTEX_POINT('',#32355);
#7424=VERTEX_POINT('',#32357);
#7425=VERTEX_POINT('',#32361);
#7426=VERTEX_POINT('',#32366);
#7427=VERTEX_POINT('',#32368);
#7428=VERTEX_POINT('',#32370);
#7429=VERTEX_POINT('',#32372);
#7430=VERTEX_POINT('',#32376);
#7431=VERTEX_POINT('',#32378);
#7432=VERTEX_POINT('',#32380);
#7433=VERTEX_POINT('',#32384);
#7434=VERTEX_POINT('',#32388);
#7435=VERTEX_POINT('',#32389);
#7436=VERTEX_POINT('',#32391);
#7437=VERTEX_POINT('',#32393);
#7438=VERTEX_POINT('',#32397);
#7439=VERTEX_POINT('',#32399);
#7440=VERTEX_POINT('',#32405);
#7441=VERTEX_POINT('',#32409);
#7442=VERTEX_POINT('',#32415);
#7443=VERTEX_POINT('',#32421);
#7444=VERTEX_POINT('',#32422);
#7445=VERTEX_POINT('',#32424);
#7446=VERTEX_POINT('',#32426);
#7447=VERTEX_POINT('',#32428);
#7448=VERTEX_POINT('',#32436);
#7449=VERTEX_POINT('',#32437);
#7450=VERTEX_POINT('',#32441);
#7451=VERTEX_POINT('',#32443);
#7452=VERTEX_POINT('',#32445);
#7453=VERTEX_POINT('',#32447);
#7454=VERTEX_POINT('',#32449);
#7455=VERTEX_POINT('',#32451);
#7456=VERTEX_POINT('',#32455);
#7457=VERTEX_POINT('',#32459);
#7458=VERTEX_POINT('',#32461);
#7459=VERTEX_POINT('',#32463);
#7460=VERTEX_POINT('',#32465);
#7461=VERTEX_POINT('',#32469);
#7462=VERTEX_POINT('',#32473);
#7463=VERTEX_POINT('',#32475);
#7464=VERTEX_POINT('',#32477);
#7465=VERTEX_POINT('',#32479);
#7466=VERTEX_POINT('',#32481);
#7467=VERTEX_POINT('',#32486);
#7468=VERTEX_POINT('',#32487);
#7469=VERTEX_POINT('',#32489);
#7470=VERTEX_POINT('',#32491);
#7471=VERTEX_POINT('',#32493);
#7472=VERTEX_POINT('',#32495);
#7473=VERTEX_POINT('',#32497);
#7474=VERTEX_POINT('',#32499);
#7475=VERTEX_POINT('',#32502);
#7476=VERTEX_POINT('',#32503);
#7477=VERTEX_POINT('',#32507);
#7478=VERTEX_POINT('',#32511);
#7479=VERTEX_POINT('',#32515);
#7480=VERTEX_POINT('',#32519);
#7481=VERTEX_POINT('',#32523);
#7482=VERTEX_POINT('',#32527);
#7483=VERTEX_POINT('',#32531);
#7484=VERTEX_POINT('',#32535);
#7485=VERTEX_POINT('',#32539);
#7486=VERTEX_POINT('',#32543);
#7487=VERTEX_POINT('',#32550);
#7488=VERTEX_POINT('',#32551);
#7489=VERTEX_POINT('',#32555);
#7490=VERTEX_POINT('',#32557);
#7491=VERTEX_POINT('',#32559);
#7492=VERTEX_POINT('',#32561);
#7493=VERTEX_POINT('',#32563);
#7494=VERTEX_POINT('',#32567);
#7495=VERTEX_POINT('',#32571);
#7496=VERTEX_POINT('',#32576);
#7497=VERTEX_POINT('',#32577);
#7498=VERTEX_POINT('',#32581);
#7499=VERTEX_POINT('',#32583);
#7500=VERTEX_POINT('',#32585);
#7501=VERTEX_POINT('',#32587);
#7502=VERTEX_POINT('',#32589);
#7503=VERTEX_POINT('',#32591);
#7504=VERTEX_POINT('',#32595);
#7505=VERTEX_POINT('',#32599);
#7506=VERTEX_POINT('',#32603);
#7507=VERTEX_POINT('',#32607);
#7508=VERTEX_POINT('',#32611);
#7509=VERTEX_POINT('',#32615);
#7510=VERTEX_POINT('',#32619);
#7511=VERTEX_POINT('',#32623);
#7512=VERTEX_POINT('',#32627);
#7513=VERTEX_POINT('',#32631);
#7514=VERTEX_POINT('',#32635);
#7515=VERTEX_POINT('',#32637);
#7516=VERTEX_POINT('',#32641);
#7517=VERTEX_POINT('',#32645);
#7518=VERTEX_POINT('',#32649);
#7519=VERTEX_POINT('',#32653);
#7520=VERTEX_POINT('',#32657);
#7521=VERTEX_POINT('',#32661);
#7522=VERTEX_POINT('',#32665);
#7523=VERTEX_POINT('',#32669);
#7524=VERTEX_POINT('',#32673);
#7525=VERTEX_POINT('',#32681);
#7526=VERTEX_POINT('',#32683);
#7527=VERTEX_POINT('',#32685);
#7528=VERTEX_POINT('',#32694);
#7529=VERTEX_POINT('',#32709);
#7530=VERTEX_POINT('',#32711);
#7531=VERTEX_POINT('',#32722);
#7532=VERTEX_POINT('',#32728);
#7533=VERTEX_POINT('',#32732);
#7534=VERTEX_POINT('',#32736);
#7535=VERTEX_POINT('',#32740);
#7536=VERTEX_POINT('',#32744);
#7537=VERTEX_POINT('',#32753);
#7538=VERTEX_POINT('',#32764);
#7539=VERTEX_POINT('',#32770);
#7540=VERTEX_POINT('',#32774);
#7541=VERTEX_POINT('',#32778);
#7542=VERTEX_POINT('',#32787);
#7543=VERTEX_POINT('',#32798);
#7544=VERTEX_POINT('',#32804);
#7545=VERTEX_POINT('',#32808);
#7546=VERTEX_POINT('',#32812);
#7547=VERTEX_POINT('',#32816);
#7548=VERTEX_POINT('',#32823);
#7549=VERTEX_POINT('',#32825);
#7550=VERTEX_POINT('',#32829);
#7551=VERTEX_POINT('',#32833);
#7552=VERTEX_POINT('',#32837);
#7553=VERTEX_POINT('',#32841);
#7554=VERTEX_POINT('',#32845);
#7555=VERTEX_POINT('',#32849);
#7556=VERTEX_POINT('',#32861);
#7557=VERTEX_POINT('',#32863);
#7558=VERTEX_POINT('',#32874);
#7559=VERTEX_POINT('',#32885);
#7560=VERTEX_POINT('',#32896);
#7561=VERTEX_POINT('',#32907);
#7562=VERTEX_POINT('',#32918);
#7563=VERTEX_POINT('',#32929);
#7564=VERTEX_POINT('',#32940);
#7565=VERTEX_POINT('',#32951);
#7566=VERTEX_POINT('',#32962);
#7567=VERTEX_POINT('',#32973);
#7568=VERTEX_POINT('',#32994);
#7569=VERTEX_POINT('',#32996);
#7570=VERTEX_POINT('',#33007);
#7571=VERTEX_POINT('',#33013);
#7572=VERTEX_POINT('',#33022);
#7573=VERTEX_POINT('',#33033);
#7574=VERTEX_POINT('',#33039);
#7575=VERTEX_POINT('',#33043);
#7576=VERTEX_POINT('',#33047);
#7577=VERTEX_POINT('',#33059);
#7578=VERTEX_POINT('',#33061);
#7579=VERTEX_POINT('',#33072);
#7580=VERTEX_POINT('',#33083);
#7581=VERTEX_POINT('',#33094);
#7582=VERTEX_POINT('',#33105);
#7583=VERTEX_POINT('',#33116);
#7584=VERTEX_POINT('',#33127);
#7585=VERTEX_POINT('',#33138);
#7586=VERTEX_POINT('',#33149);
#7587=VERTEX_POINT('',#33160);
#7588=VERTEX_POINT('',#33171);
#7589=VERTEX_POINT('',#33182);
#7590=VERTEX_POINT('',#33188);
#7591=VERTEX_POINT('',#33197);
#7592=VERTEX_POINT('',#33208);
#7593=VERTEX_POINT('',#33219);
#7594=VERTEX_POINT('',#33230);
#7595=VERTEX_POINT('',#33241);
#7596=VERTEX_POINT('',#33252);
#7597=VERTEX_POINT('',#33263);
#7598=VERTEX_POINT('',#33274);
#7599=VERTEX_POINT('',#33285);
#7600=VERTEX_POINT('',#33296);
#7601=VERTEX_POINT('',#33307);
#7602=VERTEX_POINT('',#33313);
#7603=VERTEX_POINT('',#33317);
#7604=VERTEX_POINT('',#33321);
#7605=VERTEX_POINT('',#33325);
#7606=VERTEX_POINT('',#33345);
#7607=VERTEX_POINT('',#33348);
#7608=VERTEX_POINT('',#33352);
#7609=VERTEX_POINT('',#33356);
#7610=VERTEX_POINT('',#33359);
#7611=VERTEX_POINT('',#33363);
#7612=VERTEX_POINT('',#33366);
#7613=VERTEX_POINT('',#33370);
#7614=VERTEX_POINT('',#33373);
#7615=VERTEX_POINT('',#33377);
#7616=VERTEX_POINT('',#33380);
#7617=VERTEX_POINT('',#33384);
#7618=VERTEX_POINT('',#33390);
#7619=VERTEX_POINT('',#33391);
#7620=VERTEX_POINT('',#33393);
#7621=VERTEX_POINT('',#33410);
#7622=VERTEX_POINT('',#33423);
#7623=VERTEX_POINT('',#33424);
#7624=VERTEX_POINT('',#33507);
#7625=VERTEX_POINT('',#33508);
#7626=VERTEX_POINT('',#33597);
#7627=VERTEX_POINT('',#33598);
#7628=VERTEX_POINT('',#33687);
#7629=VERTEX_POINT('',#33688);
#7630=VERTEX_POINT('',#33771);
#7631=VERTEX_POINT('',#33772);
#7632=VERTEX_POINT('',#33861);
#7633=VERTEX_POINT('',#33862);
#7634=VERTEX_POINT('',#33951);
#7635=VERTEX_POINT('',#33952);
#7636=VERTEX_POINT('',#34035);
#7637=VERTEX_POINT('',#34036);
#7638=VERTEX_POINT('',#34125);
#7639=VERTEX_POINT('',#34126);
#7640=VERTEX_POINT('',#34215);
#7641=VERTEX_POINT('',#34216);
#7642=VERTEX_POINT('',#34299);
#7643=VERTEX_POINT('',#34300);
#7644=VERTEX_POINT('',#34389);
#7645=VERTEX_POINT('',#34390);
#7646=VERTEX_POINT('',#34392);
#7647=VERTEX_POINT('',#34408);
#7648=VERTEX_POINT('',#34423);
#7649=VERTEX_POINT('',#34424);
#7650=VERTEX_POINT('',#34460);
#7651=VERTEX_POINT('',#34461);
#7652=VERTEX_POINT('',#34497);
#7653=VERTEX_POINT('',#34498);
#7654=VERTEX_POINT('',#34535);
#7655=VERTEX_POINT('',#34536);
#7656=VERTEX_POINT('',#34572);
#7657=VERTEX_POINT('',#34573);
#7658=VERTEX_POINT('',#34609);
#7659=VERTEX_POINT('',#34610);
#7660=VERTEX_POINT('',#34647);
#7661=VERTEX_POINT('',#34648);
#7662=VERTEX_POINT('',#34684);
#7663=VERTEX_POINT('',#34685);
#7664=VERTEX_POINT('',#34721);
#7665=VERTEX_POINT('',#34722);
#7666=VERTEX_POINT('',#34759);
#7667=VERTEX_POINT('',#34760);
#7668=VERTEX_POINT('',#34796);
#7669=VERTEX_POINT('',#34798);
#7670=VERTEX_POINT('',#34800);
#7671=VERTEX_POINT('',#34804);
#7672=VERTEX_POINT('',#34806);
#7673=VERTEX_POINT('',#34810);
#7674=VERTEX_POINT('',#34941);
#7675=VERTEX_POINT('',#35074);
#7676=VERTEX_POINT('',#35076);
#7677=VERTEX_POINT('',#35080);
#7678=VERTEX_POINT('',#35084);
#7679=VERTEX_POINT('',#35215);
#7680=VERTEX_POINT('',#35217);
#7681=VERTEX_POINT('',#36629);
#7682=VERTEX_POINT('',#36631);
#7683=VERTEX_POINT('',#36635);
#7684=VERTEX_POINT('',#36640);
#7685=VERTEX_POINT('',#36644);
#7686=VERTEX_POINT('',#36647);
#7687=VERTEX_POINT('',#36651);
#7688=VERTEX_POINT('',#36654);
#7689=VERTEX_POINT('',#36660);
#7690=VERTEX_POINT('',#36661);
#7691=VERTEX_POINT('',#36663);
#7692=VERTEX_POINT('',#36680);
#7693=VERTEX_POINT('',#36693);
#7694=VERTEX_POINT('',#36694);
#7695=VERTEX_POINT('',#36777);
#7696=VERTEX_POINT('',#36778);
#7697=VERTEX_POINT('',#36867);
#7698=VERTEX_POINT('',#36868);
#7699=VERTEX_POINT('',#36957);
#7700=VERTEX_POINT('',#36958);
#7701=VERTEX_POINT('',#37041);
#7702=VERTEX_POINT('',#37042);
#7703=VERTEX_POINT('',#37131);
#7704=VERTEX_POINT('',#37132);
#7705=VERTEX_POINT('',#37218);
#7706=VERTEX_POINT('',#37219);
#7707=VERTEX_POINT('',#37305);
#7708=VERTEX_POINT('',#37306);
#7709=VERTEX_POINT('',#37395);
#7710=VERTEX_POINT('',#37396);
#7711=VERTEX_POINT('',#37479);
#7712=VERTEX_POINT('',#37480);
#7713=VERTEX_POINT('',#37569);
#7714=VERTEX_POINT('',#37570);
#7715=VERTEX_POINT('',#37659);
#7716=VERTEX_POINT('',#37660);
#7717=VERTEX_POINT('',#37743);
#7718=VERTEX_POINT('',#37744);
#7719=VERTEX_POINT('',#37746);
#7720=VERTEX_POINT('',#37753);
#7721=VERTEX_POINT('',#37754);
#7722=VERTEX_POINT('',#37772);
#7723=VERTEX_POINT('',#37789);
#7724=VERTEX_POINT('',#37790);
#7725=VERTEX_POINT('',#37826);
#7726=VERTEX_POINT('',#37827);
#7727=VERTEX_POINT('',#37864);
#7728=VERTEX_POINT('',#37865);
#7729=VERTEX_POINT('',#37901);
#7730=VERTEX_POINT('',#37902);
#7731=VERTEX_POINT('',#37938);
#7732=VERTEX_POINT('',#37939);
#7733=VERTEX_POINT('',#37976);
#7734=VERTEX_POINT('',#37977);
#7735=VERTEX_POINT('',#38012);
#7736=VERTEX_POINT('',#38013);
#7737=VERTEX_POINT('',#38050);
#7738=VERTEX_POINT('',#38051);
#7739=VERTEX_POINT('',#38087);
#7740=VERTEX_POINT('',#38088);
#7741=VERTEX_POINT('',#38124);
#7742=VERTEX_POINT('',#38125);
#7743=VERTEX_POINT('',#38162);
#7744=VERTEX_POINT('',#38163);
#7745=VERTEX_POINT('',#38199);
#7746=VERTEX_POINT('',#38200);
#7747=VERTEX_POINT('',#38204);
#7748=VERTEX_POINT('',#38206);
#7749=VERTEX_POINT('',#38210);
#7750=VERTEX_POINT('',#38212);
#7751=VERTEX_POINT('',#38218);
#7752=VERTEX_POINT('',#38219);
#7753=VERTEX_POINT('',#38223);
#7754=VERTEX_POINT('',#38225);
#7755=VERTEX_POINT('',#38229);
#7756=VERTEX_POINT('',#38231);
#7757=VERTEX_POINT('',#38236);
#7758=VERTEX_POINT('',#38238);
#7759=VERTEX_POINT('',#38240);
#7760=VERTEX_POINT('',#38242);
#7761=VERTEX_POINT('',#38244);
#7762=VERTEX_POINT('',#38246);
#7763=VERTEX_POINT('',#38249);
#7764=VERTEX_POINT('',#38251);
#7765=VERTEX_POINT('',#38253);
#7766=VERTEX_POINT('',#38255);
#7767=VERTEX_POINT('',#38257);
#7768=VERTEX_POINT('',#38259);
#7769=VERTEX_POINT('',#38262);
#7770=VERTEX_POINT('',#38264);
#7771=VERTEX_POINT('',#38268);
#7772=VERTEX_POINT('',#38270);
#7773=VERTEX_POINT('',#38272);
#7774=VERTEX_POINT('',#38274);
#7775=VERTEX_POINT('',#38276);
#7776=VERTEX_POINT('',#38278);
#7777=VERTEX_POINT('',#38281);
#7778=VERTEX_POINT('',#38282);
#7779=VERTEX_POINT('',#38284);
#7780=VERTEX_POINT('',#38286);
#7781=VERTEX_POINT('',#38289);
#7782=VERTEX_POINT('',#38290);
#7783=VERTEX_POINT('',#38292);
#7784=VERTEX_POINT('',#38294);
#7785=VERTEX_POINT('',#38297);
#7786=VERTEX_POINT('',#38298);
#7787=VERTEX_POINT('',#38300);
#7788=VERTEX_POINT('',#38302);
#7789=VERTEX_POINT('',#38305);
#7790=VERTEX_POINT('',#38306);
#7791=VERTEX_POINT('',#38308);
#7792=VERTEX_POINT('',#38310);
#7793=VERTEX_POINT('',#38313);
#7794=VERTEX_POINT('',#38314);
#7795=VERTEX_POINT('',#38316);
#7796=VERTEX_POINT('',#38318);
#7797=VERTEX_POINT('',#38321);
#7798=VERTEX_POINT('',#38322);
#7799=VERTEX_POINT('',#38324);
#7800=VERTEX_POINT('',#38326);
#7801=VERTEX_POINT('',#38329);
#7802=VERTEX_POINT('',#38330);
#7803=VERTEX_POINT('',#38332);
#7804=VERTEX_POINT('',#38334);
#7805=VERTEX_POINT('',#38337);
#7806=VERTEX_POINT('',#38338);
#7807=VERTEX_POINT('',#38340);
#7808=VERTEX_POINT('',#38342);
#7809=VERTEX_POINT('',#38345);
#7810=VERTEX_POINT('',#38346);
#7811=VERTEX_POINT('',#38348);
#7812=VERTEX_POINT('',#38350);
#7813=VERTEX_POINT('',#38353);
#7814=VERTEX_POINT('',#38354);
#7815=VERTEX_POINT('',#38356);
#7816=VERTEX_POINT('',#38358);
#7817=VERTEX_POINT('',#38361);
#7818=VERTEX_POINT('',#38362);
#7819=VERTEX_POINT('',#38364);
#7820=VERTEX_POINT('',#38366);
#7821=VERTEX_POINT('',#38369);
#7822=VERTEX_POINT('',#38370);
#7823=VERTEX_POINT('',#38372);
#7824=VERTEX_POINT('',#38374);
#7825=VERTEX_POINT('',#38377);
#7826=VERTEX_POINT('',#38378);
#7827=VERTEX_POINT('',#38380);
#7828=VERTEX_POINT('',#38382);
#7829=VERTEX_POINT('',#38385);
#7830=VERTEX_POINT('',#38386);
#7831=VERTEX_POINT('',#38388);
#7832=VERTEX_POINT('',#38390);
#7833=VERTEX_POINT('',#38393);
#7834=VERTEX_POINT('',#38394);
#7835=VERTEX_POINT('',#38396);
#7836=VERTEX_POINT('',#38398);
#7837=VERTEX_POINT('',#38401);
#7838=VERTEX_POINT('',#38402);
#7839=VERTEX_POINT('',#38404);
#7840=VERTEX_POINT('',#38406);
#7841=VERTEX_POINT('',#38409);
#7842=VERTEX_POINT('',#38410);
#7843=VERTEX_POINT('',#38412);
#7844=VERTEX_POINT('',#38414);
#7845=VERTEX_POINT('',#38417);
#7846=VERTEX_POINT('',#38418);
#7847=VERTEX_POINT('',#38420);
#7848=VERTEX_POINT('',#38422);
#7849=VERTEX_POINT('',#38425);
#7850=VERTEX_POINT('',#38426);
#7851=VERTEX_POINT('',#38428);
#7852=VERTEX_POINT('',#38430);
#7853=VERTEX_POINT('',#38433);
#7854=VERTEX_POINT('',#38434);
#7855=VERTEX_POINT('',#38436);
#7856=VERTEX_POINT('',#38438);
#7857=VERTEX_POINT('',#38441);
#7858=VERTEX_POINT('',#38442);
#7859=VERTEX_POINT('',#38444);
#7860=VERTEX_POINT('',#38446);
#7861=VERTEX_POINT('',#39120);
#7862=VERTEX_POINT('',#39243);
#7863=VERTEX_POINT('',#39362);
#7864=VERTEX_POINT('',#39365);
#7865=VERTEX_POINT('',#40148);
#7866=VERTEX_POINT('',#40272);
#7867=VERTEX_POINT('',#40275);
#7868=VERTEX_POINT('',#40280);
#7869=VERTEX_POINT('',#40284);
#7870=VERTEX_POINT('',#40286);
#7871=VERTEX_POINT('',#40295);
#7872=VERTEX_POINT('',#40297);
#7873=VERTEX_POINT('',#40306);
#7874=VERTEX_POINT('',#40308);
#7875=VERTEX_POINT('',#40317);
#7876=VERTEX_POINT('',#40319);
#7877=VERTEX_POINT('',#40328);
#7878=VERTEX_POINT('',#40330);
#7879=VERTEX_POINT('',#40342);
#7880=VERTEX_POINT('',#40344);
#7881=VERTEX_POINT('',#40353);
#7882=VERTEX_POINT('',#40355);
#7883=VERTEX_POINT('',#40364);
#7884=VERTEX_POINT('',#40366);
#7885=VERTEX_POINT('',#40375);
#7886=VERTEX_POINT('',#40377);
#7887=VERTEX_POINT('',#40386);
#7888=VERTEX_POINT('',#40388);
#7889=VERTEX_POINT('',#40397);
#7890=VERTEX_POINT('',#40399);
#7891=VERTEX_POINT('',#40408);
#7892=VERTEX_POINT('',#40410);
#7893=VERTEX_POINT('',#40419);
#7894=VERTEX_POINT('',#40421);
#7895=VERTEX_POINT('',#40430);
#7896=VERTEX_POINT('',#40432);
#7897=VERTEX_POINT('',#40441);
#7898=VERTEX_POINT('',#40443);
#7899=VERTEX_POINT('',#40452);
#7900=VERTEX_POINT('',#40454);
#7901=VERTEX_POINT('',#40463);
#7902=VERTEX_POINT('',#40470);
#7903=VERTEX_POINT('',#40472);
#7904=VERTEX_POINT('',#40481);
#7905=VERTEX_POINT('',#40483);
#7906=VERTEX_POINT('',#40492);
#7907=VERTEX_POINT('',#40494);
#7908=VERTEX_POINT('',#40503);
#7909=VERTEX_POINT('',#40505);
#7910=VERTEX_POINT('',#40514);
#7911=VERTEX_POINT('',#40516);
#7912=VERTEX_POINT('',#40525);
#7913=VERTEX_POINT('',#40527);
#7914=VERTEX_POINT('',#40536);
#7915=VERTEX_POINT('',#40543);
#7916=VERTEX_POINT('',#40550);
#7917=VERTEX_POINT('',#40552);
#7918=VERTEX_POINT('',#40554);
#7919=VERTEX_POINT('',#40558);
#7920=VERTEX_POINT('',#40562);
#7921=VERTEX_POINT('',#40565);
#7922=VERTEX_POINT('',#40569);
#7923=VERTEX_POINT('',#40572);
#7924=VERTEX_POINT('',#40576);
#7925=VERTEX_POINT('',#40580);
#7926=VERTEX_POINT('',#40587);
#7927=VERTEX_POINT('',#40589);
#7928=VERTEX_POINT('',#40591);
#7929=VERTEX_POINT('',#40595);
#7930=VERTEX_POINT('',#40597);
#7931=VERTEX_POINT('',#40602);
#7932=VERTEX_POINT('',#40604);
#7933=VERTEX_POINT('',#40608);
#7934=VERTEX_POINT('',#40610);
#7935=VERTEX_POINT('',#40614);
#7936=VERTEX_POINT('',#40616);
#7937=VERTEX_POINT('',#40620);
#7938=VERTEX_POINT('',#40624);
#7939=VERTEX_POINT('',#40626);
#7940=VERTEX_POINT('',#40630);
#7941=VERTEX_POINT('',#40635);
#7942=VERTEX_POINT('',#40641);
#7943=VERTEX_POINT('',#40642);
#7944=VERTEX_POINT('',#40644);
#7945=VERTEX_POINT('',#40655);
#7946=VERTEX_POINT('',#40668);
#7947=VERTEX_POINT('',#40669);
#7948=VERTEX_POINT('',#40716);
#7949=VERTEX_POINT('',#40717);
#7950=VERTEX_POINT('',#40764);
#7951=VERTEX_POINT('',#40765);
#7952=VERTEX_POINT('',#40812);
#7953=VERTEX_POINT('',#40813);
#7954=VERTEX_POINT('',#40866);
#7955=VERTEX_POINT('',#40867);
#7956=VERTEX_POINT('',#40914);
#7957=VERTEX_POINT('',#40915);
#7958=VERTEX_POINT('',#40962);
#7959=VERTEX_POINT('',#40963);
#7960=VERTEX_POINT('',#41016);
#7961=VERTEX_POINT('',#41017);
#7962=VERTEX_POINT('',#41064);
#7963=VERTEX_POINT('',#41065);
#7964=VERTEX_POINT('',#41112);
#7965=VERTEX_POINT('',#41113);
#7966=VERTEX_POINT('',#41160);
#7967=VERTEX_POINT('',#41161);
#7968=VERTEX_POINT('',#41214);
#7969=VERTEX_POINT('',#41215);
#7970=VERTEX_POINT('',#41262);
#7971=VERTEX_POINT('',#41263);
#7972=VERTEX_POINT('',#41265);
#7973=VERTEX_POINT('',#41275);
#7974=VERTEX_POINT('',#41287);
#7975=VERTEX_POINT('',#41288);
#7976=VERTEX_POINT('',#41312);
#7977=VERTEX_POINT('',#41313);
#7978=VERTEX_POINT('',#41337);
#7979=VERTEX_POINT('',#41338);
#7980=VERTEX_POINT('',#41361);
#7981=VERTEX_POINT('',#41362);
#7982=VERTEX_POINT('',#41385);
#7983=VERTEX_POINT('',#41386);
#7984=VERTEX_POINT('',#41410);
#7985=VERTEX_POINT('',#41411);
#7986=VERTEX_POINT('',#41435);
#7987=VERTEX_POINT('',#41436);
#7988=VERTEX_POINT('',#41459);
#7989=VERTEX_POINT('',#41460);
#7990=VERTEX_POINT('',#41484);
#7991=VERTEX_POINT('',#41485);
#7992=VERTEX_POINT('',#41509);
#7993=VERTEX_POINT('',#41510);
#7994=VERTEX_POINT('',#41533);
#7995=VERTEX_POINT('',#41534);
#7996=VERTEX_POINT('',#41900);
#7997=VERTEX_POINT('',#42017);
#7998=VERTEX_POINT('',#42134);
#7999=VERTEX_POINT('',#42137);
#8000=VERTEX_POINT('',#42605);
#8001=VERTEX_POINT('',#42727);
#8002=VERTEX_POINT('',#42735);
#8003=VERTEX_POINT('',#42736);
#8004=VERTEX_POINT('',#42740);
#8005=VERTEX_POINT('',#42742);
#8006=VERTEX_POINT('',#42753);
#8007=VERTEX_POINT('',#42757);
#8008=VERTEX_POINT('',#42768);
#8009=VERTEX_POINT('',#42772);
#8010=VERTEX_POINT('',#42783);
#8011=VERTEX_POINT('',#42787);
#8012=VERTEX_POINT('',#42798);
#8013=VERTEX_POINT('',#42802);
#8014=VERTEX_POINT('',#42813);
#8015=VERTEX_POINT('',#42817);
#8016=VERTEX_POINT('',#42828);
#8017=VERTEX_POINT('',#42832);
#8018=VERTEX_POINT('',#42843);
#8019=VERTEX_POINT('',#42847);
#8020=VERTEX_POINT('',#42858);
#8021=VERTEX_POINT('',#42862);
#8022=VERTEX_POINT('',#42873);
#8023=VERTEX_POINT('',#42877);
#8024=VERTEX_POINT('',#42896);
#8025=VERTEX_POINT('',#42897);
#8026=VERTEX_POINT('',#42899);
#8027=VERTEX_POINT('',#42901);
#8028=VERTEX_POINT('',#42905);
#8029=VERTEX_POINT('',#42907);
#8030=VERTEX_POINT('',#42911);
#8031=VERTEX_POINT('',#42913);
#8032=VERTEX_POINT('',#42917);
#8033=VERTEX_POINT('',#42919);
#8034=VERTEX_POINT('',#42923);
#8035=VERTEX_POINT('',#42925);
#8036=VERTEX_POINT('',#42929);
#8037=VERTEX_POINT('',#42931);
#8038=VERTEX_POINT('',#42935);
#8039=VERTEX_POINT('',#42937);
#8040=VERTEX_POINT('',#42941);
#8041=VERTEX_POINT('',#42943);
#8042=VERTEX_POINT('',#42947);
#8043=VERTEX_POINT('',#42949);
#8044=VERTEX_POINT('',#42962);
#8045=VERTEX_POINT('',#42963);
#8046=VERTEX_POINT('',#42967);
#8047=VERTEX_POINT('',#42969);
#8048=VERTEX_POINT('',#42980);
#8049=VERTEX_POINT('',#42984);
#8050=VERTEX_POINT('',#42995);
#8051=VERTEX_POINT('',#42999);
#8052=VERTEX_POINT('',#43010);
#8053=VERTEX_POINT('',#43014);
#8054=VERTEX_POINT('',#43025);
#8055=VERTEX_POINT('',#43029);
#8056=VERTEX_POINT('',#43040);
#8057=VERTEX_POINT('',#43044);
#8058=VERTEX_POINT('',#43055);
#8059=VERTEX_POINT('',#43059);
#8060=VERTEX_POINT('',#43070);
#8061=VERTEX_POINT('',#43074);
#8062=VERTEX_POINT('',#43085);
#8063=VERTEX_POINT('',#43089);
#8064=VERTEX_POINT('',#43100);
#8065=VERTEX_POINT('',#43104);
#8066=VERTEX_POINT('',#43123);
#8067=VERTEX_POINT('',#43124);
#8068=VERTEX_POINT('',#43126);
#8069=VERTEX_POINT('',#43128);
#8070=VERTEX_POINT('',#43132);
#8071=VERTEX_POINT('',#43134);
#8072=VERTEX_POINT('',#43138);
#8073=VERTEX_POINT('',#43140);
#8074=VERTEX_POINT('',#43144);
#8075=VERTEX_POINT('',#43146);
#8076=VERTEX_POINT('',#43150);
#8077=VERTEX_POINT('',#43152);
#8078=VERTEX_POINT('',#43156);
#8079=VERTEX_POINT('',#43158);
#8080=VERTEX_POINT('',#43162);
#8081=VERTEX_POINT('',#43164);
#8082=VERTEX_POINT('',#43168);
#8083=VERTEX_POINT('',#43170);
#8084=VERTEX_POINT('',#43174);
#8085=VERTEX_POINT('',#43176);
#8086=VERTEX_POINT('',#43184);
#8087=VERTEX_POINT('',#43185);
#8088=VERTEX_POINT('',#43187);
#8089=VERTEX_POINT('',#43189);
#8090=VERTEX_POINT('',#43193);
#8091=VERTEX_POINT('',#43195);
#8092=VERTEX_POINT('',#43199);
#8093=VERTEX_POINT('',#43201);
#8094=VERTEX_POINT('',#43205);
#8095=VERTEX_POINT('',#43207);
#8096=VERTEX_POINT('',#43211);
#8097=VERTEX_POINT('',#43213);
#8098=VERTEX_POINT('',#43217);
#8099=VERTEX_POINT('',#43219);
#8100=VERTEX_POINT('',#43223);
#8101=VERTEX_POINT('',#43225);
#8102=VERTEX_POINT('',#43229);
#8103=VERTEX_POINT('',#43231);
#8104=VERTEX_POINT('',#43235);
#8105=VERTEX_POINT('',#43237);
#8106=VERTEX_POINT('',#43245);
#8107=VERTEX_POINT('',#43247);
#8108=VERTEX_POINT('',#43250);
#8109=VERTEX_POINT('',#43254);
#8110=VERTEX_POINT('',#43259);
#8111=VERTEX_POINT('',#43260);
#8112=VERTEX_POINT('',#43262);
#8113=VERTEX_POINT('',#43264);
#8114=VERTEX_POINT('',#43268);
#8115=VERTEX_POINT('',#43272);
#8116=VERTEX_POINT('',#43278);
#8117=VERTEX_POINT('',#43279);
#8118=VERTEX_POINT('',#43281);
#8119=VERTEX_POINT('',#43283);
#8120=VERTEX_POINT('',#43287);
#8121=VERTEX_POINT('',#43291);
#8122=VERTEX_POINT('',#43297);
#8123=VERTEX_POINT('',#43298);
#8124=VERTEX_POINT('',#43300);
#8125=VERTEX_POINT('',#43302);
#8126=VERTEX_POINT('',#43306);
#8127=VERTEX_POINT('',#43310);
#8128=VERTEX_POINT('',#43316);
#8129=VERTEX_POINT('',#43317);
#8130=VERTEX_POINT('',#43319);
#8131=VERTEX_POINT('',#43321);
#8132=VERTEX_POINT('',#43325);
#8133=VERTEX_POINT('',#43329);
#8134=VERTEX_POINT('',#43335);
#8135=VERTEX_POINT('',#43336);
#8136=VERTEX_POINT('',#43338);
#8137=VERTEX_POINT('',#43340);
#8138=VERTEX_POINT('',#43344);
#8139=VERTEX_POINT('',#43348);
#8140=VERTEX_POINT('',#43354);
#8141=VERTEX_POINT('',#43355);
#8142=VERTEX_POINT('',#43357);
#8143=VERTEX_POINT('',#43359);
#8144=VERTEX_POINT('',#43363);
#8145=VERTEX_POINT('',#43367);
#8146=VERTEX_POINT('',#43373);
#8147=VERTEX_POINT('',#43374);
#8148=VERTEX_POINT('',#43376);
#8149=VERTEX_POINT('',#43378);
#8150=VERTEX_POINT('',#43382);
#8151=VERTEX_POINT('',#43386);
#8152=VERTEX_POINT('',#43392);
#8153=VERTEX_POINT('',#43393);
#8154=VERTEX_POINT('',#43395);
#8155=VERTEX_POINT('',#43397);
#8156=VERTEX_POINT('',#43401);
#8157=VERTEX_POINT('',#43405);
#8158=VERTEX_POINT('',#43411);
#8159=VERTEX_POINT('',#43412);
#8160=VERTEX_POINT('',#43414);
#8161=VERTEX_POINT('',#43416);
#8162=VERTEX_POINT('',#43420);
#8163=VERTEX_POINT('',#43424);
#8164=VERTEX_POINT('',#43430);
#8165=VERTEX_POINT('',#43431);
#8166=VERTEX_POINT('',#43433);
#8167=VERTEX_POINT('',#43435);
#8168=VERTEX_POINT('',#43439);
#8169=VERTEX_POINT('',#43443);
#8170=VERTEX_POINT('',#43449);
#8171=VERTEX_POINT('',#43450);
#8172=VERTEX_POINT('',#43452);
#8173=VERTEX_POINT('',#43454);
#8174=VERTEX_POINT('',#43458);
#8175=VERTEX_POINT('',#43462);
#8176=VERTEX_POINT('',#43468);
#8177=VERTEX_POINT('',#43469);
#8178=VERTEX_POINT('',#43471);
#8179=VERTEX_POINT('',#43473);
#8180=VERTEX_POINT('',#43477);
#8181=VERTEX_POINT('',#43481);
#8182=VERTEX_POINT('',#43487);
#8183=VERTEX_POINT('',#43488);
#8184=VERTEX_POINT('',#43490);
#8185=VERTEX_POINT('',#43492);
#8186=VERTEX_POINT('',#43496);
#8187=VERTEX_POINT('',#43500);
#8188=VERTEX_POINT('',#43506);
#8189=VERTEX_POINT('',#43507);
#8190=VERTEX_POINT('',#43509);
#8191=VERTEX_POINT('',#43511);
#8192=VERTEX_POINT('',#43515);
#8193=VERTEX_POINT('',#43519);
#8194=VERTEX_POINT('',#43525);
#8195=VERTEX_POINT('',#43526);
#8196=VERTEX_POINT('',#43528);
#8197=VERTEX_POINT('',#43530);
#8198=VERTEX_POINT('',#43534);
#8199=VERTEX_POINT('',#43536);
#8200=VERTEX_POINT('',#43540);
#8201=VERTEX_POINT('',#43544);
#8202=VERTEX_POINT('',#43548);
#8203=VERTEX_POINT('',#43549);
#8204=VERTEX_POINT('',#43551);
#8205=VERTEX_POINT('',#43553);
#8206=VERTEX_POINT('',#43557);
#8207=VERTEX_POINT('',#43561);
#8208=VERTEX_POINT('',#43567);
#8209=VERTEX_POINT('',#43568);
#8210=VERTEX_POINT('',#43570);
#8211=VERTEX_POINT('',#43572);
#8212=VERTEX_POINT('',#43576);
#8213=VERTEX_POINT('',#43580);
#8214=VERTEX_POINT('',#43586);
#8215=VERTEX_POINT('',#43587);
#8216=VERTEX_POINT('',#43589);
#8217=VERTEX_POINT('',#43591);
#8218=VERTEX_POINT('',#43595);
#8219=VERTEX_POINT('',#43599);
#8220=VERTEX_POINT('',#43605);
#8221=VERTEX_POINT('',#43606);
#8222=VERTEX_POINT('',#43608);
#8223=VERTEX_POINT('',#43610);
#8224=VERTEX_POINT('',#43614);
#8225=VERTEX_POINT('',#43618);
#8226=VERTEX_POINT('',#43624);
#8227=VERTEX_POINT('',#43625);
#8228=VERTEX_POINT('',#43627);
#8229=VERTEX_POINT('',#43629);
#8230=VERTEX_POINT('',#43633);
#8231=VERTEX_POINT('',#43637);
#8232=VERTEX_POINT('',#43643);
#8233=VERTEX_POINT('',#43644);
#8234=VERTEX_POINT('',#43646);
#8235=VERTEX_POINT('',#43648);
#8236=VERTEX_POINT('',#43652);
#8237=VERTEX_POINT('',#43656);
#8238=VERTEX_POINT('',#43662);
#8239=VERTEX_POINT('',#43663);
#8240=VERTEX_POINT('',#43665);
#8241=VERTEX_POINT('',#43667);
#8242=VERTEX_POINT('',#43671);
#8243=VERTEX_POINT('',#43675);
#8244=VERTEX_POINT('',#43681);
#8245=VERTEX_POINT('',#43682);
#8246=VERTEX_POINT('',#43684);
#8247=VERTEX_POINT('',#43686);
#8248=VERTEX_POINT('',#43690);
#8249=VERTEX_POINT('',#43694);
#8250=VERTEX_POINT('',#43700);
#8251=VERTEX_POINT('',#43701);
#8252=VERTEX_POINT('',#43703);
#8253=VERTEX_POINT('',#43705);
#8254=VERTEX_POINT('',#43709);
#8255=VERTEX_POINT('',#43713);
#8256=VERTEX_POINT('',#43719);
#8257=VERTEX_POINT('',#43720);
#8258=VERTEX_POINT('',#43722);
#8259=VERTEX_POINT('',#43724);
#8260=VERTEX_POINT('',#43728);
#8261=VERTEX_POINT('',#43732);
#8262=VERTEX_POINT('',#43738);
#8263=VERTEX_POINT('',#43739);
#8264=VERTEX_POINT('',#43741);
#8265=VERTEX_POINT('',#43743);
#8266=VERTEX_POINT('',#43747);
#8267=VERTEX_POINT('',#43751);
#8268=VERTEX_POINT('',#43757);
#8269=VERTEX_POINT('',#43758);
#8270=VERTEX_POINT('',#43760);
#8271=VERTEX_POINT('',#43762);
#8272=VERTEX_POINT('',#43766);
#8273=VERTEX_POINT('',#43770);
#8274=VERTEX_POINT('',#43776);
#8275=VERTEX_POINT('',#43777);
#8276=VERTEX_POINT('',#43779);
#8277=VERTEX_POINT('',#43781);
#8278=VERTEX_POINT('',#43785);
#8279=VERTEX_POINT('',#43789);
#8280=VERTEX_POINT('',#43795);
#8281=VERTEX_POINT('',#43796);
#8282=VERTEX_POINT('',#43798);
#8283=VERTEX_POINT('',#43800);
#8284=VERTEX_POINT('',#43804);
#8285=VERTEX_POINT('',#43808);
#8286=VERTEX_POINT('',#43814);
#8287=VERTEX_POINT('',#43815);
#8288=VERTEX_POINT('',#43817);
#8289=VERTEX_POINT('',#43819);
#8290=VERTEX_POINT('',#43823);
#8291=VERTEX_POINT('',#43827);
#8292=VERTEX_POINT('',#43833);
#8293=VERTEX_POINT('',#43836);
#8294=VERTEX_POINT('',#43843);
#8295=VERTEX_POINT('',#43847);
#8296=VERTEX_POINT('',#43850);
#8297=VERTEX_POINT('',#43854);
#8298=VERTEX_POINT('',#43859);
#8299=VERTEX_POINT('',#43865);
#8300=VERTEX_POINT('',#43866);
#8301=VERTEX_POINT('',#43868);
#8302=VERTEX_POINT('',#43870);
#8303=VERTEX_POINT('',#43874);
#8304=VERTEX_POINT('',#43876);
#8305=VERTEX_POINT('',#43880);
#8306=VERTEX_POINT('',#43881);
#8307=VERTEX_POINT('',#43883);
#8308=VERTEX_POINT('',#43885);
#8309=VERTEX_POINT('',#43889);
#8310=VERTEX_POINT('',#43891);
#8311=VERTEX_POINT('',#43895);
#8312=VERTEX_POINT('',#43896);
#8313=VERTEX_POINT('',#43898);
#8314=VERTEX_POINT('',#43900);
#8315=VERTEX_POINT('',#43902);
#8316=VERTEX_POINT('',#43906);
#8317=VERTEX_POINT('',#43908);
#8318=VERTEX_POINT('',#43912);
#8319=VERTEX_POINT('',#43917);
#8320=VERTEX_POINT('',#43923);
#8321=VERTEX_POINT('',#43925);
#8322=VERTEX_POINT('',#43928);
#8323=VERTEX_POINT('',#43929);
#8324=VERTEX_POINT('',#43931);
#8325=VERTEX_POINT('',#43933);
#8326=VERTEX_POINT('',#43935);
#8327=VERTEX_POINT('',#43939);
#8328=VERTEX_POINT('',#43941);
#8329=VERTEX_POINT('',#43945);
#8330=VERTEX_POINT('',#43947);
#8331=VERTEX_POINT('',#43954);
#8332=VERTEX_POINT('',#43956);
#8333=VERTEX_POINT('',#43958);
#8334=VERTEX_POINT('',#43960);
#8335=VERTEX_POINT('',#43964);
#8336=VERTEX_POINT('',#43968);
#8337=VERTEX_POINT('',#43972);
#8338=VERTEX_POINT('',#43976);
#8339=VERTEX_POINT('',#43978);
#8340=VERTEX_POINT('',#43980);
#8341=VERTEX_POINT('',#44017);
#8342=VERTEX_POINT('',#44018);
#8343=VERTEX_POINT('',#44074);
#8344=VERTEX_POINT('',#44079);
#8345=VERTEX_POINT('',#44160);
#8346=VERTEX_POINT('',#44167);
#8347=VERTEX_POINT('',#44176);
#8348=VERTEX_POINT('',#44178);
#8349=VERTEX_POINT('',#44183);
#8350=VERTEX_POINT('',#44185);
#8351=VERTEX_POINT('',#44187);
#8352=VERTEX_POINT('',#44189);
#8353=VERTEX_POINT('',#44191);
#8354=VERTEX_POINT('',#44194);
#8355=VERTEX_POINT('',#44196);
#8356=VERTEX_POINT('',#44199);
#8357=VERTEX_POINT('',#44201);
#8358=VERTEX_POINT('',#44265);
#8359=VERTEX_POINT('',#44268);
#8360=VERTEX_POINT('',#44303);
#8361=VERTEX_POINT('',#44304);
#8362=VERTEX_POINT('',#44360);
#8363=VERTEX_POINT('',#44365);
#8364=VERTEX_POINT('',#44459);
#8365=VERTEX_POINT('',#44465);
#8366=VERTEX_POINT('',#44467);
#8367=VERTEX_POINT('',#44470);
#8368=VERTEX_POINT('',#44472);
#8369=VERTEX_POINT('',#44507);
#8370=VERTEX_POINT('',#44599);
#8371=VERTEX_POINT('',#44600);
#8372=VERTEX_POINT('',#44656);
#8373=VERTEX_POINT('',#44661);
#8374=VERTEX_POINT('',#44801);
#8375=VERTEX_POINT('',#44807);
#8376=VERTEX_POINT('',#44813);
#8377=VERTEX_POINT('',#44815);
#8378=VERTEX_POINT('',#44818);
#8379=VERTEX_POINT('',#44822);
#8380=VERTEX_POINT('',#44840);
#8381=VERTEX_POINT('',#44845);
#8382=VERTEX_POINT('',#44854);
#8383=VERTEX_POINT('',#44856);
#8384=VERTEX_POINT('',#44860);
#8385=VERTEX_POINT('',#44864);
#8386=VERTEX_POINT('',#44868);
#8387=VERTEX_POINT('',#44872);
#8388=VERTEX_POINT('',#44875);
#8389=VERTEX_POINT('',#44877);
#8390=VERTEX_POINT('',#44879);
#8391=VERTEX_POINT('',#44883);
#8392=VERTEX_POINT('',#44885);
#8393=VERTEX_POINT('',#44890);
#8394=VERTEX_POINT('',#44893);
#8395=VERTEX_POINT('',#44902);
#8396=VERTEX_POINT('',#44903);
#8397=VERTEX_POINT('',#44905);
#8398=VERTEX_POINT('',#44907);
#8399=VERTEX_POINT('',#44911);
#8400=VERTEX_POINT('',#44912);
#8401=VERTEX_POINT('',#44917);
#8402=VERTEX_POINT('',#44918);
#8403=VERTEX_POINT('',#44926);
#8404=VERTEX_POINT('',#44928);
#8405=VERTEX_POINT('',#44932);
#8406=VERTEX_POINT('',#44936);
#8407=VERTEX_POINT('',#44938);
#8408=VERTEX_POINT('',#44941);
#8409=VERTEX_POINT('',#44943);
#8410=VERTEX_POINT('',#44947);
#8411=VERTEX_POINT('',#44951);
#8412=VERTEX_POINT('',#44952);
#8413=VERTEX_POINT('',#44960);
#8414=VERTEX_POINT('',#44962);
#8415=VERTEX_POINT('',#44966);
#8416=VERTEX_POINT('',#44970);
#8417=VERTEX_POINT('',#44972);
#8418=VERTEX_POINT('',#44976);
#8419=VERTEX_POINT('',#44980);
#8420=VERTEX_POINT('',#44981);
#8421=VERTEX_POINT('',#44991);
#8422=VERTEX_POINT('',#44993);
#8423=VERTEX_POINT('',#45005);
#8424=VERTEX_POINT('',#45008);
#8425=VERTEX_POINT('',#45012);
#8426=VERTEX_POINT('',#45016);
#8427=VERTEX_POINT('',#45019);
#8428=VERTEX_POINT('',#45023);
#8429=VERTEX_POINT('',#45026);
#8430=VERTEX_POINT('',#45030);
#8431=VERTEX_POINT('',#45033);
#8432=VERTEX_POINT('',#45037);
#8433=VERTEX_POINT('',#45040);
#8434=VERTEX_POINT('',#45044);
#8435=VERTEX_POINT('',#45050);
#8436=VERTEX_POINT('',#45051);
#8437=VERTEX_POINT('',#45053);
#8438=VERTEX_POINT('',#45058);
#8439=VERTEX_POINT('',#45065);
#8440=VERTEX_POINT('',#45067);
#8441=VERTEX_POINT('',#45071);
#8442=VERTEX_POINT('',#45073);
#8443=VERTEX_POINT('',#45080);
#8444=VERTEX_POINT('',#45082);
#8445=VERTEX_POINT('',#45086);
#8446=VERTEX_POINT('',#45090);
#8447=VERTEX_POINT('',#45093);
#8448=VERTEX_POINT('',#45098);
#8449=VERTEX_POINT('',#45105);
#8450=VERTEX_POINT('',#45109);
#8451=VERTEX_POINT('',#45111);
#8452=VERTEX_POINT('',#45120);
#8453=VERTEX_POINT('',#45125);
#8454=VERTEX_POINT('',#45128);
#8455=VERTEX_POINT('',#45131);
#8456=VERTEX_POINT('',#45138);
#8457=VERTEX_POINT('',#45139);
#8458=VERTEX_POINT('',#45141);
#8459=VERTEX_POINT('',#45143);
#8460=VERTEX_POINT('',#45147);
#8461=VERTEX_POINT('',#45149);
#8462=VERTEX_POINT('',#45153);
#8463=VERTEX_POINT('',#45155);
#8464=EDGE_CURVE('',#6963,#6964,#6508,.T.);
#8465=EDGE_CURVE('',#6964,#6963,#6509,.T.);
#8466=EDGE_CURVE('',#6963,#6965,#3886,.T.);
#8467=EDGE_CURVE('',#6965,#6965,#6510,.T.);
#8468=EDGE_CURVE('',#6966,#6966,#6511,.T.);
#8469=EDGE_CURVE('',#6966,#6964,#3887,.T.);
#8470=EDGE_CURVE('',#6967,#6967,#6512,.T.);
#8471=EDGE_CURVE('',#6968,#6968,#6513,.T.);
#8472=EDGE_CURVE('',#6968,#6966,#3888,.T.);
#8473=EDGE_CURVE('',#6969,#6970,#6514,.T.);
#8474=EDGE_CURVE('',#6971,#6969,#3889,.T.);
#8475=EDGE_CURVE('',#6972,#6971,#3890,.T.);
#8476=EDGE_CURVE('',#6973,#6972,#3891,.T.);
#8477=EDGE_CURVE('',#6974,#6973,#6515,.T.);
#8478=EDGE_CURVE('',#6975,#6974,#3892,.T.);
#8479=EDGE_CURVE('',#6976,#6975,#3893,.T.);
#8480=EDGE_CURVE('',#6977,#6976,#6516,.T.);
#8481=EDGE_CURVE('',#6978,#6977,#3894,.T.);
#8482=EDGE_CURVE('',#6970,#6978,#3895,.T.);
#8483=EDGE_CURVE('',#6979,#6980,#256,.T.);
#8484=EDGE_CURVE('',#6981,#6980,#257,.T.);
#8485=EDGE_CURVE('',#6981,#6982,#258,.T.);
#8486=EDGE_CURVE('',#6982,#6979,#3896,.T.);
#8487=EDGE_CURVE('',#6980,#6983,#259,.T.);
#8488=EDGE_CURVE('',#6983,#6984,#3897,.T.);
#8489=EDGE_CURVE('',#6984,#6981,#260,.T.);
#8490=EDGE_CURVE('',#6985,#6986,#246,.F.);
#8491=EDGE_CURVE('',#6986,#6984,#3898,.T.);
#8492=EDGE_CURVE('',#6983,#6985,#3899,.T.);
#8493=EDGE_CURVE('',#6987,#6982,#3900,.T.);
#8494=EDGE_CURVE('',#6988,#6987,#3901,.T.);
#8495=EDGE_CURVE('',#6989,#6988,#3902,.T.);
#8496=EDGE_CURVE('',#6990,#6989,#3903,.T.);
#8497=EDGE_CURVE('',#6991,#6990,#3904,.T.);
#8498=EDGE_CURVE('',#6992,#6991,#3905,.T.);
#8499=EDGE_CURVE('',#6993,#6992,#3906,.T.);
#8500=EDGE_CURVE('',#6994,#6993,#6517,.T.);
#8501=EDGE_CURVE('',#6995,#6994,#3907,.T.);
#8502=EDGE_CURVE('',#6996,#6995,#6518,.T.);
#8503=EDGE_CURVE('',#6997,#6996,#3908,.T.);
#8504=EDGE_CURVE('',#6997,#6998,#3909,.T.);
#8505=EDGE_CURVE('',#6979,#6998,#3910,.T.);
#8506=EDGE_CURVE('',#6984,#6999,#3911,.T.);
#8507=EDGE_CURVE('',#6987,#6999,#6519,.T.);
#8508=EDGE_CURVE('',#6986,#7000,#247,.T.);
#8509=EDGE_CURVE('',#7001,#7000,#3912,.T.);
#8510=EDGE_CURVE('',#7002,#7001,#3913,.T.);
#8511=EDGE_CURVE('',#6999,#7002,#3914,.T.);
#8512=EDGE_CURVE('',#7003,#7004,#261,.T.);
#8513=EDGE_CURVE('',#7005,#7004,#262,.T.);
#8514=EDGE_CURVE('',#7005,#7006,#263,.T.);
#8515=EDGE_CURVE('',#7006,#7003,#3915,.T.);
#8516=EDGE_CURVE('',#7007,#7008,#264,.T.);
#8517=EDGE_CURVE('',#7009,#7008,#265,.T.);
#8518=EDGE_CURVE('',#7009,#7010,#266,.T.);
#8519=EDGE_CURVE('',#7010,#7007,#3916,.T.);
#8520=EDGE_CURVE('',#7008,#7011,#267,.T.);
#8521=EDGE_CURVE('',#7011,#7012,#3917,.T.);
#8522=EDGE_CURVE('',#7012,#7009,#268,.T.);
#8523=EDGE_CURVE('',#7013,#7014,#3918,.T.);
#8524=EDGE_CURVE('',#7014,#7015,#269,.T.);
#8525=EDGE_CURVE('',#7015,#7016,#3919,.T.);
#8526=EDGE_CURVE('',#7016,#7013,#270,.T.);
#8527=EDGE_CURVE('',#7015,#7012,#271,.T.);
#8528=EDGE_CURVE('',#7011,#7016,#272,.T.);
#8529=EDGE_CURVE('',#7017,#7018,#3920,.T.);
#8530=EDGE_CURVE('',#7018,#7019,#3921,.T.);
#8531=EDGE_CURVE('',#7019,#7020,#3922,.T.);
#8532=EDGE_CURVE('',#7020,#7017,#3923,.T.);
#8533=EDGE_CURVE('',#7017,#7014,#273,.T.);
#8534=EDGE_CURVE('',#7013,#7018,#274,.T.);
#8535=EDGE_CURVE('',#7021,#7022,#3924,.T.);
#8536=EDGE_CURVE('',#7022,#7023,#275,.T.);
#8537=EDGE_CURVE('',#7023,#7024,#3925,.T.);
#8538=EDGE_CURVE('',#7024,#7021,#276,.T.);
#8539=EDGE_CURVE('',#7021,#7020,#277,.T.);
#8540=EDGE_CURVE('',#7019,#7022,#278,.T.);
#8541=EDGE_CURVE('',#7004,#7025,#279,.T.);
#8542=EDGE_CURVE('',#7025,#7026,#3926,.T.);
#8543=EDGE_CURVE('',#7026,#7005,#280,.T.);
#8544=EDGE_CURVE('',#7025,#7024,#281,.T.);
#8545=EDGE_CURVE('',#7023,#7026,#282,.T.);
#8546=EDGE_CURVE('',#7007,#7027,#3927,.T.);
#8547=EDGE_CURVE('',#7027,#7028,#6520,.F.);
#8548=EDGE_CURVE('',#7028,#7013,#3928,.T.);
#8549=EDGE_CURVE('',#7029,#7010,#3929,.T.);
#8550=EDGE_CURVE('',#7030,#7029,#3930,.T.);
#8551=EDGE_CURVE('',#7027,#7030,#3931,.T.);
#8552=EDGE_CURVE('',#7012,#7031,#3932,.T.);
#8553=EDGE_CURVE('',#7031,#7029,#6521,.T.);
#8554=EDGE_CURVE('',#7032,#7025,#3933,.T.);
#8555=EDGE_CURVE('',#7031,#7032,#3934,.T.);
#8556=EDGE_CURVE('',#7033,#7034,#6522,.T.);
#8557=EDGE_CURVE('',#7034,#7035,#3935,.T.);
#8558=EDGE_CURVE('',#7035,#7036,#6523,.T.);
#8559=EDGE_CURVE('',#7036,#7033,#3936,.T.);
#8560=EDGE_CURVE('',#7035,#7037,#6524,.T.);
#8561=EDGE_CURVE('',#7037,#7036,#6525,.T.);
#8562=EDGE_CURVE('',#7033,#6978,#6526,.T.);
#8563=EDGE_CURVE('',#6978,#7034,#6527,.T.);
#8564=EDGE_CURVE('',#7037,#7038,#3937,.T.);
#8565=EDGE_CURVE('',#7038,#7039,#283,.F.);
#8566=EDGE_CURVE('',#7039,#7036,#3938,.T.);
#8567=EDGE_CURVE('',#7035,#7040,#3939,.T.);
#8568=EDGE_CURVE('',#7040,#7041,#284,.F.);
#8569=EDGE_CURVE('',#7041,#7037,#3940,.T.);
#8570=EDGE_CURVE('',#7042,#7034,#3941,.T.);
#8571=EDGE_CURVE('',#7042,#7040,#3942,.T.);
#8572=EDGE_CURVE('',#7001,#7043,#6528,.F.);
#8573=EDGE_CURVE('',#7044,#7001,#6529,.F.);
#8574=EDGE_CURVE('',#7043,#7044,#6530,.F.);
#8575=EDGE_CURVE('',#7000,#7045,#285,.F.);
#8576=EDGE_CURVE('',#7045,#7044,#3943,.T.);
#8577=EDGE_CURVE('',#7046,#7047,#286,.F.);
#8578=EDGE_CURVE('',#7047,#7043,#3944,.T.);
#8579=EDGE_CURVE('',#7044,#7046,#3945,.T.);
#8580=EDGE_CURVE('',#7048,#7049,#6531,.F.);
#8581=EDGE_CURVE('',#7002,#7048,#6532,.F.);
#8582=EDGE_CURVE('',#7049,#7002,#6533,.F.);
#8583=EDGE_CURVE('',#6999,#7050,#6534,.T.);
#8584=EDGE_CURVE('',#7050,#6987,#6535,.T.);
#8585=EDGE_CURVE('',#7048,#7050,#3946,.T.);
#8586=EDGE_CURVE('',#7043,#7049,#3947,.T.);
#8587=EDGE_CURVE('',#7051,#7052,#6536,.F.);
#8588=EDGE_CURVE('',#7053,#7051,#6537,.F.);
#8589=EDGE_CURVE('',#7052,#7053,#6538,.F.);
#8590=EDGE_CURVE('',#7054,#7055,#6539,.T.);
#8591=EDGE_CURVE('',#7055,#6988,#6540,.T.);
#8592=EDGE_CURVE('',#6988,#7054,#6541,.T.);
#8593=EDGE_CURVE('',#7054,#7053,#3948,.T.);
#8594=EDGE_CURVE('',#7051,#7055,#3949,.T.);
#8595=EDGE_CURVE('',#7049,#7052,#3950,.T.);
#8596=EDGE_CURVE('',#7053,#7048,#3951,.T.);
#8597=EDGE_CURVE('',#7056,#7027,#6542,.F.);
#8598=EDGE_CURVE('',#7028,#7056,#6543,.F.);
#8599=EDGE_CURVE('',#7057,#7030,#6544,.T.);
#8600=EDGE_CURVE('',#7030,#6989,#6545,.T.);
#8601=EDGE_CURVE('',#6989,#7057,#6546,.T.);
#8602=EDGE_CURVE('',#7057,#7056,#3952,.T.);
#8603=EDGE_CURVE('',#7052,#7028,#3953,.T.);
#8604=EDGE_CURVE('',#7056,#7051,#3954,.T.);
#8605=EDGE_CURVE('',#7058,#7032,#6547,.F.);
#8606=EDGE_CURVE('',#6991,#7058,#6548,.F.);
#8607=EDGE_CURVE('',#7032,#6991,#6549,.F.);
#8608=EDGE_CURVE('',#7059,#6992,#6550,.T.);
#8609=EDGE_CURVE('',#7058,#7059,#3955,.T.);
#8610=EDGE_CURVE('',#7059,#7060,#6551,.T.);
#8611=EDGE_CURVE('',#7060,#6992,#6552,.T.);
#8612=EDGE_CURVE('',#6990,#7031,#6553,.T.);
#8613=EDGE_CURVE('',#7003,#7058,#3956,.T.);
#8614=EDGE_CURVE('',#7061,#7062,#6554,.T.);
#8615=EDGE_CURVE('',#7062,#7063,#6555,.T.);
#8616=EDGE_CURVE('',#7063,#7061,#6556,.T.);
#8617=EDGE_CURVE('',#7022,#7062,#3957,.T.);
#8618=EDGE_CURVE('',#7061,#7006,#3958,.T.);
#8619=EDGE_CURVE('',#6990,#7029,#6557,.T.);
#8620=EDGE_CURVE('',#7050,#7054,#3959,.T.);
#8621=EDGE_CURVE('',#7064,#7065,#287,.T.);
#8622=EDGE_CURVE('',#7065,#7066,#288,.T.);
#8623=EDGE_CURVE('',#7066,#7067,#289,.T.);
#8624=EDGE_CURVE('',#7067,#7068,#290,.T.);
#8625=EDGE_CURVE('',#7068,#7069,#291,.T.);
#8626=EDGE_CURVE('',#7069,#7070,#292,.T.);
#8627=EDGE_CURVE('',#7070,#7071,#293,.T.);
#8628=EDGE_CURVE('',#7071,#7072,#294,.T.);
#8629=EDGE_CURVE('',#7072,#7073,#295,.T.);
#8630=EDGE_CURVE('',#7073,#7074,#296,.T.);
#8631=EDGE_CURVE('',#7074,#7064,#297,.T.);
#8632=EDGE_CURVE('',#7075,#7076,#3960,.T.);
#8633=EDGE_CURVE('',#7076,#7077,#3961,.T.);
#8634=EDGE_CURVE('',#7077,#7078,#3962,.T.);
#8635=EDGE_CURVE('',#7078,#7079,#3963,.T.);
#8636=EDGE_CURVE('',#7079,#7080,#3964,.T.);
#8637=EDGE_CURVE('',#7080,#7081,#3965,.T.);
#8638=EDGE_CURVE('',#7081,#7082,#3966,.T.);
#8639=EDGE_CURVE('',#7082,#7075,#3967,.T.);
#8640=EDGE_CURVE('',#7083,#7084,#298,.T.);
#8641=EDGE_CURVE('',#7084,#7085,#299,.T.);
#8642=EDGE_CURVE('',#7085,#7086,#300,.T.);
#8643=EDGE_CURVE('',#7086,#7087,#301,.T.);
#8644=EDGE_CURVE('',#7087,#7088,#302,.T.);
#8645=EDGE_CURVE('',#7088,#7089,#303,.T.);
#8646=EDGE_CURVE('',#7089,#7090,#304,.T.);
#8647=EDGE_CURVE('',#7090,#7091,#305,.T.);
#8648=EDGE_CURVE('',#7091,#7092,#306,.T.);
#8649=EDGE_CURVE('',#7092,#7093,#307,.T.);
#8650=EDGE_CURVE('',#7093,#7094,#308,.T.);
#8651=EDGE_CURVE('',#7094,#7095,#309,.T.);
#8652=EDGE_CURVE('',#7095,#7096,#310,.T.);
#8653=EDGE_CURVE('',#7096,#7097,#311,.T.);
#8654=EDGE_CURVE('',#7097,#7098,#312,.T.);
#8655=EDGE_CURVE('',#7098,#7083,#313,.T.);
#8656=EDGE_CURVE('',#7099,#7100,#3968,.T.);
#8657=EDGE_CURVE('',#7100,#7101,#3969,.T.);
#8658=EDGE_CURVE('',#7101,#7102,#3970,.T.);
#8659=EDGE_CURVE('',#7102,#7103,#3971,.T.);
#8660=EDGE_CURVE('',#7103,#7104,#3972,.T.);
#8661=EDGE_CURVE('',#7104,#7105,#3973,.T.);
#8662=EDGE_CURVE('',#7105,#7106,#3974,.T.);
#8663=EDGE_CURVE('',#7106,#7107,#3975,.T.);
#8664=EDGE_CURVE('',#7107,#7108,#3976,.T.);
#8665=EDGE_CURVE('',#7108,#7099,#3977,.T.);
#8666=EDGE_CURVE('',#7055,#7057,#3978,.T.);
#8667=EDGE_CURVE('',#7060,#7109,#3979,.T.);
#8668=EDGE_CURVE('',#6993,#7109,#6558,.T.);
#8669=EDGE_CURVE('',#7059,#7061,#3980,.T.);
#8670=EDGE_CURVE('',#7063,#7060,#3981,.T.);
#8671=EDGE_CURVE('',#7062,#7110,#3982,.T.);
#8672=EDGE_CURVE('',#7111,#7110,#6559,.T.);
#8673=EDGE_CURVE('',#7111,#7063,#3983,.T.);
#8674=EDGE_CURVE('',#6998,#7112,#314,.F.);
#8675=EDGE_CURVE('',#7112,#6983,#3984,.T.);
#8676=EDGE_CURVE('',#7112,#6985,#6560,.T.);
#8677=EDGE_CURVE('',#7041,#7038,#6561,.T.);
#8678=EDGE_CURVE('',#7033,#7113,#3985,.T.);
#8679=EDGE_CURVE('',#7113,#6970,#315,.F.);
#8680=EDGE_CURVE('',#6977,#7042,#316,.F.);
#8681=EDGE_CURVE('',#7039,#7113,#3986,.T.);
#8682=EDGE_CURVE('',#7114,#7115,#6562,.F.);
#8683=EDGE_CURVE('',#6975,#7114,#6563,.F.);
#8684=EDGE_CURVE('',#7115,#6975,#6564,.F.);
#8685=EDGE_CURVE('',#7116,#6976,#317,.F.);
#8686=EDGE_CURVE('',#7114,#7116,#3987,.T.);
#8687=EDGE_CURVE('',#6974,#7117,#318,.F.);
#8688=EDGE_CURVE('',#7117,#7115,#3988,.T.);
#8689=EDGE_CURVE('',#7118,#7119,#6565,.T.);
#8690=EDGE_CURVE('',#7119,#7120,#6566,.T.);
#8691=EDGE_CURVE('',#7120,#7118,#6567,.T.);
#8692=EDGE_CURVE('',#7118,#7114,#3989,.T.);
#8693=EDGE_CURVE('',#7115,#7119,#3990,.T.);
#8694=EDGE_CURVE('',#7121,#7118,#3991,.T.);
#8695=EDGE_CURVE('',#7121,#7116,#3992,.T.);
#8696=EDGE_CURVE('',#7120,#7122,#3993,.T.);
#8697=EDGE_CURVE('',#7122,#7121,#319,.F.);
#8698=EDGE_CURVE('',#7119,#7123,#3994,.T.);
#8699=EDGE_CURVE('',#7123,#7124,#320,.F.);
#8700=EDGE_CURVE('',#7124,#7120,#3995,.T.);
#8701=EDGE_CURVE('',#7124,#7122,#6568,.T.);
#8702=EDGE_CURVE('',#7125,#7125,#6569,.T.);
#8703=EDGE_CURVE('',#7125,#7126,#6570,.T.);
#8704=EDGE_CURVE('',#7126,#7127,#6571,.T.);
#8705=EDGE_CURVE('',#7127,#7126,#6572,.T.);
#8706=EDGE_CURVE('',#7127,#7128,#3996,.T.);
#8707=EDGE_CURVE('',#7129,#7128,#6573,.T.);
#8708=EDGE_CURVE('',#7128,#7129,#6574,.T.);
#8709=EDGE_CURVE('',#7130,#7130,#6575,.T.);
#8710=EDGE_CURVE('',#7129,#7131,#6576,.T.);
#8711=EDGE_CURVE('',#7131,#7132,#6577,.T.);
#8712=EDGE_CURVE('',#7132,#7131,#6578,.T.);
#8713=EDGE_CURVE('',#7132,#7133,#3997,.T.);
#8714=EDGE_CURVE('',#7113,#7133,#6579,.T.);
#8715=EDGE_CURVE('',#7116,#7042,#6580,.T.);
#8716=EDGE_CURVE('',#7117,#7123,#3998,.T.);
#8717=EDGE_CURVE('',#7134,#7117,#6581,.T.);
#8718=EDGE_CURVE('',#7047,#7134,#3999,.T.);
#8719=EDGE_CURVE('',#7045,#7046,#6582,.T.);
#8720=EDGE_CURVE('',#7133,#6997,#6583,.T.);
#8721=EDGE_CURVE('',#7135,#7136,#6584,.T.);
#8722=EDGE_CURVE('',#7136,#7137,#4000,.T.);
#8723=EDGE_CURVE('',#7137,#7138,#6585,.T.);
#8724=EDGE_CURVE('',#7138,#7135,#4001,.T.);
#8725=EDGE_CURVE('',#7110,#7138,#6586,.T.);
#8726=EDGE_CURVE('',#7137,#7111,#6587,.T.);
#8727=EDGE_CURVE('',#6994,#7139,#6588,.T.);
#8728=EDGE_CURVE('',#7139,#7140,#4002,.T.);
#8729=EDGE_CURVE('',#7140,#6995,#6589,.T.);
#8730=EDGE_CURVE('',#6971,#6996,#6590,.T.);
#8731=EDGE_CURVE('',#7140,#6971,#6591,.T.);
#8732=EDGE_CURVE('',#6969,#6997,#321,.T.);
#8733=EDGE_CURVE('',#7109,#7139,#6592,.T.);
#8734=EDGE_CURVE('',#7141,#6972,#6593,.T.);
#8735=EDGE_CURVE('',#6972,#7136,#6594,.T.);
#8736=EDGE_CURVE('',#7135,#7141,#6595,.T.);
#8737=EDGE_CURVE('',#7141,#7134,#4003,.T.);
#8738=EDGE_CURVE('',#7134,#6973,#322,.T.);
#8739=EDGE_CURVE('',#7109,#7111,#4004,.T.);
#8740=EDGE_CURVE('',#7142,#7142,#6596,.T.);
#8741=EDGE_CURVE('',#7137,#7139,#4005,.T.);
#8742=EDGE_CURVE('',#7140,#7136,#4006,.T.);
#8743=EDGE_CURVE('',#7064,#7143,#4007,.T.);
#8744=EDGE_CURVE('',#7143,#7144,#323,.T.);
#8745=EDGE_CURVE('',#7065,#7144,#4008,.T.);
#8746=EDGE_CURVE('',#7074,#7145,#4009,.T.);
#8747=EDGE_CURVE('',#7145,#7143,#324,.T.);
#8748=EDGE_CURVE('',#7073,#7146,#4010,.T.);
#8749=EDGE_CURVE('',#7146,#7145,#325,.T.);
#8750=EDGE_CURVE('',#7072,#7147,#4011,.T.);
#8751=EDGE_CURVE('',#7147,#7146,#326,.T.);
#8752=EDGE_CURVE('',#7071,#7148,#4012,.T.);
#8753=EDGE_CURVE('',#7148,#7147,#327,.T.);
#8754=EDGE_CURVE('',#7070,#7149,#4013,.T.);
#8755=EDGE_CURVE('',#7149,#7148,#328,.T.);
#8756=EDGE_CURVE('',#7069,#7150,#4014,.T.);
#8757=EDGE_CURVE('',#7150,#7149,#329,.T.);
#8758=EDGE_CURVE('',#7068,#7151,#4015,.T.);
#8759=EDGE_CURVE('',#7151,#7150,#330,.T.);
#8760=EDGE_CURVE('',#7067,#7152,#4016,.T.);
#8761=EDGE_CURVE('',#7152,#7151,#331,.T.);
#8762=EDGE_CURVE('',#7066,#7153,#4017,.T.);
#8763=EDGE_CURVE('',#7153,#7152,#332,.T.);
#8764=EDGE_CURVE('',#7144,#7153,#333,.T.);
#8765=EDGE_CURVE('',#7075,#7154,#4018,.T.);
#8766=EDGE_CURVE('',#7154,#7155,#4019,.T.);
#8767=EDGE_CURVE('',#7076,#7155,#4020,.T.);
#8768=EDGE_CURVE('',#7082,#7156,#4021,.T.);
#8769=EDGE_CURVE('',#7156,#7154,#4022,.T.);
#8770=EDGE_CURVE('',#7081,#7157,#4023,.T.);
#8771=EDGE_CURVE('',#7157,#7156,#4024,.T.);
#8772=EDGE_CURVE('',#7080,#7158,#4025,.T.);
#8773=EDGE_CURVE('',#7158,#7157,#4026,.T.);
#8774=EDGE_CURVE('',#7079,#7159,#4027,.T.);
#8775=EDGE_CURVE('',#7159,#7158,#4028,.T.);
#8776=EDGE_CURVE('',#7078,#7160,#4029,.T.);
#8777=EDGE_CURVE('',#7160,#7159,#4030,.T.);
#8778=EDGE_CURVE('',#7077,#7161,#4031,.T.);
#8779=EDGE_CURVE('',#7161,#7160,#4032,.T.);
#8780=EDGE_CURVE('',#7155,#7161,#4033,.T.);
#8781=EDGE_CURVE('',#7083,#7162,#4034,.T.);
#8782=EDGE_CURVE('',#7162,#7163,#334,.T.);
#8783=EDGE_CURVE('',#7084,#7163,#4035,.T.);
#8784=EDGE_CURVE('',#7098,#7164,#4036,.T.);
#8785=EDGE_CURVE('',#7164,#7162,#335,.T.);
#8786=EDGE_CURVE('',#7097,#7165,#4037,.T.);
#8787=EDGE_CURVE('',#7165,#7164,#336,.T.);
#8788=EDGE_CURVE('',#7096,#7166,#4038,.T.);
#8789=EDGE_CURVE('',#7166,#7165,#337,.T.);
#8790=EDGE_CURVE('',#7095,#7167,#4039,.T.);
#8791=EDGE_CURVE('',#7167,#7166,#338,.T.);
#8792=EDGE_CURVE('',#7094,#7168,#4040,.T.);
#8793=EDGE_CURVE('',#7168,#7167,#339,.T.);
#8794=EDGE_CURVE('',#7093,#7169,#4041,.T.);
#8795=EDGE_CURVE('',#7169,#7168,#340,.T.);
#8796=EDGE_CURVE('',#7092,#7170,#4042,.T.);
#8797=EDGE_CURVE('',#7170,#7169,#341,.T.);
#8798=EDGE_CURVE('',#7091,#7171,#4043,.T.);
#8799=EDGE_CURVE('',#7171,#7170,#342,.T.);
#8800=EDGE_CURVE('',#7090,#7172,#4044,.T.);
#8801=EDGE_CURVE('',#7172,#7171,#343,.T.);
#8802=EDGE_CURVE('',#7089,#7173,#4045,.T.);
#8803=EDGE_CURVE('',#7173,#7172,#344,.T.);
#8804=EDGE_CURVE('',#7088,#7174,#4046,.T.);
#8805=EDGE_CURVE('',#7174,#7173,#345,.T.);
#8806=EDGE_CURVE('',#7087,#7175,#4047,.T.);
#8807=EDGE_CURVE('',#7175,#7174,#346,.T.);
#8808=EDGE_CURVE('',#7086,#7176,#4048,.T.);
#8809=EDGE_CURVE('',#7176,#7175,#347,.T.);
#8810=EDGE_CURVE('',#7085,#7177,#4049,.T.);
#8811=EDGE_CURVE('',#7177,#7176,#348,.T.);
#8812=EDGE_CURVE('',#7163,#7177,#349,.T.);
#8813=EDGE_CURVE('',#7099,#7178,#4050,.T.);
#8814=EDGE_CURVE('',#7178,#7179,#4051,.T.);
#8815=EDGE_CURVE('',#7100,#7179,#4052,.T.);
#8816=EDGE_CURVE('',#7108,#7180,#4053,.T.);
#8817=EDGE_CURVE('',#7180,#7178,#4054,.T.);
#8818=EDGE_CURVE('',#7107,#7181,#4055,.T.);
#8819=EDGE_CURVE('',#7181,#7180,#4056,.T.);
#8820=EDGE_CURVE('',#7106,#7182,#4057,.T.);
#8821=EDGE_CURVE('',#7182,#7181,#4058,.T.);
#8822=EDGE_CURVE('',#7105,#7183,#4059,.T.);
#8823=EDGE_CURVE('',#7183,#7182,#4060,.T.);
#8824=EDGE_CURVE('',#7104,#7184,#4061,.T.);
#8825=EDGE_CURVE('',#7184,#7183,#4062,.T.);
#8826=EDGE_CURVE('',#7103,#7185,#4063,.T.);
#8827=EDGE_CURVE('',#7185,#7184,#4064,.T.);
#8828=EDGE_CURVE('',#7102,#7186,#4065,.T.);
#8829=EDGE_CURVE('',#7186,#7185,#4066,.T.);
#8830=EDGE_CURVE('',#7101,#7187,#4067,.T.);
#8831=EDGE_CURVE('',#7187,#7186,#4068,.T.);
#8832=EDGE_CURVE('',#7179,#7187,#4069,.T.);
#8833=EDGE_CURVE('',#7142,#7188,#4070,.T.);
#8834=EDGE_CURVE('',#7188,#7188,#6597,.T.);
#8835=EDGE_CURVE('',#7189,#7189,#6598,.T.);
#8836=EDGE_CURVE('',#7189,#7130,#4071,.T.);
#8837=EDGE_CURVE('',#6967,#7189,#4072,.T.);
#8838=EDGE_CURVE('',#7190,#7191,#4073,.T.);
#8839=EDGE_CURVE('',#7190,#7192,#350,.T.);
#8840=EDGE_CURVE('',#7192,#7193,#6599,.T.);
#8841=EDGE_CURVE('',#7193,#7191,#351,.T.);
#8842=EDGE_CURVE('',#7194,#7195,#4074,.T.);
#8843=EDGE_CURVE('',#7194,#7190,#352,.T.);
#8844=EDGE_CURVE('',#7191,#7195,#353,.T.);
#8845=EDGE_CURVE('',#7196,#7197,#4075,.T.);
#8846=EDGE_CURVE('',#7196,#7194,#354,.T.);
#8847=EDGE_CURVE('',#7195,#7197,#355,.T.);
#8848=EDGE_CURVE('',#7198,#7199,#4076,.T.);
#8849=EDGE_CURVE('',#7198,#7196,#356,.T.);
#8850=EDGE_CURVE('',#7197,#7199,#357,.T.);
#8851=EDGE_CURVE('',#7200,#7201,#4077,.T.);
#8852=EDGE_CURVE('',#7200,#7198,#358,.T.);
#8853=EDGE_CURVE('',#7199,#7201,#359,.T.);
#8854=EDGE_CURVE('',#7202,#7203,#4078,.T.);
#8855=EDGE_CURVE('',#7202,#7200,#360,.T.);
#8856=EDGE_CURVE('',#7201,#7203,#361,.T.);
#8857=EDGE_CURVE('',#7204,#7205,#4079,.T.);
#8858=EDGE_CURVE('',#7204,#7202,#362,.T.);
#8859=EDGE_CURVE('',#7203,#7205,#363,.T.);
#8860=EDGE_CURVE('',#7206,#7207,#4080,.T.);
#8861=EDGE_CURVE('',#7206,#7204,#364,.T.);
#8862=EDGE_CURVE('',#7205,#7207,#365,.T.);
#8863=EDGE_CURVE('',#7208,#7209,#4081,.T.);
#8864=EDGE_CURVE('',#7208,#7206,#366,.T.);
#8865=EDGE_CURVE('',#7207,#7209,#367,.T.);
#8866=EDGE_CURVE('',#7210,#7211,#4082,.T.);
#8867=EDGE_CURVE('',#7210,#7208,#368,.T.);
#8868=EDGE_CURVE('',#7209,#7211,#369,.T.);
#8869=EDGE_CURVE('',#7212,#7213,#4083,.T.);
#8870=EDGE_CURVE('',#7212,#7210,#370,.T.);
#8871=EDGE_CURVE('',#7211,#7213,#371,.T.);
#8872=EDGE_CURVE('',#7214,#7215,#4084,.T.);
#8873=EDGE_CURVE('',#7214,#7212,#372,.T.);
#8874=EDGE_CURVE('',#7213,#7215,#373,.T.);
#8875=EDGE_CURVE('',#7216,#7217,#4085,.T.);
#8876=EDGE_CURVE('',#7216,#7214,#374,.T.);
#8877=EDGE_CURVE('',#7215,#7217,#375,.T.);
#8878=EDGE_CURVE('',#7218,#7219,#4086,.T.);
#8879=EDGE_CURVE('',#7218,#7216,#376,.T.);
#8880=EDGE_CURVE('',#7217,#7219,#377,.T.);
#8881=EDGE_CURVE('',#7220,#7221,#4087,.T.);
#8882=EDGE_CURVE('',#7220,#7218,#378,.T.);
#8883=EDGE_CURVE('',#7219,#7221,#379,.T.);
#8884=EDGE_CURVE('',#7222,#7223,#4088,.T.);
#8885=EDGE_CURVE('',#7222,#7220,#380,.T.);
#8886=EDGE_CURVE('',#7221,#7223,#381,.T.);
#8887=EDGE_CURVE('',#7224,#7225,#4089,.T.);
#8888=EDGE_CURVE('',#7224,#7226,#382,.T.);
#8889=EDGE_CURVE('',#7227,#7226,#6600,.T.);
#8890=EDGE_CURVE('',#7225,#7227,#383,.T.);
#8891=EDGE_CURVE('',#7228,#7229,#4090,.T.);
#8892=EDGE_CURVE('',#7228,#7224,#384,.T.);
#8893=EDGE_CURVE('',#7229,#7225,#385,.T.);
#8894=EDGE_CURVE('',#7230,#7231,#4091,.T.);
#8895=EDGE_CURVE('',#7230,#7228,#386,.T.);
#8896=EDGE_CURVE('',#7231,#7229,#387,.T.);
#8897=EDGE_CURVE('',#7232,#7233,#4092,.T.);
#8898=EDGE_CURVE('',#7232,#7230,#388,.T.);
#8899=EDGE_CURVE('',#7233,#7231,#389,.T.);
#8900=EDGE_CURVE('',#7234,#7235,#4093,.T.);
#8901=EDGE_CURVE('',#7234,#7232,#390,.T.);
#8902=EDGE_CURVE('',#7235,#7233,#391,.T.);
#8903=EDGE_CURVE('',#7236,#7237,#4094,.T.);
#8904=EDGE_CURVE('',#7236,#7234,#392,.T.);
#8905=EDGE_CURVE('',#7237,#7235,#393,.T.);
#8906=EDGE_CURVE('',#7238,#7239,#4095,.T.);
#8907=EDGE_CURVE('',#7238,#7236,#394,.T.);
#8908=EDGE_CURVE('',#7239,#7237,#395,.T.);
#8909=EDGE_CURVE('',#7240,#7241,#4096,.T.);
#8910=EDGE_CURVE('',#7240,#7238,#396,.T.);
#8911=EDGE_CURVE('',#7241,#7239,#397,.T.);
#8912=EDGE_CURVE('',#7242,#7243,#4097,.T.);
#8913=EDGE_CURVE('',#7242,#7240,#398,.T.);
#8914=EDGE_CURVE('',#7243,#7241,#399,.T.);
#8915=EDGE_CURVE('',#7244,#7245,#4098,.T.);
#8916=EDGE_CURVE('',#7244,#7242,#400,.T.);
#8917=EDGE_CURVE('',#7245,#7243,#401,.T.);
#8918=EDGE_CURVE('',#7246,#7247,#4099,.T.);
#8919=EDGE_CURVE('',#7246,#7244,#402,.T.);
#8920=EDGE_CURVE('',#7247,#7245,#403,.T.);
#8921=EDGE_CURVE('',#7248,#7249,#4100,.T.);
#8922=EDGE_CURVE('',#7248,#7246,#404,.T.);
#8923=EDGE_CURVE('',#7249,#7247,#405,.T.);
#8924=EDGE_CURVE('',#7250,#7251,#4101,.T.);
#8925=EDGE_CURVE('',#7250,#7248,#406,.T.);
#8926=EDGE_CURVE('',#7251,#7249,#407,.T.);
#8927=EDGE_CURVE('',#7252,#7253,#4102,.T.);
#8928=EDGE_CURVE('',#7252,#7250,#408,.T.);
#8929=EDGE_CURVE('',#7253,#7251,#409,.T.);
#8930=EDGE_CURVE('',#7254,#7255,#4103,.T.);
#8931=EDGE_CURVE('',#7254,#7252,#410,.T.);
#8932=EDGE_CURVE('',#7255,#7253,#411,.T.);
#8933=EDGE_CURVE('',#7256,#7257,#4104,.T.);
#8934=EDGE_CURVE('',#7256,#7258,#412,.T.);
#8935=EDGE_CURVE('',#7258,#7259,#6601,.F.);
#8936=EDGE_CURVE('',#7259,#7257,#413,.T.);
#8937=EDGE_CURVE('',#7260,#7261,#4105,.T.);
#8938=EDGE_CURVE('',#7260,#7256,#414,.T.);
#8939=EDGE_CURVE('',#7257,#7261,#415,.T.);
#8940=EDGE_CURVE('',#7262,#7263,#4106,.T.);
#8941=EDGE_CURVE('',#7262,#7260,#416,.T.);
#8942=EDGE_CURVE('',#7261,#7263,#417,.T.);
#8943=EDGE_CURVE('',#7264,#7265,#4107,.T.);
#8944=EDGE_CURVE('',#7264,#7262,#418,.T.);
#8945=EDGE_CURVE('',#7263,#7265,#419,.T.);
#8946=EDGE_CURVE('',#7266,#7267,#4108,.T.);
#8947=EDGE_CURVE('',#7266,#7264,#420,.T.);
#8948=EDGE_CURVE('',#7265,#7267,#421,.T.);
#8949=EDGE_CURVE('',#7268,#7269,#4109,.T.);
#8950=EDGE_CURVE('',#7268,#7266,#422,.T.);
#8951=EDGE_CURVE('',#7267,#7269,#423,.T.);
#8952=EDGE_CURVE('',#7270,#7271,#4110,.T.);
#8953=EDGE_CURVE('',#7270,#7268,#424,.T.);
#8954=EDGE_CURVE('',#7269,#7271,#425,.T.);
#8955=EDGE_CURVE('',#7272,#7273,#4111,.T.);
#8956=EDGE_CURVE('',#7272,#7270,#426,.T.);
#8957=EDGE_CURVE('',#7271,#7273,#427,.T.);
#8958=EDGE_CURVE('',#7274,#7275,#4112,.T.);
#8959=EDGE_CURVE('',#7274,#7272,#428,.T.);
#8960=EDGE_CURVE('',#7273,#7275,#429,.T.);
#8961=EDGE_CURVE('',#7276,#7277,#4113,.T.);
#8962=EDGE_CURVE('',#7276,#7274,#430,.T.);
#8963=EDGE_CURVE('',#7275,#7277,#431,.T.);
#8964=EDGE_CURVE('',#7278,#7279,#4114,.T.);
#8965=EDGE_CURVE('',#7280,#7278,#6602,.F.);
#8966=EDGE_CURVE('',#7280,#7276,#432,.T.);
#8967=EDGE_CURVE('',#7277,#7279,#433,.T.);
#8968=EDGE_CURVE('',#7281,#7282,#4115,.T.);
#8969=EDGE_CURVE('',#7281,#7283,#434,.T.);
#8970=EDGE_CURVE('',#7284,#7283,#6603,.T.);
#8971=EDGE_CURVE('',#7282,#7284,#435,.T.);
#8972=EDGE_CURVE('',#7285,#7286,#4116,.T.);
#8973=EDGE_CURVE('',#7285,#7281,#436,.T.);
#8974=EDGE_CURVE('',#7286,#7282,#437,.T.);
#8975=EDGE_CURVE('',#7287,#7288,#4117,.T.);
#8976=EDGE_CURVE('',#7287,#7285,#438,.T.);
#8977=EDGE_CURVE('',#7288,#7286,#439,.T.);
#8978=EDGE_CURVE('',#7289,#7290,#4118,.T.);
#8979=EDGE_CURVE('',#7289,#7287,#440,.T.);
#8980=EDGE_CURVE('',#7290,#7288,#441,.T.);
#8981=EDGE_CURVE('',#7291,#7292,#4119,.T.);
#8982=EDGE_CURVE('',#7291,#7289,#442,.T.);
#8983=EDGE_CURVE('',#7292,#7290,#443,.T.);
#8984=EDGE_CURVE('',#7293,#7294,#4120,.T.);
#8985=EDGE_CURVE('',#7293,#7291,#444,.T.);
#8986=EDGE_CURVE('',#7294,#7292,#445,.T.);
#8987=EDGE_CURVE('',#7295,#7296,#4121,.T.);
#8988=EDGE_CURVE('',#7295,#7293,#446,.T.);
#8989=EDGE_CURVE('',#7296,#7294,#447,.T.);
#8990=EDGE_CURVE('',#7297,#7298,#4122,.T.);
#8991=EDGE_CURVE('',#7297,#7295,#448,.T.);
#8992=EDGE_CURVE('',#7298,#7296,#449,.T.);
#8993=EDGE_CURVE('',#7299,#7300,#4123,.T.);
#8994=EDGE_CURVE('',#7299,#7297,#450,.T.);
#8995=EDGE_CURVE('',#7300,#7298,#451,.T.);
#8996=EDGE_CURVE('',#7301,#7302,#4124,.T.);
#8997=EDGE_CURVE('',#7301,#7299,#452,.T.);
#8998=EDGE_CURVE('',#7302,#7300,#453,.T.);
#8999=EDGE_CURVE('',#7303,#7303,#6604,.T.);
#9000=EDGE_CURVE('',#7303,#7304,#4125,.T.);
#9001=EDGE_CURVE('',#7304,#7305,#6605,.T.);
#9002=EDGE_CURVE('',#7305,#7304,#6606,.T.);
#9003=EDGE_CURVE('',#7306,#7307,#6607,.T.);
#9004=EDGE_CURVE('',#7307,#7306,#6608,.T.);
#9005=EDGE_CURVE('',#7307,#7305,#4126,.T.);
#9006=EDGE_CURVE('',#7308,#7308,#6609,.T.);
#9007=EDGE_CURVE('',#7306,#7309,#4127,.T.);
#9008=EDGE_CURVE('',#7309,#7309,#6610,.T.);
#9009=EDGE_CURVE('',#7310,#7310,#6611,.T.);
#9010=EDGE_CURVE('',#7311,#7311,#6612,.T.);
#9011=EDGE_CURVE('',#7311,#7312,#4128,.T.);
#9012=EDGE_CURVE('',#7312,#7313,#6613,.T.);
#9013=EDGE_CURVE('',#7313,#7312,#6614,.T.);
#9014=EDGE_CURVE('',#7313,#7314,#4129,.T.);
#9015=EDGE_CURVE('',#7314,#7314,#6615,.T.);
#9016=EDGE_CURVE('',#7258,#7315,#454,.T.);
#9017=EDGE_CURVE('',#7315,#7316,#6616,.T.);
#9018=EDGE_CURVE('',#7316,#7259,#455,.T.);
#9019=EDGE_CURVE('',#7317,#7317,#6617,.T.);
#9020=EDGE_CURVE('',#7317,#7318,#4130,.T.);
#9021=EDGE_CURVE('',#7319,#7318,#456,.T.);
#9022=EDGE_CURVE('',#7319,#7320,#6618,.T.);
#9023=EDGE_CURVE('',#7318,#7320,#457,.T.);
#9024=EDGE_CURVE('',#7321,#7321,#6619,.T.);
#9025=EDGE_CURVE('',#7321,#7317,#4131,.T.);
#9026=EDGE_CURVE('',#7321,#7322,#4132,.T.);
#9027=EDGE_CURVE('',#7322,#7322,#6620,.T.);
#9028=EDGE_CURVE('',#7323,#7323,#6621,.T.);
#9029=EDGE_CURVE('',#7283,#7280,#458,.T.);
#9030=EDGE_CURVE('',#7324,#7280,#6622,.F.);
#9031=EDGE_CURVE('',#7324,#7284,#459,.T.);
#9032=EDGE_CURVE('',#7279,#7324,#460,.T.);
#9033=EDGE_CURVE('',#7316,#7302,#461,.T.);
#9034=EDGE_CURVE('',#7315,#7301,#462,.T.);
#9035=EDGE_CURVE('',#7278,#7324,#6623,.F.);
#9036=EDGE_CURVE('',#7325,#7227,#463,.T.);
#9037=EDGE_CURVE('',#7223,#7325,#464,.T.);
#9038=EDGE_CURVE('',#7326,#7193,#465,.T.);
#9039=EDGE_CURVE('',#7326,#7255,#466,.T.);
#9040=EDGE_CURVE('',#7193,#7327,#6624,.T.);
#9041=EDGE_CURVE('',#7327,#7192,#6625,.T.);
#9042=EDGE_CURVE('',#7192,#7328,#467,.T.);
#9043=EDGE_CURVE('',#7328,#7326,#6626,.T.);
#9044=EDGE_CURVE('',#7328,#7254,#468,.T.);
#9045=EDGE_CURVE('',#7226,#7329,#469,.T.);
#9046=EDGE_CURVE('',#7329,#7222,#470,.T.);
#9047=EDGE_CURVE('',#7330,#7331,#471,.T.);
#9048=EDGE_CURVE('',#7331,#7332,#4133,.T.);
#9049=EDGE_CURVE('',#7332,#7333,#472,.F.);
#9050=EDGE_CURVE('',#7333,#7330,#4134,.T.);
#9051=EDGE_CURVE('',#7334,#7330,#4135,.T.);
#9052=EDGE_CURVE('',#7335,#7334,#473,.T.);
#9053=EDGE_CURVE('',#7335,#7336,#6627,.T.);
#9054=EDGE_CURVE('',#7337,#7336,#474,.T.);
#9055=EDGE_CURVE('',#7337,#7319,#475,.T.);
#9056=EDGE_CURVE('',#7320,#7338,#476,.T.);
#9057=EDGE_CURVE('',#7339,#7338,#477,.T.);
#9058=EDGE_CURVE('',#7331,#7339,#6628,.T.);
#9059=EDGE_CURVE('',#7340,#7333,#6629,.T.);
#9060=EDGE_CURVE('',#7334,#7340,#4136,.T.);
#9061=EDGE_CURVE('',#7340,#7341,#478,.F.);
#9062=EDGE_CURVE('',#7341,#7335,#4137,.T.);
#9063=EDGE_CURVE('',#7342,#7343,#479,.T.);
#9064=EDGE_CURVE('',#7342,#7339,#4138,.T.);
#9065=EDGE_CURVE('',#7338,#7343,#4139,.T.);
#9066=EDGE_CURVE('',#7336,#7344,#4140,.T.);
#9067=EDGE_CURVE('',#7344,#7345,#480,.F.);
#9068=EDGE_CURVE('',#7345,#7337,#4141,.T.);
#9069=EDGE_CURVE('',#7346,#7346,#6630,.T.);
#9070=EDGE_CURVE('',#7346,#7347,#4142,.T.);
#9071=EDGE_CURVE('',#7347,#7347,#6631,.T.);
#9072=EDGE_CURVE('',#7348,#7348,#6632,.T.);
#9073=EDGE_CURVE('',#7347,#7349,#4143,.T.);
#9074=EDGE_CURVE('',#7349,#7349,#6633,.T.);
#9075=EDGE_CURVE('',#7323,#7350,#4144,.T.);
#9076=EDGE_CURVE('',#7350,#7350,#6634,.T.);
#9077=EDGE_CURVE('',#7350,#7351,#4145,.T.);
#9078=EDGE_CURVE('',#7351,#7351,#6635,.T.);
#9079=EDGE_CURVE('',#7348,#7352,#4146,.T.);
#9080=EDGE_CURVE('',#7352,#7352,#6636,.T.);
#9081=EDGE_CURVE('',#7352,#7353,#4147,.T.);
#9082=EDGE_CURVE('',#7314,#7353,#481,.T.);
#9083=EDGE_CURVE('',#7353,#7314,#482,.T.);
#9084=EDGE_CURVE('',#7343,#7345,#483,.T.);
#9085=EDGE_CURVE('',#7354,#7354,#6637,.T.);
#9086=EDGE_CURVE('',#7354,#7355,#4148,.T.);
#9087=EDGE_CURVE('',#7355,#7355,#6638,.T.);
#9088=EDGE_CURVE('',#7353,#7356,#4149,.T.);
#9089=EDGE_CURVE('',#7356,#7356,#6639,.T.);
#9090=EDGE_CURVE('',#7344,#7341,#4150,.T.);
#9091=EDGE_CURVE('',#7332,#7342,#4151,.T.);
#9092=EDGE_CURVE('',#7308,#7357,#4152,.T.);
#9093=EDGE_CURVE('',#7357,#7357,#6640,.T.);
#9094=EDGE_CURVE('',#7358,#7358,#6641,.T.);
#9095=EDGE_CURVE('',#7327,#7358,#4153,.T.);
#9096=EDGE_CURVE('',#7329,#7325,#6642,.T.);
#9097=EDGE_CURVE('',#7359,#7359,#6643,.T.);
#9098=EDGE_CURVE('',#7356,#7359,#4154,.T.);
#9099=EDGE_CURVE('',#7310,#7278,#4155,.T.);
#9100=EDGE_CURVE('',#7360,#7360,#6644,.T.);
#9101=EDGE_CURVE('',#7360,#7361,#4156,.T.);
#9102=EDGE_CURVE('',#7361,#7361,#6645,.T.);
#9103=EDGE_CURVE('',#7362,#7362,#6646,.T.);
#9104=EDGE_CURVE('',#7363,#7363,#6647,.T.);
#9105=EDGE_CURVE('',#7363,#7362,#4157,.T.);
#9106=EDGE_CURVE('',#7364,#7364,#6648,.T.);
#9107=EDGE_CURVE('',#7364,#7363,#4158,.T.);
#9108=EDGE_CURVE('',#7365,#7365,#6649,.T.);
#9109=EDGE_CURVE('',#7366,#7366,#6650,.T.);
#9110=EDGE_CURVE('',#7366,#7365,#4159,.T.);
#9111=EDGE_CURVE('',#7367,#7367,#6651,.T.);
#9112=EDGE_CURVE('',#7367,#7366,#4160,.T.);
#9113=EDGE_CURVE('',#7368,#7368,#6652,.T.);
#9114=EDGE_CURVE('',#7369,#7369,#6653,.T.);
#9115=EDGE_CURVE('',#7369,#7368,#4161,.T.);
#9116=EDGE_CURVE('',#7370,#7370,#6654,.T.);
#9117=EDGE_CURVE('',#7371,#7371,#6655,.T.);
#9118=EDGE_CURVE('',#7371,#7370,#4162,.T.);
#9119=EDGE_CURVE('',#7372,#7372,#6656,.T.);
#9120=EDGE_CURVE('',#7373,#7373,#6657,.T.);
#9121=EDGE_CURVE('',#7373,#7372,#4163,.T.);
#9122=EDGE_CURVE('',#7374,#7374,#6658,.T.);
#9123=EDGE_CURVE('',#7375,#7375,#6659,.T.);
#9124=EDGE_CURVE('',#7375,#7374,#4164,.T.);
#9125=EDGE_CURVE('',#7376,#7376,#6660,.T.);
#9126=EDGE_CURVE('',#7376,#7375,#4165,.T.);
#9127=EDGE_CURVE('',#7377,#7377,#6661,.T.);
#9128=EDGE_CURVE('',#7377,#7378,#484,.T.);
#9129=EDGE_CURVE('',#7378,#7378,#6662,.T.);
#9130=EDGE_CURVE('',#7379,#7379,#6663,.T.);
#9131=EDGE_CURVE('',#7379,#7379,#6664,.T.);
#9132=EDGE_CURVE('',#7380,#7380,#6665,.T.);
#9133=EDGE_CURVE('',#7380,#7381,#4166,.T.);
#9134=EDGE_CURVE('',#7381,#7381,#6666,.T.);
#9135=EDGE_CURVE('',#7382,#7382,#6667,.T.);
#9136=EDGE_CURVE('',#7383,#7383,#6668,.T.);
#9137=EDGE_CURVE('',#7383,#7382,#4167,.T.);
#9138=EDGE_CURVE('',#7384,#7384,#6669,.T.);
#9139=EDGE_CURVE('',#7385,#7385,#6670,.T.);
#9140=EDGE_CURVE('',#7385,#7384,#4168,.T.);
#9141=EDGE_CURVE('',#7386,#7386,#6671,.T.);
#9142=EDGE_CURVE('',#7386,#7385,#4169,.T.);
#9143=EDGE_CURVE('',#7387,#7387,#6672,.T.);
#9144=EDGE_CURVE('',#7387,#7386,#4170,.T.);
#9145=EDGE_CURVE('',#7388,#7389,#4171,.T.);
#9146=EDGE_CURVE('',#7389,#7390,#4172,.T.);
#9147=EDGE_CURVE('',#7390,#7391,#4173,.T.);
#9148=EDGE_CURVE('',#7391,#7388,#4174,.T.);
#9149=EDGE_CURVE('',#7388,#7392,#4175,.T.);
#9150=EDGE_CURVE('',#7393,#7392,#4176,.T.);
#9151=EDGE_CURVE('',#7393,#7394,#4177,.T.);
#9152=EDGE_CURVE('',#7394,#7395,#4178,.T.);
#9153=EDGE_CURVE('',#7395,#7389,#4179,.T.);
#9154=EDGE_CURVE('',#7396,#7391,#4180,.T.);
#9155=EDGE_CURVE('',#7392,#7396,#4181,.T.);
#9156=EDGE_CURVE('',#7397,#7398,#4182,.T.);
#9157=EDGE_CURVE('',#7398,#7399,#4183,.T.);
#9158=EDGE_CURVE('',#7399,#7400,#4184,.T.);
#9159=EDGE_CURVE('',#7400,#7397,#4185,.T.);
#9160=EDGE_CURVE('',#7401,#7400,#4186,.T.);
#9161=EDGE_CURVE('',#7402,#7401,#4187,.T.);
#9162=EDGE_CURVE('',#7397,#7402,#4188,.T.);
#9163=EDGE_CURVE('',#7399,#7395,#4189,.T.);
#9164=EDGE_CURVE('',#7395,#7403,#4190,.T.);
#9165=EDGE_CURVE('',#7403,#7404,#4191,.T.);
#9166=EDGE_CURVE('',#7401,#7404,#4192,.T.);
#9167=EDGE_CURVE('',#7405,#7406,#4193,.T.);
#9168=EDGE_CURVE('',#7406,#7407,#4194,.T.);
#9169=EDGE_CURVE('',#7407,#7408,#4195,.T.);
#9170=EDGE_CURVE('',#7408,#7409,#4196,.T.);
#9171=EDGE_CURVE('',#7409,#7410,#4197,.T.);
#9172=EDGE_CURVE('',#7410,#7405,#4198,.T.);
#9173=EDGE_CURVE('',#7411,#7406,#4199,.T.);
#9174=EDGE_CURVE('',#7412,#7411,#4200,.T.);
#9175=EDGE_CURVE('',#7407,#7412,#4201,.T.);
#9176=EDGE_CURVE('',#7413,#7405,#4202,.T.);
#9177=EDGE_CURVE('',#7413,#7414,#4203,.T.);
#9178=EDGE_CURVE('',#7414,#7415,#4204,.T.);
#9179=EDGE_CURVE('',#7411,#7415,#4205,.T.);
#9180=EDGE_CURVE('',#7410,#7416,#4206,.T.);
#9181=EDGE_CURVE('',#7417,#7416,#4207,.T.);
#9182=EDGE_CURVE('',#7417,#7413,#4208,.T.);
#9183=EDGE_CURVE('',#7418,#7419,#4209,.T.);
#9184=EDGE_CURVE('',#7419,#7420,#4210,.T.);
#9185=EDGE_CURVE('',#7420,#7421,#4211,.T.);
#9186=EDGE_CURVE('',#7421,#7422,#4212,.T.);
#9187=EDGE_CURVE('',#7422,#7418,#4213,.T.);
#9188=EDGE_CURVE('',#7423,#7418,#4214,.T.);
#9189=EDGE_CURVE('',#7422,#7424,#4215,.T.);
#9190=EDGE_CURVE('',#7424,#7423,#4216,.T.);
#9191=EDGE_CURVE('',#7408,#7425,#4217,.T.);
#9192=EDGE_CURVE('',#7425,#7423,#4218,.T.);
#9193=EDGE_CURVE('',#7424,#7409,#4219,.T.);
#9194=EDGE_CURVE('',#7419,#7426,#4220,.T.);
#9195=EDGE_CURVE('',#7426,#7427,#4221,.T.);
#9196=EDGE_CURVE('',#7428,#7427,#4222,.T.);
#9197=EDGE_CURVE('',#7428,#7429,#4223,.T.);
#9198=EDGE_CURVE('',#7420,#7429,#4224,.T.);
#9199=EDGE_CURVE('',#7430,#7425,#4225,.T.);
#9200=EDGE_CURVE('',#7431,#7430,#4226,.T.);
#9201=EDGE_CURVE('',#7432,#7431,#4227,.T.);
#9202=EDGE_CURVE('',#7426,#7432,#4228,.T.);
#9203=EDGE_CURVE('',#7433,#7412,#4229,.T.);
#9204=EDGE_CURVE('',#7433,#7430,#4230,.T.);
#9205=EDGE_CURVE('',#7434,#7435,#4231,.T.);
#9206=EDGE_CURVE('',#7435,#7436,#4232,.T.);
#9207=EDGE_CURVE('',#7436,#7437,#4233,.T.);
#9208=EDGE_CURVE('',#7437,#7434,#4234,.T.);
#9209=EDGE_CURVE('',#7434,#7438,#4235,.T.);
#9210=EDGE_CURVE('',#7439,#7438,#4236,.T.);
#9211=EDGE_CURVE('',#7439,#7414,#4237,.T.);
#9212=EDGE_CURVE('',#7414,#7394,#4238,.T.);
#9213=EDGE_CURVE('',#7394,#7435,#4239,.T.);
#9214=EDGE_CURVE('',#7440,#7437,#4240,.T.);
#9215=EDGE_CURVE('',#7438,#7440,#4241,.T.);
#9216=EDGE_CURVE('',#7396,#7441,#4242,.T.);
#9217=EDGE_CURVE('',#7441,#7393,#4243,.T.);
#9218=EDGE_CURVE('',#7415,#7433,#4244,.T.);
#9219=EDGE_CURVE('',#7442,#7439,#4245,.T.);
#9220=EDGE_CURVE('',#7430,#7442,#4246,.T.);
#9221=EDGE_CURVE('',#7440,#7442,#4247,.T.);
#9222=EDGE_CURVE('',#7443,#7444,#4248,.T.);
#9223=EDGE_CURVE('',#7444,#7445,#4249,.T.);
#9224=EDGE_CURVE('',#7445,#7446,#4250,.T.);
#9225=EDGE_CURVE('',#7446,#7447,#4251,.T.);
#9226=EDGE_CURVE('',#7447,#7443,#4252,.T.);
#9227=EDGE_CURVE('',#7447,#7417,#4253,.T.);
#9228=EDGE_CURVE('',#7416,#7443,#4254,.T.);
#9229=EDGE_CURVE('',#7403,#7446,#4255,.T.);
#9230=EDGE_CURVE('',#7448,#7449,#485,.T.);
#9231=EDGE_CURVE('',#7449,#7450,#4256,.T.);
#9232=EDGE_CURVE('',#7450,#7451,#4257,.T.);
#9233=EDGE_CURVE('',#7451,#7452,#4258,.T.);
#9234=EDGE_CURVE('',#7452,#7453,#4259,.T.);
#9235=EDGE_CURVE('',#7453,#7454,#4260,.T.);
#9236=EDGE_CURVE('',#7454,#7455,#486,.T.);
#9237=EDGE_CURVE('',#7455,#7456,#487,.T.);
#9238=EDGE_CURVE('',#7456,#7457,#4261,.T.);
#9239=EDGE_CURVE('',#7457,#7458,#4262,.T.);
#9240=EDGE_CURVE('',#7458,#7459,#4263,.T.);
#9241=EDGE_CURVE('',#7459,#7460,#488,.T.);
#9242=EDGE_CURVE('',#7460,#7461,#489,.T.);
#9243=EDGE_CURVE('',#7461,#7462,#4264,.T.);
#9244=EDGE_CURVE('',#7462,#7463,#4265,.T.);
#9245=EDGE_CURVE('',#7463,#7464,#4266,.T.);
#9246=EDGE_CURVE('',#7464,#7465,#4267,.T.);
#9247=EDGE_CURVE('',#7465,#7466,#4268,.T.);
#9248=EDGE_CURVE('',#7466,#7448,#490,.T.);
#9249=EDGE_CURVE('',#7467,#7468,#4269,.T.);
#9250=EDGE_CURVE('',#7468,#7469,#4270,.T.);
#9251=EDGE_CURVE('',#7469,#7470,#4271,.T.);
#9252=EDGE_CURVE('',#7470,#7471,#4272,.T.);
#9253=EDGE_CURVE('',#7471,#7472,#4273,.T.);
#9254=EDGE_CURVE('',#7472,#7473,#4274,.T.);
#9255=EDGE_CURVE('',#7473,#7474,#4275,.T.);
#9256=EDGE_CURVE('',#7474,#7467,#4276,.T.);
#9257=EDGE_CURVE('',#7475,#7476,#491,.T.);
#9258=EDGE_CURVE('',#7476,#7477,#492,.T.);
#9259=EDGE_CURVE('',#7477,#7478,#493,.T.);
#9260=EDGE_CURVE('',#7478,#7479,#494,.T.);
#9261=EDGE_CURVE('',#7479,#7480,#495,.T.);
#9262=EDGE_CURVE('',#7480,#7481,#496,.T.);
#9263=EDGE_CURVE('',#7481,#7482,#497,.T.);
#9264=EDGE_CURVE('',#7482,#7483,#498,.T.);
#9265=EDGE_CURVE('',#7483,#7484,#499,.T.);
#9266=EDGE_CURVE('',#7484,#7485,#500,.T.);
#9267=EDGE_CURVE('',#7485,#7486,#501,.T.);
#9268=EDGE_CURVE('',#7486,#7475,#502,.T.);
#9269=EDGE_CURVE('',#7487,#7488,#503,.T.);
#9270=EDGE_CURVE('',#7488,#7489,#4277,.T.);
#9271=EDGE_CURVE('',#7489,#7490,#4278,.T.);
#9272=EDGE_CURVE('',#7490,#7491,#4279,.T.);
#9273=EDGE_CURVE('',#7491,#7492,#4280,.T.);
#9274=EDGE_CURVE('',#7492,#7493,#504,.T.);
#9275=EDGE_CURVE('',#7493,#7494,#505,.T.);
#9276=EDGE_CURVE('',#7494,#7495,#4281,.T.);
#9277=EDGE_CURVE('',#7495,#7487,#506,.T.);
#9278=EDGE_CURVE('',#7496,#7497,#507,.T.);
#9279=EDGE_CURVE('',#7497,#7498,#4282,.T.);
#9280=EDGE_CURVE('',#7498,#7499,#4283,.T.);
#9281=EDGE_CURVE('',#7499,#7500,#4284,.T.);
#9282=EDGE_CURVE('',#7500,#7501,#4285,.T.);
#9283=EDGE_CURVE('',#7501,#7502,#4286,.T.);
#9284=EDGE_CURVE('',#7502,#7503,#508,.T.);
#9285=EDGE_CURVE('',#7503,#7504,#509,.T.);
#9286=EDGE_CURVE('',#7504,#7505,#510,.T.);
#9287=EDGE_CURVE('',#7505,#7506,#511,.T.);
#9288=EDGE_CURVE('',#7506,#7507,#512,.T.);
#9289=EDGE_CURVE('',#7507,#7508,#513,.T.);
#9290=EDGE_CURVE('',#7508,#7509,#514,.T.);
#9291=EDGE_CURVE('',#7509,#7510,#515,.T.);
#9292=EDGE_CURVE('',#7510,#7511,#516,.T.);
#9293=EDGE_CURVE('',#7511,#7512,#517,.T.);
#9294=EDGE_CURVE('',#7512,#7513,#518,.T.);
#9295=EDGE_CURVE('',#7513,#7514,#4287,.T.);
#9296=EDGE_CURVE('',#7514,#7515,#519,.T.);
#9297=EDGE_CURVE('',#7515,#7516,#520,.T.);
#9298=EDGE_CURVE('',#7516,#7517,#521,.T.);
#9299=EDGE_CURVE('',#7517,#7518,#522,.T.);
#9300=EDGE_CURVE('',#7518,#7519,#523,.T.);
#9301=EDGE_CURVE('',#7519,#7520,#524,.T.);
#9302=EDGE_CURVE('',#7520,#7521,#525,.T.);
#9303=EDGE_CURVE('',#7521,#7522,#526,.T.);
#9304=EDGE_CURVE('',#7522,#7523,#527,.T.);
#9305=EDGE_CURVE('',#7523,#7524,#528,.T.);
#9306=EDGE_CURVE('',#7524,#7496,#529,.T.);
#9307=EDGE_CURVE('',#7525,#7445,#4288,.T.);
#9308=EDGE_CURVE('',#7525,#7526,#4289,.T.);
#9309=EDGE_CURVE('',#7527,#7526,#4290,.T.);
#9310=EDGE_CURVE('',#7527,#7403,#4291,.T.);
#9311=EDGE_CURVE('',#7429,#7525,#4292,.T.);
#9312=EDGE_CURVE('',#7444,#7421,#4293,.T.);
#9313=EDGE_CURVE('',#7526,#7428,#4294,.T.);
#9314=EDGE_CURVE('',#7404,#7528,#4295,.T.);
#9315=EDGE_CURVE('',#7528,#7402,#4296,.T.);
#9316=EDGE_CURVE('',#7528,#7426,#4297,.T.);
#9317=EDGE_CURVE('',#7432,#7398,#4298,.T.);
#9318=EDGE_CURVE('',#7427,#7527,#4299,.T.);
#9319=EDGE_CURVE('',#7448,#7529,#4300,.T.);
#9320=EDGE_CURVE('',#7529,#7530,#530,.T.);
#9321=EDGE_CURVE('',#7449,#7530,#4301,.T.);
#9322=EDGE_CURVE('',#7466,#7531,#4302,.T.);
#9323=EDGE_CURVE('',#7531,#7529,#531,.T.);
#9324=EDGE_CURVE('',#7465,#7532,#4303,.T.);
#9325=EDGE_CURVE('',#7532,#7531,#4304,.T.);
#9326=EDGE_CURVE('',#7464,#7533,#4305,.T.);
#9327=EDGE_CURVE('',#7533,#7532,#4306,.T.);
#9328=EDGE_CURVE('',#7463,#7534,#4307,.T.);
#9329=EDGE_CURVE('',#7534,#7533,#4308,.T.);
#9330=EDGE_CURVE('',#7462,#7535,#4309,.T.);
#9331=EDGE_CURVE('',#7535,#7534,#4310,.T.);
#9332=EDGE_CURVE('',#7461,#7536,#4311,.T.);
#9333=EDGE_CURVE('',#7536,#7535,#4312,.T.);
#9334=EDGE_CURVE('',#7460,#7537,#4313,.T.);
#9335=EDGE_CURVE('',#7537,#7536,#532,.T.);
#9336=EDGE_CURVE('',#7459,#7538,#4314,.T.);
#9337=EDGE_CURVE('',#7538,#7537,#533,.T.);
#9338=EDGE_CURVE('',#7458,#7539,#4315,.T.);
#9339=EDGE_CURVE('',#7539,#7538,#4316,.T.);
#9340=EDGE_CURVE('',#7457,#7540,#4317,.T.);
#9341=EDGE_CURVE('',#7540,#7539,#4318,.T.);
#9342=EDGE_CURVE('',#7456,#7541,#4319,.T.);
#9343=EDGE_CURVE('',#7541,#7540,#4320,.T.);
#9344=EDGE_CURVE('',#7455,#7542,#4321,.T.);
#9345=EDGE_CURVE('',#7542,#7541,#534,.T.);
#9346=EDGE_CURVE('',#7454,#7543,#4322,.T.);
#9347=EDGE_CURVE('',#7543,#7542,#535,.T.);
#9348=EDGE_CURVE('',#7453,#7544,#4323,.T.);
#9349=EDGE_CURVE('',#7544,#7543,#4324,.T.);
#9350=EDGE_CURVE('',#7452,#7545,#4325,.T.);
#9351=EDGE_CURVE('',#7545,#7544,#4326,.T.);
#9352=EDGE_CURVE('',#7451,#7546,#4327,.T.);
#9353=EDGE_CURVE('',#7546,#7545,#4328,.T.);
#9354=EDGE_CURVE('',#7450,#7547,#4329,.T.);
#9355=EDGE_CURVE('',#7547,#7546,#4330,.T.);
#9356=EDGE_CURVE('',#7530,#7547,#4331,.T.);
#9357=EDGE_CURVE('',#7467,#7548,#4332,.T.);
#9358=EDGE_CURVE('',#7548,#7549,#4333,.T.);
#9359=EDGE_CURVE('',#7468,#7549,#4334,.T.);
#9360=EDGE_CURVE('',#7474,#7550,#4335,.T.);
#9361=EDGE_CURVE('',#7550,#7548,#4336,.T.);
#9362=EDGE_CURVE('',#7473,#7551,#4337,.T.);
#9363=EDGE_CURVE('',#7551,#7550,#4338,.T.);
#9364=EDGE_CURVE('',#7472,#7552,#4339,.T.);
#9365=EDGE_CURVE('',#7552,#7551,#4340,.T.);
#9366=EDGE_CURVE('',#7471,#7553,#4341,.T.);
#9367=EDGE_CURVE('',#7553,#7552,#4342,.T.);
#9368=EDGE_CURVE('',#7470,#7554,#4343,.T.);
#9369=EDGE_CURVE('',#7554,#7553,#4344,.T.);
#9370=EDGE_CURVE('',#7469,#7555,#4345,.T.);
#9371=EDGE_CURVE('',#7555,#7554,#4346,.T.);
#9372=EDGE_CURVE('',#7549,#7555,#4347,.T.);
#9373=EDGE_CURVE('',#7475,#7556,#4348,.T.);
#9374=EDGE_CURVE('',#7556,#7557,#536,.T.);
#9375=EDGE_CURVE('',#7476,#7557,#4349,.T.);
#9376=EDGE_CURVE('',#7486,#7558,#4350,.T.);
#9377=EDGE_CURVE('',#7558,#7556,#537,.T.);
#9378=EDGE_CURVE('',#7485,#7559,#4351,.T.);
#9379=EDGE_CURVE('',#7559,#7558,#538,.T.);
#9380=EDGE_CURVE('',#7484,#7560,#4352,.T.);
#9381=EDGE_CURVE('',#7560,#7559,#539,.T.);
#9382=EDGE_CURVE('',#7483,#7561,#4353,.T.);
#9383=EDGE_CURVE('',#7561,#7560,#540,.T.);
#9384=EDGE_CURVE('',#7482,#7562,#4354,.T.);
#9385=EDGE_CURVE('',#7562,#7561,#541,.T.);
#9386=EDGE_CURVE('',#7481,#7563,#4355,.T.);
#9387=EDGE_CURVE('',#7563,#7562,#542,.T.);
#9388=EDGE_CURVE('',#7480,#7564,#4356,.T.);
#9389=EDGE_CURVE('',#7564,#7563,#543,.T.);
#9390=EDGE_CURVE('',#7479,#7565,#4357,.T.);
#9391=EDGE_CURVE('',#7565,#7564,#544,.T.);
#9392=EDGE_CURVE('',#7478,#7566,#4358,.T.);
#9393=EDGE_CURVE('',#7566,#7565,#545,.T.);
#9394=EDGE_CURVE('',#7477,#7567,#4359,.T.);
#9395=EDGE_CURVE('',#7567,#7566,#546,.T.);
#9396=EDGE_CURVE('',#7557,#7567,#547,.T.);
#9397=EDGE_CURVE('',#7487,#7568,#4360,.T.);
#9398=EDGE_CURVE('',#7568,#7569,#548,.T.);
#9399=EDGE_CURVE('',#7488,#7569,#4361,.T.);
#9400=EDGE_CURVE('',#7495,#7570,#4362,.T.);
#9401=EDGE_CURVE('',#7570,#7568,#549,.T.);
#9402=EDGE_CURVE('',#7494,#7571,#4363,.T.);
#9403=EDGE_CURVE('',#7571,#7570,#4364,.T.);
#9404=EDGE_CURVE('',#7493,#7572,#4365,.T.);
#9405=EDGE_CURVE('',#7572,#7571,#550,.T.);
#9406=EDGE_CURVE('',#7492,#7573,#4366,.T.);
#9407=EDGE_CURVE('',#7573,#7572,#551,.T.);
#9408=EDGE_CURVE('',#7491,#7574,#4367,.T.);
#9409=EDGE_CURVE('',#7574,#7573,#4368,.T.);
#9410=EDGE_CURVE('',#7490,#7575,#4369,.T.);
#9411=EDGE_CURVE('',#7575,#7574,#4370,.T.);
#9412=EDGE_CURVE('',#7489,#7576,#4371,.T.);
#9413=EDGE_CURVE('',#7576,#7575,#4372,.T.);
#9414=EDGE_CURVE('',#7569,#7576,#4373,.T.);
#9415=EDGE_CURVE('',#7496,#7577,#4374,.T.);
#9416=EDGE_CURVE('',#7577,#7578,#552,.T.);
#9417=EDGE_CURVE('',#7497,#7578,#4375,.T.);
#9418=EDGE_CURVE('',#7524,#7579,#4376,.T.);
#9419=EDGE_CURVE('',#7579,#7577,#553,.T.);
#9420=EDGE_CURVE('',#7523,#7580,#4377,.T.);
#9421=EDGE_CURVE('',#7580,#7579,#554,.T.);
#9422=EDGE_CURVE('',#7522,#7581,#4378,.T.);
#9423=EDGE_CURVE('',#7581,#7580,#555,.T.);
#9424=EDGE_CURVE('',#7521,#7582,#4379,.T.);
#9425=EDGE_CURVE('',#7582,#7581,#556,.T.);
#9426=EDGE_CURVE('',#7520,#7583,#4380,.T.);
#9427=EDGE_CURVE('',#7583,#7582,#557,.T.);
#9428=EDGE_CURVE('',#7519,#7584,#4381,.T.);
#9429=EDGE_CURVE('',#7584,#7583,#558,.T.);
#9430=EDGE_CURVE('',#7518,#7585,#4382,.T.);
#9431=EDGE_CURVE('',#7585,#7584,#559,.T.);
#9432=EDGE_CURVE('',#7517,#7586,#4383,.T.);
#9433=EDGE_CURVE('',#7586,#7585,#560,.T.);
#9434=EDGE_CURVE('',#7516,#7587,#4384,.T.);
#9435=EDGE_CURVE('',#7587,#7586,#561,.T.);
#9436=EDGE_CURVE('',#7515,#7588,#4385,.T.);
#9437=EDGE_CURVE('',#7588,#7587,#562,.T.);
#9438=EDGE_CURVE('',#7514,#7589,#4386,.T.);
#9439=EDGE_CURVE('',#7589,#7588,#563,.T.);
#9440=EDGE_CURVE('',#7513,#7590,#4387,.T.);
#9441=EDGE_CURVE('',#7590,#7589,#4388,.T.);
#9442=EDGE_CURVE('',#7512,#7591,#4389,.T.);
#9443=EDGE_CURVE('',#7591,#7590,#564,.T.);
#9444=EDGE_CURVE('',#7511,#7592,#4390,.T.);
#9445=EDGE_CURVE('',#7592,#7591,#565,.T.);
#9446=EDGE_CURVE('',#7510,#7593,#4391,.T.);
#9447=EDGE_CURVE('',#7593,#7592,#566,.T.);
#9448=EDGE_CURVE('',#7509,#7594,#4392,.T.);
#9449=EDGE_CURVE('',#7594,#7593,#567,.T.);
#9450=EDGE_CURVE('',#7508,#7595,#4393,.T.);
#9451=EDGE_CURVE('',#7595,#7594,#568,.T.);
#9452=EDGE_CURVE('',#7507,#7596,#4394,.T.);
#9453=EDGE_CURVE('',#7596,#7595,#569,.T.);
#9454=EDGE_CURVE('',#7506,#7597,#4395,.T.);
#9455=EDGE_CURVE('',#7597,#7596,#570,.T.);
#9456=EDGE_CURVE('',#7505,#7598,#4396,.T.);
#9457=EDGE_CURVE('',#7598,#7597,#571,.T.);
#9458=EDGE_CURVE('',#7504,#7599,#4397,.T.);
#9459=EDGE_CURVE('',#7599,#7598,#572,.T.);
#9460=EDGE_CURVE('',#7503,#7600,#4398,.T.);
#9461=EDGE_CURVE('',#7600,#7599,#573,.T.);
#9462=EDGE_CURVE('',#7502,#7601,#4399,.T.);
#9463=EDGE_CURVE('',#7601,#7600,#574,.T.);
#9464=EDGE_CURVE('',#7501,#7602,#4400,.T.);
#9465=EDGE_CURVE('',#7602,#7601,#4401,.T.);
#9466=EDGE_CURVE('',#7500,#7603,#4402,.T.);
#9467=EDGE_CURVE('',#7603,#7602,#4403,.T.);
#9468=EDGE_CURVE('',#7499,#7604,#4404,.T.);
#9469=EDGE_CURVE('',#7604,#7603,#4405,.T.);
#9470=EDGE_CURVE('',#7498,#7605,#4406,.T.);
#9471=EDGE_CURVE('',#7605,#7604,#4407,.T.);
#9472=EDGE_CURVE('',#7578,#7605,#4408,.T.);
#9473=EDGE_CURVE('',#7431,#7441,#4409,.T.);
#9474=EDGE_CURVE('',#7436,#7431,#4410,.T.);
#9475=EDGE_CURVE('',#7390,#7432,#4411,.T.);
#9476=EDGE_CURVE('',#7416,#7424,#4412,.T.);
#9477=EDGE_CURVE('',#7443,#7422,#4413,.T.);
#9478=EDGE_CURVE('',#7606,#7606,#6673,.T.);
#9479=EDGE_CURVE('',#7607,#7607,#6674,.T.);
#9480=EDGE_CURVE('',#7607,#7606,#4414,.T.);
#9481=EDGE_CURVE('',#7608,#7608,#6675,.T.);
#9482=EDGE_CURVE('',#7608,#7607,#4415,.T.);
#9483=EDGE_CURVE('',#7609,#7609,#6676,.T.);
#9484=EDGE_CURVE('',#7610,#7610,#6677,.T.);
#9485=EDGE_CURVE('',#7610,#7609,#4416,.T.);
#9486=EDGE_CURVE('',#7611,#7611,#6678,.T.);
#9487=EDGE_CURVE('',#7612,#7612,#6679,.T.);
#9488=EDGE_CURVE('',#7612,#7611,#4417,.T.);
#9489=EDGE_CURVE('',#7613,#7613,#6680,.T.);
#9490=EDGE_CURVE('',#7614,#7614,#6681,.T.);
#9491=EDGE_CURVE('',#7614,#7613,#4418,.T.);
#9492=EDGE_CURVE('',#7615,#7615,#6682,.T.);
#9493=EDGE_CURVE('',#7616,#7616,#6683,.T.);
#9494=EDGE_CURVE('',#7616,#7615,#4419,.T.);
#9495=EDGE_CURVE('',#7617,#7617,#6684,.T.);
#9496=EDGE_CURVE('',#7617,#7616,#4420,.T.);
#9497=EDGE_CURVE('',#7618,#7619,#4421,.T.);
#9498=EDGE_CURVE('',#7618,#7620,#575,.T.);
#9499=EDGE_CURVE('',#7620,#7621,#6685,.F.);
#9500=EDGE_CURVE('',#7621,#7619,#576,.T.);
#9501=EDGE_CURVE('',#7622,#7623,#4422,.T.);
#9502=EDGE_CURVE('',#7622,#7618,#577,.T.);
#9503=EDGE_CURVE('',#7619,#7623,#578,.T.);
#9504=EDGE_CURVE('',#7624,#7625,#4423,.T.);
#9505=EDGE_CURVE('',#7624,#7622,#579,.T.);
#9506=EDGE_CURVE('',#7623,#7625,#580,.T.);
#9507=EDGE_CURVE('',#7626,#7627,#4424,.T.);
#9508=EDGE_CURVE('',#7626,#7624,#581,.T.);
#9509=EDGE_CURVE('',#7625,#7627,#582,.T.);
#9510=EDGE_CURVE('',#7628,#7629,#4425,.T.);
#9511=EDGE_CURVE('',#7628,#7626,#583,.T.);
#9512=EDGE_CURVE('',#7627,#7629,#584,.T.);
#9513=EDGE_CURVE('',#7630,#7631,#4426,.T.);
#9514=EDGE_CURVE('',#7630,#7628,#585,.T.);
#9515=EDGE_CURVE('',#7629,#7631,#586,.T.);
#9516=EDGE_CURVE('',#7632,#7633,#4427,.T.);
#9517=EDGE_CURVE('',#7632,#7630,#587,.T.);
#9518=EDGE_CURVE('',#7631,#7633,#588,.T.);
#9519=EDGE_CURVE('',#7634,#7635,#4428,.T.);
#9520=EDGE_CURVE('',#7634,#7632,#589,.T.);
#9521=EDGE_CURVE('',#7633,#7635,#590,.T.);
#9522=EDGE_CURVE('',#7636,#7637,#4429,.T.);
#9523=EDGE_CURVE('',#7636,#7634,#591,.T.);
#9524=EDGE_CURVE('',#7635,#7637,#592,.T.);
#9525=EDGE_CURVE('',#7638,#7639,#4430,.T.);
#9526=EDGE_CURVE('',#7638,#7636,#593,.T.);
#9527=EDGE_CURVE('',#7637,#7639,#594,.T.);
#9528=EDGE_CURVE('',#7640,#7641,#4431,.T.);
#9529=EDGE_CURVE('',#7640,#7638,#595,.T.);
#9530=EDGE_CURVE('',#7639,#7641,#596,.T.);
#9531=EDGE_CURVE('',#7642,#7643,#4432,.T.);
#9532=EDGE_CURVE('',#7642,#7640,#597,.T.);
#9533=EDGE_CURVE('',#7641,#7643,#598,.T.);
#9534=EDGE_CURVE('',#7644,#7645,#4433,.T.);
#9535=EDGE_CURVE('',#7644,#7646,#599,.T.);
#9536=EDGE_CURVE('',#7647,#7646,#6686,.T.);
#9537=EDGE_CURVE('',#7645,#7647,#600,.T.);
#9538=EDGE_CURVE('',#7648,#7649,#4434,.T.);
#9539=EDGE_CURVE('',#7648,#7644,#601,.T.);
#9540=EDGE_CURVE('',#7649,#7645,#602,.T.);
#9541=EDGE_CURVE('',#7650,#7651,#4435,.T.);
#9542=EDGE_CURVE('',#7650,#7648,#603,.T.);
#9543=EDGE_CURVE('',#7651,#7649,#604,.T.);
#9544=EDGE_CURVE('',#7652,#7653,#4436,.T.);
#9545=EDGE_CURVE('',#7652,#7650,#605,.T.);
#9546=EDGE_CURVE('',#7653,#7651,#606,.T.);
#9547=EDGE_CURVE('',#7654,#7655,#4437,.T.);
#9548=EDGE_CURVE('',#7654,#7652,#607,.T.);
#9549=EDGE_CURVE('',#7655,#7653,#608,.T.);
#9550=EDGE_CURVE('',#7656,#7657,#4438,.T.);
#9551=EDGE_CURVE('',#7656,#7654,#609,.T.);
#9552=EDGE_CURVE('',#7657,#7655,#610,.T.);
#9553=EDGE_CURVE('',#7658,#7659,#4439,.T.);
#9554=EDGE_CURVE('',#7658,#7656,#611,.T.);
#9555=EDGE_CURVE('',#7659,#7657,#612,.T.);
#9556=EDGE_CURVE('',#7660,#7661,#4440,.T.);
#9557=EDGE_CURVE('',#7660,#7658,#613,.T.);
#9558=EDGE_CURVE('',#7661,#7659,#614,.T.);
#9559=EDGE_CURVE('',#7662,#7663,#4441,.T.);
#9560=EDGE_CURVE('',#7662,#7660,#615,.T.);
#9561=EDGE_CURVE('',#7663,#7661,#616,.T.);
#9562=EDGE_CURVE('',#7664,#7665,#4442,.T.);
#9563=EDGE_CURVE('',#7664,#7662,#617,.T.);
#9564=EDGE_CURVE('',#7665,#7663,#618,.T.);
#9565=EDGE_CURVE('',#7666,#7667,#4443,.T.);
#9566=EDGE_CURVE('',#7666,#7664,#619,.T.);
#9567=EDGE_CURVE('',#7667,#7665,#620,.T.);
#9568=EDGE_CURVE('',#7668,#7668,#6687,.T.);
#9569=EDGE_CURVE('',#7668,#7669,#4444,.T.);
#9570=EDGE_CURVE('',#7669,#7670,#6688,.T.);
#9571=EDGE_CURVE('',#7670,#7669,#6689,.T.);
#9572=EDGE_CURVE('',#7670,#7671,#4445,.T.);
#9573=EDGE_CURVE('',#7672,#7671,#6690,.T.);
#9574=EDGE_CURVE('',#7671,#7672,#6691,.T.);
#9575=EDGE_CURVE('',#7620,#7673,#621,.T.);
#9576=EDGE_CURVE('',#7673,#7674,#6692,.T.);
#9577=EDGE_CURVE('',#7674,#7621,#622,.T.);
#9578=EDGE_CURVE('',#7672,#7675,#4446,.T.);
#9579=EDGE_CURVE('',#7675,#7676,#6693,.T.);
#9580=EDGE_CURVE('',#7676,#7675,#6694,.T.);
#9581=EDGE_CURVE('',#7676,#7677,#4447,.T.);
#9582=EDGE_CURVE('',#7677,#7677,#6695,.T.);
#9583=EDGE_CURVE('',#7646,#7678,#623,.T.);
#9584=EDGE_CURVE('',#7679,#7678,#6696,.F.);
#9585=EDGE_CURVE('',#7680,#7679,#6697,.F.);
#9586=EDGE_CURVE('',#7680,#7647,#624,.T.);
#9587=EDGE_CURVE('',#7643,#7680,#625,.T.);
#9588=EDGE_CURVE('',#7674,#7667,#626,.T.);
#9589=EDGE_CURVE('',#7673,#7666,#627,.T.);
#9590=EDGE_CURVE('',#7678,#7642,#628,.T.);
#9591=EDGE_CURVE('',#7678,#7680,#6698,.F.);
#9592=EDGE_CURVE('',#7681,#7681,#6699,.T.);
#9593=EDGE_CURVE('',#7681,#7682,#4448,.T.);
#9594=EDGE_CURVE('',#7682,#7682,#6700,.T.);
#9595=EDGE_CURVE('',#7683,#7683,#6701,.T.);
#9596=EDGE_CURVE('',#7677,#7683,#4449,.T.);
#9597=EDGE_CURVE('',#7684,#7684,#6702,.T.);
#9598=EDGE_CURVE('',#7684,#7679,#4450,.T.);
#9599=EDGE_CURVE('',#7685,#7685,#6703,.T.);
#9600=EDGE_CURVE('',#7685,#7686,#4451,.T.);
#9601=EDGE_CURVE('',#7686,#7686,#6704,.T.);
#9602=EDGE_CURVE('',#7687,#7687,#6705,.T.);
#9603=EDGE_CURVE('',#7687,#7688,#4452,.T.);
#9604=EDGE_CURVE('',#7688,#7688,#6706,.T.);
#9605=EDGE_CURVE('',#7689,#7690,#4453,.T.);
#9606=EDGE_CURVE('',#7689,#7691,#629,.T.);
#9607=EDGE_CURVE('',#7691,#7692,#6707,.T.);
#9608=EDGE_CURVE('',#7692,#7690,#630,.T.);
#9609=EDGE_CURVE('',#7693,#7694,#4454,.T.);
#9610=EDGE_CURVE('',#7693,#7689,#631,.T.);
#9611=EDGE_CURVE('',#7690,#7694,#632,.T.);
#9612=EDGE_CURVE('',#7695,#7696,#4455,.T.);
#9613=EDGE_CURVE('',#7695,#7693,#633,.T.);
#9614=EDGE_CURVE('',#7694,#7696,#634,.T.);
#9615=EDGE_CURVE('',#7697,#7698,#4456,.T.);
#9616=EDGE_CURVE('',#7697,#7695,#635,.T.);
#9617=EDGE_CURVE('',#7696,#7698,#636,.T.);
#9618=EDGE_CURVE('',#7699,#7700,#4457,.T.);
#9619=EDGE_CURVE('',#7699,#7697,#637,.T.);
#9620=EDGE_CURVE('',#7698,#7700,#638,.T.);
#9621=EDGE_CURVE('',#7701,#7702,#4458,.T.);
#9622=EDGE_CURVE('',#7701,#7699,#639,.T.);
#9623=EDGE_CURVE('',#7700,#7702,#640,.T.);
#9624=EDGE_CURVE('',#7703,#7704,#4459,.T.);
#9625=EDGE_CURVE('',#7703,#7701,#641,.T.);
#9626=EDGE_CURVE('',#7702,#7704,#642,.T.);
#9627=EDGE_CURVE('',#7705,#7706,#4460,.T.);
#9628=EDGE_CURVE('',#7705,#7703,#643,.T.);
#9629=EDGE_CURVE('',#7704,#7706,#644,.T.);
#9630=EDGE_CURVE('',#7707,#7708,#4461,.T.);
#9631=EDGE_CURVE('',#7707,#7705,#645,.T.);
#9632=EDGE_CURVE('',#7706,#7708,#646,.T.);
#9633=EDGE_CURVE('',#7709,#7710,#4462,.T.);
#9634=EDGE_CURVE('',#7709,#7707,#647,.T.);
#9635=EDGE_CURVE('',#7708,#7710,#648,.T.);
#9636=EDGE_CURVE('',#7711,#7712,#4463,.T.);
#9637=EDGE_CURVE('',#7711,#7709,#649,.T.);
#9638=EDGE_CURVE('',#7710,#7712,#650,.T.);
#9639=EDGE_CURVE('',#7713,#7714,#4464,.T.);
#9640=EDGE_CURVE('',#7713,#7711,#651,.T.);
#9641=EDGE_CURVE('',#7712,#7714,#652,.T.);
#9642=EDGE_CURVE('',#7715,#7716,#4465,.T.);
#9643=EDGE_CURVE('',#7715,#7713,#653,.T.);
#9644=EDGE_CURVE('',#7714,#7716,#654,.T.);
#9645=EDGE_CURVE('',#7717,#7718,#4466,.T.);
#9646=EDGE_CURVE('',#7717,#7719,#655,.T.);
#9647=EDGE_CURVE('',#7718,#7719,#6708,.T.);
#9648=EDGE_CURVE('',#7720,#7721,#4467,.T.);
#9649=EDGE_CURVE('',#7720,#7717,#656,.T.);
#9650=EDGE_CURVE('',#7722,#7718,#6709,.T.);
#9651=EDGE_CURVE('',#7721,#7722,#657,.T.);
#9652=EDGE_CURVE('',#7723,#7724,#4468,.T.);
#9653=EDGE_CURVE('',#7723,#7720,#658,.T.);
#9654=EDGE_CURVE('',#7724,#7721,#659,.T.);
#9655=EDGE_CURVE('',#7725,#7726,#4469,.T.);
#9656=EDGE_CURVE('',#7725,#7723,#660,.T.);
#9657=EDGE_CURVE('',#7726,#7724,#661,.T.);
#9658=EDGE_CURVE('',#7727,#7728,#4470,.T.);
#9659=EDGE_CURVE('',#7727,#7725,#662,.T.);
#9660=EDGE_CURVE('',#7728,#7726,#663,.T.);
#9661=EDGE_CURVE('',#7729,#7730,#4471,.T.);
#9662=EDGE_CURVE('',#7729,#7727,#664,.T.);
#9663=EDGE_CURVE('',#7730,#7728,#665,.T.);
#9664=EDGE_CURVE('',#7731,#7732,#4472,.T.);
#9665=EDGE_CURVE('',#7731,#7729,#666,.T.);
#9666=EDGE_CURVE('',#7732,#7730,#667,.T.);
#9667=EDGE_CURVE('',#7733,#7734,#4473,.T.);
#9668=EDGE_CURVE('',#7733,#7731,#668,.T.);
#9669=EDGE_CURVE('',#7734,#7732,#669,.T.);
#9670=EDGE_CURVE('',#7735,#7736,#4474,.T.);
#9671=EDGE_CURVE('',#7735,#7733,#670,.T.);
#9672=EDGE_CURVE('',#7736,#7734,#671,.T.);
#9673=EDGE_CURVE('',#7737,#7738,#4475,.T.);
#9674=EDGE_CURVE('',#7737,#7735,#672,.T.);
#9675=EDGE_CURVE('',#7738,#7736,#673,.T.);
#9676=EDGE_CURVE('',#7739,#7740,#4476,.T.);
#9677=EDGE_CURVE('',#7739,#7737,#674,.T.);
#9678=EDGE_CURVE('',#7740,#7738,#675,.T.);
#9679=EDGE_CURVE('',#7741,#7742,#4477,.T.);
#9680=EDGE_CURVE('',#7741,#7739,#676,.T.);
#9681=EDGE_CURVE('',#7742,#7740,#677,.T.);
#9682=EDGE_CURVE('',#7743,#7744,#4478,.T.);
#9683=EDGE_CURVE('',#7743,#7741,#678,.T.);
#9684=EDGE_CURVE('',#7744,#7742,#679,.T.);
#9685=EDGE_CURVE('',#7745,#7746,#131,.T.);
#9686=EDGE_CURVE('',#7746,#7747,#4479,.T.);
#9687=EDGE_CURVE('',#7747,#7748,#132,.T.);
#9688=EDGE_CURVE('',#7748,#7749,#248,.T.);
#9689=EDGE_CURVE('',#7749,#7750,#4480,.T.);
#9690=EDGE_CURVE('',#7750,#7745,#249,.T.);
#9691=EDGE_CURVE('',#7746,#7747,#6710,.T.);
#9692=EDGE_CURVE('',#7751,#7752,#133,.T.);
#9693=EDGE_CURVE('',#7752,#7753,#4481,.T.);
#9694=EDGE_CURVE('',#7753,#7754,#134,.T.);
#9695=EDGE_CURVE('',#7754,#7755,#250,.T.);
#9696=EDGE_CURVE('',#7755,#7756,#4482,.T.);
#9697=EDGE_CURVE('',#7756,#7751,#251,.T.);
#9698=EDGE_CURVE('',#7745,#7748,#6711,.T.);
#9699=EDGE_CURVE('',#7750,#7757,#4483,.T.);
#9700=EDGE_CURVE('',#7757,#7758,#6712,.T.);
#9701=EDGE_CURVE('',#7758,#7759,#4484,.T.);
#9702=EDGE_CURVE('',#7759,#7760,#6713,.T.);
#9703=EDGE_CURVE('',#7760,#7761,#4485,.T.);
#9704=EDGE_CURVE('',#7761,#7762,#6714,.T.);
#9705=EDGE_CURVE('',#7762,#7755,#4486,.T.);
#9706=EDGE_CURVE('',#7763,#7754,#6715,.T.);
#9707=EDGE_CURVE('',#7763,#7764,#4487,.T.);
#9708=EDGE_CURVE('',#7764,#7765,#6716,.T.);
#9709=EDGE_CURVE('',#7765,#7766,#4488,.T.);
#9710=EDGE_CURVE('',#7766,#7767,#6717,.T.);
#9711=EDGE_CURVE('',#7767,#7768,#4489,.T.);
#9712=EDGE_CURVE('',#7768,#7768,#6718,.T.);
#9713=EDGE_CURVE('',#7767,#7769,#6719,.T.);
#9714=EDGE_CURVE('',#7769,#7770,#4490,.T.);
#9715=EDGE_CURVE('',#7770,#7764,#6720,.T.);
#9716=EDGE_CURVE('',#7751,#7763,#6721,.T.);
#9717=EDGE_CURVE('',#7756,#7771,#4491,.T.);
#9718=EDGE_CURVE('',#7771,#7772,#6722,.T.);
#9719=EDGE_CURVE('',#7772,#7773,#4492,.T.);
#9720=EDGE_CURVE('',#7773,#7774,#6723,.T.);
#9721=EDGE_CURVE('',#7774,#7775,#4493,.T.);
#9722=EDGE_CURVE('',#7775,#7776,#6724,.T.);
#9723=EDGE_CURVE('',#7776,#7749,#4494,.T.);
#9724=EDGE_CURVE('',#7777,#7778,#4495,.T.);
#9725=EDGE_CURVE('',#7778,#7779,#6725,.T.);
#9726=EDGE_CURVE('',#7779,#7780,#4496,.T.);
#9727=EDGE_CURVE('',#7780,#7777,#6726,.T.);
#9728=EDGE_CURVE('',#7781,#7782,#4497,.T.);
#9729=EDGE_CURVE('',#7782,#7783,#6727,.T.);
#9730=EDGE_CURVE('',#7783,#7784,#4498,.T.);
#9731=EDGE_CURVE('',#7784,#7781,#6728,.T.);
#9732=EDGE_CURVE('',#7785,#7786,#4499,.T.);
#9733=EDGE_CURVE('',#7786,#7787,#6729,.T.);
#9734=EDGE_CURVE('',#7787,#7788,#4500,.T.);
#9735=EDGE_CURVE('',#7788,#7785,#6730,.T.);
#9736=EDGE_CURVE('',#7789,#7790,#4501,.T.);
#9737=EDGE_CURVE('',#7790,#7791,#6731,.T.);
#9738=EDGE_CURVE('',#7791,#7792,#4502,.T.);
#9739=EDGE_CURVE('',#7792,#7789,#6732,.T.);
#9740=EDGE_CURVE('',#7793,#7794,#4503,.T.);
#9741=EDGE_CURVE('',#7794,#7795,#6733,.T.);
#9742=EDGE_CURVE('',#7795,#7796,#4504,.T.);
#9743=EDGE_CURVE('',#7796,#7793,#6734,.T.);
#9744=EDGE_CURVE('',#7797,#7798,#4505,.T.);
#9745=EDGE_CURVE('',#7798,#7799,#6735,.T.);
#9746=EDGE_CURVE('',#7799,#7800,#4506,.T.);
#9747=EDGE_CURVE('',#7800,#7797,#6736,.T.);
#9748=EDGE_CURVE('',#7801,#7802,#4507,.T.);
#9749=EDGE_CURVE('',#7802,#7803,#6737,.T.);
#9750=EDGE_CURVE('',#7803,#7804,#4508,.T.);
#9751=EDGE_CURVE('',#7804,#7801,#6738,.T.);
#9752=EDGE_CURVE('',#7805,#7806,#4509,.T.);
#9753=EDGE_CURVE('',#7806,#7807,#6739,.T.);
#9754=EDGE_CURVE('',#7807,#7808,#4510,.T.);
#9755=EDGE_CURVE('',#7808,#7805,#6740,.T.);
#9756=EDGE_CURVE('',#7809,#7810,#4511,.T.);
#9757=EDGE_CURVE('',#7810,#7811,#6741,.T.);
#9758=EDGE_CURVE('',#7811,#7812,#4512,.T.);
#9759=EDGE_CURVE('',#7812,#7809,#6742,.T.);
#9760=EDGE_CURVE('',#7813,#7814,#4513,.T.);
#9761=EDGE_CURVE('',#7814,#7815,#6743,.T.);
#9762=EDGE_CURVE('',#7815,#7816,#4514,.T.);
#9763=EDGE_CURVE('',#7816,#7813,#6744,.T.);
#9764=EDGE_CURVE('',#7817,#7818,#4515,.T.);
#9765=EDGE_CURVE('',#7818,#7819,#6745,.T.);
#9766=EDGE_CURVE('',#7819,#7820,#4516,.T.);
#9767=EDGE_CURVE('',#7820,#7817,#6746,.T.);
#9768=EDGE_CURVE('',#7821,#7822,#4517,.T.);
#9769=EDGE_CURVE('',#7822,#7823,#6747,.T.);
#9770=EDGE_CURVE('',#7823,#7824,#4518,.T.);
#9771=EDGE_CURVE('',#7824,#7821,#6748,.T.);
#9772=EDGE_CURVE('',#7825,#7826,#4519,.T.);
#9773=EDGE_CURVE('',#7826,#7827,#6749,.T.);
#9774=EDGE_CURVE('',#7827,#7828,#4520,.T.);
#9775=EDGE_CURVE('',#7828,#7825,#6750,.T.);
#9776=EDGE_CURVE('',#7829,#7830,#4521,.T.);
#9777=EDGE_CURVE('',#7830,#7831,#6751,.T.);
#9778=EDGE_CURVE('',#7831,#7832,#4522,.T.);
#9779=EDGE_CURVE('',#7832,#7829,#6752,.T.);
#9780=EDGE_CURVE('',#7833,#7834,#4523,.T.);
#9781=EDGE_CURVE('',#7834,#7835,#6753,.T.);
#9782=EDGE_CURVE('',#7835,#7836,#4524,.T.);
#9783=EDGE_CURVE('',#7836,#7833,#6754,.T.);
#9784=EDGE_CURVE('',#7837,#7838,#4525,.T.);
#9785=EDGE_CURVE('',#7838,#7839,#6755,.T.);
#9786=EDGE_CURVE('',#7839,#7840,#4526,.T.);
#9787=EDGE_CURVE('',#7840,#7837,#6756,.T.);
#9788=EDGE_CURVE('',#7841,#7842,#4527,.T.);
#9789=EDGE_CURVE('',#7842,#7843,#6757,.T.);
#9790=EDGE_CURVE('',#7843,#7844,#4528,.T.);
#9791=EDGE_CURVE('',#7844,#7841,#6758,.T.);
#9792=EDGE_CURVE('',#7845,#7846,#4529,.T.);
#9793=EDGE_CURVE('',#7846,#7847,#6759,.T.);
#9794=EDGE_CURVE('',#7847,#7848,#4530,.T.);
#9795=EDGE_CURVE('',#7848,#7845,#6760,.T.);
#9796=EDGE_CURVE('',#7849,#7850,#4531,.T.);
#9797=EDGE_CURVE('',#7850,#7851,#6761,.T.);
#9798=EDGE_CURVE('',#7851,#7852,#4532,.T.);
#9799=EDGE_CURVE('',#7852,#7849,#6762,.T.);
#9800=EDGE_CURVE('',#7853,#7854,#4533,.T.);
#9801=EDGE_CURVE('',#7854,#7855,#6763,.T.);
#9802=EDGE_CURVE('',#7855,#7856,#4534,.T.);
#9803=EDGE_CURVE('',#7856,#7853,#6764,.T.);
#9804=EDGE_CURVE('',#7857,#7858,#4535,.T.);
#9805=EDGE_CURVE('',#7858,#7859,#6765,.T.);
#9806=EDGE_CURVE('',#7859,#7860,#4536,.T.);
#9807=EDGE_CURVE('',#7860,#7857,#6766,.T.);
#9808=EDGE_CURVE('',#7752,#7753,#6767,.T.);
#9809=EDGE_CURVE('',#7861,#7722,#680,.T.);
#9810=EDGE_CURVE('',#7716,#7861,#681,.T.);
#9811=EDGE_CURVE('',#7862,#7692,#682,.T.);
#9812=EDGE_CURVE('',#7862,#7744,#683,.T.);
#9813=EDGE_CURVE('',#7692,#7863,#6768,.T.);
#9814=EDGE_CURVE('',#7863,#7691,#6769,.T.);
#9815=EDGE_CURVE('',#7691,#7864,#684,.T.);
#9816=EDGE_CURVE('',#7864,#7862,#6770,.T.);
#9817=EDGE_CURVE('',#7864,#7743,#685,.T.);
#9818=EDGE_CURVE('',#7719,#7865,#686,.T.);
#9819=EDGE_CURVE('',#7865,#7715,#687,.T.);
#9820=EDGE_CURVE('',#7762,#7771,#4537,.T.);
#9821=EDGE_CURVE('',#7776,#7757,#4538,.T.);
#9822=EDGE_CURVE('',#7866,#7775,#4539,.T.);
#9823=EDGE_CURVE('',#7772,#7866,#4540,.T.);
#9824=EDGE_CURVE('',#7867,#7761,#4541,.T.);
#9825=EDGE_CURVE('',#7758,#7867,#4542,.T.);
#9826=EDGE_CURVE('',#7868,#7760,#4543,.T.);
#9827=EDGE_CURVE('',#7868,#7867,#4544,.T.);
#9828=EDGE_CURVE('',#7859,#7869,#4545,.T.);
#9829=EDGE_CURVE('',#7870,#7869,#4546,.T.);
#9830=EDGE_CURVE('',#7860,#7870,#4547,.T.);
#9831=EDGE_CURVE('',#7870,#7857,#4548,.T.);
#9832=EDGE_CURVE('',#7869,#7858,#4549,.T.);
#9833=EDGE_CURVE('',#7855,#7871,#4550,.T.);
#9834=EDGE_CURVE('',#7872,#7871,#4551,.T.);
#9835=EDGE_CURVE('',#7856,#7872,#4552,.T.);
#9836=EDGE_CURVE('',#7872,#7853,#4553,.T.);
#9837=EDGE_CURVE('',#7871,#7854,#4554,.T.);
#9838=EDGE_CURVE('',#7851,#7873,#4555,.T.);
#9839=EDGE_CURVE('',#7874,#7873,#4556,.T.);
#9840=EDGE_CURVE('',#7852,#7874,#4557,.T.);
#9841=EDGE_CURVE('',#7874,#7849,#4558,.T.);
#9842=EDGE_CURVE('',#7873,#7850,#4559,.T.);
#9843=EDGE_CURVE('',#7847,#7875,#4560,.T.);
#9844=EDGE_CURVE('',#7876,#7875,#4561,.T.);
#9845=EDGE_CURVE('',#7848,#7876,#4562,.T.);
#9846=EDGE_CURVE('',#7876,#7845,#4563,.T.);
#9847=EDGE_CURVE('',#7875,#7846,#4564,.T.);
#9848=EDGE_CURVE('',#7843,#7877,#4565,.T.);
#9849=EDGE_CURVE('',#7878,#7877,#4566,.T.);
#9850=EDGE_CURVE('',#7844,#7878,#4567,.T.);
#9851=EDGE_CURVE('',#7878,#7841,#4568,.T.);
#9852=EDGE_CURVE('',#7877,#7842,#4569,.T.);
#9853=EDGE_CURVE('',#7759,#7868,#4570,.T.);
#9854=EDGE_CURVE('',#7839,#7879,#4571,.T.);
#9855=EDGE_CURVE('',#7880,#7879,#4572,.T.);
#9856=EDGE_CURVE('',#7840,#7880,#4573,.T.);
#9857=EDGE_CURVE('',#7880,#7837,#4574,.T.);
#9858=EDGE_CURVE('',#7879,#7838,#4575,.T.);
#9859=EDGE_CURVE('',#7835,#7881,#4576,.T.);
#9860=EDGE_CURVE('',#7882,#7881,#4577,.T.);
#9861=EDGE_CURVE('',#7836,#7882,#4578,.T.);
#9862=EDGE_CURVE('',#7882,#7833,#4579,.T.);
#9863=EDGE_CURVE('',#7881,#7834,#4580,.T.);
#9864=EDGE_CURVE('',#7831,#7883,#4581,.T.);
#9865=EDGE_CURVE('',#7884,#7883,#4582,.T.);
#9866=EDGE_CURVE('',#7832,#7884,#4583,.T.);
#9867=EDGE_CURVE('',#7884,#7829,#4584,.T.);
#9868=EDGE_CURVE('',#7883,#7830,#4585,.T.);
#9869=EDGE_CURVE('',#7827,#7885,#4586,.T.);
#9870=EDGE_CURVE('',#7886,#7885,#4587,.T.);
#9871=EDGE_CURVE('',#7828,#7886,#4588,.T.);
#9872=EDGE_CURVE('',#7886,#7825,#4589,.T.);
#9873=EDGE_CURVE('',#7885,#7826,#4590,.T.);
#9874=EDGE_CURVE('',#7823,#7887,#4591,.T.);
#9875=EDGE_CURVE('',#7888,#7887,#4592,.T.);
#9876=EDGE_CURVE('',#7824,#7888,#4593,.T.);
#9877=EDGE_CURVE('',#7888,#7821,#4594,.T.);
#9878=EDGE_CURVE('',#7887,#7822,#4595,.T.);
#9879=EDGE_CURVE('',#7765,#7889,#4596,.T.);
#9880=EDGE_CURVE('',#7890,#7889,#4597,.T.);
#9881=EDGE_CURVE('',#7766,#7890,#4598,.T.);
#9882=EDGE_CURVE('',#7890,#7769,#4599,.T.);
#9883=EDGE_CURVE('',#7889,#7770,#4600,.T.);
#9884=EDGE_CURVE('',#7819,#7891,#4601,.T.);
#9885=EDGE_CURVE('',#7892,#7891,#4602,.T.);
#9886=EDGE_CURVE('',#7820,#7892,#4603,.T.);
#9887=EDGE_CURVE('',#7892,#7817,#4604,.T.);
#9888=EDGE_CURVE('',#7891,#7818,#4605,.T.);
#9889=EDGE_CURVE('',#7815,#7893,#4606,.T.);
#9890=EDGE_CURVE('',#7894,#7893,#4607,.T.);
#9891=EDGE_CURVE('',#7816,#7894,#4608,.T.);
#9892=EDGE_CURVE('',#7894,#7813,#4609,.T.);
#9893=EDGE_CURVE('',#7893,#7814,#4610,.T.);
#9894=EDGE_CURVE('',#7811,#7895,#4611,.T.);
#9895=EDGE_CURVE('',#7896,#7895,#4612,.T.);
#9896=EDGE_CURVE('',#7812,#7896,#4613,.T.);
#9897=EDGE_CURVE('',#7896,#7809,#4614,.T.);
#9898=EDGE_CURVE('',#7895,#7810,#4615,.T.);
#9899=EDGE_CURVE('',#7807,#7897,#4616,.T.);
#9900=EDGE_CURVE('',#7898,#7897,#4617,.T.);
#9901=EDGE_CURVE('',#7808,#7898,#4618,.T.);
#9902=EDGE_CURVE('',#7898,#7805,#4619,.T.);
#9903=EDGE_CURVE('',#7897,#7806,#4620,.T.);
#9904=EDGE_CURVE('',#7803,#7899,#4621,.T.);
#9905=EDGE_CURVE('',#7900,#7899,#4622,.T.);
#9906=EDGE_CURVE('',#7804,#7900,#4623,.T.);
#9907=EDGE_CURVE('',#7900,#7801,#4624,.T.);
#9908=EDGE_CURVE('',#7899,#7802,#4625,.T.);
#9909=EDGE_CURVE('',#7901,#7866,#4626,.T.);
#9910=EDGE_CURVE('',#7773,#7901,#4627,.T.);
#9911=EDGE_CURVE('',#7901,#7774,#4628,.T.);
#9912=EDGE_CURVE('',#7799,#7902,#4629,.T.);
#9913=EDGE_CURVE('',#7903,#7902,#4630,.T.);
#9914=EDGE_CURVE('',#7800,#7903,#4631,.T.);
#9915=EDGE_CURVE('',#7903,#7797,#4632,.T.);
#9916=EDGE_CURVE('',#7902,#7798,#4633,.T.);
#9917=EDGE_CURVE('',#7795,#7904,#4634,.T.);
#9918=EDGE_CURVE('',#7905,#7904,#4635,.T.);
#9919=EDGE_CURVE('',#7796,#7905,#4636,.T.);
#9920=EDGE_CURVE('',#7905,#7793,#4637,.T.);
#9921=EDGE_CURVE('',#7904,#7794,#4638,.T.);
#9922=EDGE_CURVE('',#7791,#7906,#4639,.T.);
#9923=EDGE_CURVE('',#7907,#7906,#4640,.T.);
#9924=EDGE_CURVE('',#7792,#7907,#4641,.T.);
#9925=EDGE_CURVE('',#7907,#7789,#4642,.T.);
#9926=EDGE_CURVE('',#7906,#7790,#4643,.T.);
#9927=EDGE_CURVE('',#7787,#7908,#4644,.T.);
#9928=EDGE_CURVE('',#7909,#7908,#4645,.T.);
#9929=EDGE_CURVE('',#7788,#7909,#4646,.T.);
#9930=EDGE_CURVE('',#7909,#7785,#4647,.T.);
#9931=EDGE_CURVE('',#7908,#7786,#4648,.T.);
#9932=EDGE_CURVE('',#7783,#7910,#4649,.T.);
#9933=EDGE_CURVE('',#7911,#7910,#4650,.T.);
#9934=EDGE_CURVE('',#7784,#7911,#4651,.T.);
#9935=EDGE_CURVE('',#7911,#7781,#4652,.T.);
#9936=EDGE_CURVE('',#7910,#7782,#4653,.T.);
#9937=EDGE_CURVE('',#7779,#7912,#4654,.T.);
#9938=EDGE_CURVE('',#7913,#7912,#4655,.T.);
#9939=EDGE_CURVE('',#7780,#7913,#4656,.T.);
#9940=EDGE_CURVE('',#7913,#7777,#4657,.T.);
#9941=EDGE_CURVE('',#7912,#7778,#4658,.T.);
#9942=EDGE_CURVE('',#7914,#7914,#6771,.T.);
#9943=EDGE_CURVE('',#7863,#7914,#4659,.T.);
#9944=EDGE_CURVE('',#7865,#7861,#6772,.T.);
#9945=EDGE_CURVE('',#7915,#7915,#6773,.T.);
#9946=EDGE_CURVE('',#7768,#7915,#4660,.T.);
#9947=EDGE_CURVE('',#7916,#7916,#6774,.T.);
#9948=EDGE_CURVE('',#7916,#7917,#4661,.T.);
#9949=EDGE_CURVE('',#7917,#7918,#6775,.T.);
#9950=EDGE_CURVE('',#7918,#7917,#6776,.T.);
#9951=EDGE_CURVE('',#7919,#7919,#6777,.T.);
#9952=EDGE_CURVE('',#7919,#7918,#4662,.T.);
#9953=EDGE_CURVE('',#7920,#7920,#6778,.T.);
#9954=EDGE_CURVE('',#7920,#7921,#4663,.T.);
#9955=EDGE_CURVE('',#7921,#7921,#6779,.T.);
#9956=EDGE_CURVE('',#7922,#7922,#6780,.T.);
#9957=EDGE_CURVE('',#7923,#7923,#6781,.T.);
#9958=EDGE_CURVE('',#7923,#7922,#4664,.T.);
#9959=EDGE_CURVE('',#7924,#7924,#6782,.T.);
#9960=EDGE_CURVE('',#7924,#7923,#4665,.T.);
#9961=EDGE_CURVE('',#7925,#7925,#6783,.T.);
#9962=EDGE_CURVE('',#7925,#7924,#4666,.T.);
#9963=EDGE_CURVE('',#7926,#7926,#6784,.T.);
#9964=EDGE_CURVE('',#7926,#7927,#4667,.T.);
#9965=EDGE_CURVE('',#7927,#7928,#6785,.T.);
#9966=EDGE_CURVE('',#7928,#7927,#6786,.T.);
#9967=EDGE_CURVE('',#7928,#7929,#4668,.T.);
#9968=EDGE_CURVE('',#7930,#7929,#6787,.T.);
#9969=EDGE_CURVE('',#7929,#7930,#6788,.T.);
#9970=EDGE_CURVE('',#7930,#7931,#4669,.T.);
#9971=EDGE_CURVE('',#7931,#7932,#6789,.T.);
#9972=EDGE_CURVE('',#7932,#7931,#6790,.T.);
#9973=EDGE_CURVE('',#7932,#7933,#4670,.T.);
#9974=EDGE_CURVE('',#7934,#7933,#6791,.T.);
#9975=EDGE_CURVE('',#7933,#7934,#6792,.T.);
#9976=EDGE_CURVE('',#7934,#7935,#4671,.T.);
#9977=EDGE_CURVE('',#7935,#7936,#6793,.T.);
#9978=EDGE_CURVE('',#7936,#7935,#6794,.T.);
#9979=EDGE_CURVE('',#7936,#7937,#4672,.T.);
#9980=EDGE_CURVE('',#7937,#7937,#6795,.T.);
#9981=EDGE_CURVE('',#7938,#7938,#6796,.T.);
#9982=EDGE_CURVE('',#7938,#7939,#4673,.T.);
#9983=EDGE_CURVE('',#7939,#7939,#6797,.T.);
#9984=EDGE_CURVE('',#7940,#7940,#6798,.T.);
#9985=EDGE_CURVE('',#7937,#7940,#4674,.T.);
#9986=EDGE_CURVE('',#7941,#7941,#6799,.T.);
#9987=EDGE_CURVE('',#7941,#7938,#4675,.T.);
#9988=EDGE_CURVE('',#7942,#7943,#4676,.T.);
#9989=EDGE_CURVE('',#7942,#7944,#688,.T.);
#9990=EDGE_CURVE('',#7944,#7945,#6800,.T.);
#9991=EDGE_CURVE('',#7945,#7943,#689,.T.);
#9992=EDGE_CURVE('',#7946,#7947,#4677,.T.);
#9993=EDGE_CURVE('',#7946,#7942,#690,.T.);
#9994=EDGE_CURVE('',#7943,#7947,#691,.T.);
#9995=EDGE_CURVE('',#7948,#7949,#4678,.T.);
#9996=EDGE_CURVE('',#7948,#7946,#692,.T.);
#9997=EDGE_CURVE('',#7947,#7949,#693,.T.);
#9998=EDGE_CURVE('',#7950,#7951,#4679,.T.);
#9999=EDGE_CURVE('',#7950,#7948,#694,.T.);
#10000=EDGE_CURVE('',#7949,#7951,#695,.T.);
#10001=EDGE_CURVE('',#7952,#7953,#4680,.T.);
#10002=EDGE_CURVE('',#7952,#7950,#696,.T.);
#10003=EDGE_CURVE('',#7951,#7953,#697,.T.);
#10004=EDGE_CURVE('',#7954,#7955,#4681,.T.);
#10005=EDGE_CURVE('',#7954,#7952,#698,.T.);
#10006=EDGE_CURVE('',#7953,#7955,#699,.T.);
#10007=EDGE_CURVE('',#7956,#7957,#4682,.T.);
#10008=EDGE_CURVE('',#7956,#7954,#700,.T.);
#10009=EDGE_CURVE('',#7955,#7957,#701,.T.);
#10010=EDGE_CURVE('',#7958,#7959,#4683,.T.);
#10011=EDGE_CURVE('',#7958,#7956,#702,.T.);
#10012=EDGE_CURVE('',#7957,#7959,#703,.T.);
#10013=EDGE_CURVE('',#7960,#7961,#4684,.T.);
#10014=EDGE_CURVE('',#7960,#7958,#704,.T.);
#10015=EDGE_CURVE('',#7959,#7961,#705,.T.);
#10016=EDGE_CURVE('',#7962,#7963,#4685,.T.);
#10017=EDGE_CURVE('',#7962,#7960,#706,.T.);
#10018=EDGE_CURVE('',#7961,#7963,#707,.T.);
#10019=EDGE_CURVE('',#7964,#7965,#4686,.T.);
#10020=EDGE_CURVE('',#7964,#7962,#708,.T.);
#10021=EDGE_CURVE('',#7963,#7965,#709,.T.);
#10022=EDGE_CURVE('',#7966,#7967,#4687,.T.);
#10023=EDGE_CURVE('',#7966,#7964,#710,.T.);
#10024=EDGE_CURVE('',#7965,#7967,#711,.T.);
#10025=EDGE_CURVE('',#7968,#7969,#4688,.T.);
#10026=EDGE_CURVE('',#7968,#7966,#712,.T.);
#10027=EDGE_CURVE('',#7967,#7969,#713,.T.);
#10028=EDGE_CURVE('',#7970,#7971,#4689,.T.);
#10029=EDGE_CURVE('',#7970,#7972,#714,.T.);
#10030=EDGE_CURVE('',#7973,#7972,#6801,.T.);
#10031=EDGE_CURVE('',#7971,#7973,#715,.T.);
#10032=EDGE_CURVE('',#7974,#7975,#4690,.T.);
#10033=EDGE_CURVE('',#7974,#7970,#716,.T.);
#10034=EDGE_CURVE('',#7975,#7971,#717,.T.);
#10035=EDGE_CURVE('',#7976,#7977,#4691,.T.);
#10036=EDGE_CURVE('',#7976,#7974,#718,.T.);
#10037=EDGE_CURVE('',#7977,#7975,#719,.T.);
#10038=EDGE_CURVE('',#7978,#7979,#4692,.T.);
#10039=EDGE_CURVE('',#7978,#7976,#720,.T.);
#10040=EDGE_CURVE('',#7979,#7977,#721,.T.);
#10041=EDGE_CURVE('',#7980,#7981,#4693,.T.);
#10042=EDGE_CURVE('',#7980,#7978,#722,.T.);
#10043=EDGE_CURVE('',#7981,#7979,#723,.T.);
#10044=EDGE_CURVE('',#7982,#7983,#4694,.T.);
#10045=EDGE_CURVE('',#7982,#7980,#724,.T.);
#10046=EDGE_CURVE('',#7983,#7981,#725,.T.);
#10047=EDGE_CURVE('',#7984,#7985,#4695,.T.);
#10048=EDGE_CURVE('',#7984,#7982,#726,.T.);
#10049=EDGE_CURVE('',#7985,#7983,#727,.T.);
#10050=EDGE_CURVE('',#7986,#7987,#4696,.T.);
#10051=EDGE_CURVE('',#7986,#7984,#728,.T.);
#10052=EDGE_CURVE('',#7987,#7985,#729,.T.);
#10053=EDGE_CURVE('',#7988,#7989,#4697,.T.);
#10054=EDGE_CURVE('',#7988,#7986,#730,.T.);
#10055=EDGE_CURVE('',#7989,#7987,#731,.T.);
#10056=EDGE_CURVE('',#7990,#7991,#4698,.T.);
#10057=EDGE_CURVE('',#7990,#7988,#732,.T.);
#10058=EDGE_CURVE('',#7991,#7989,#733,.T.);
#10059=EDGE_CURVE('',#7992,#7993,#4699,.T.);
#10060=EDGE_CURVE('',#7992,#7990,#734,.T.);
#10061=EDGE_CURVE('',#7993,#7991,#735,.T.);
#10062=EDGE_CURVE('',#7994,#7995,#4700,.T.);
#10063=EDGE_CURVE('',#7994,#7992,#736,.T.);
#10064=EDGE_CURVE('',#7995,#7993,#737,.T.);
#10065=EDGE_CURVE('',#7996,#7973,#738,.T.);
#10066=EDGE_CURVE('',#7969,#7996,#739,.T.);
#10067=EDGE_CURVE('',#7997,#7945,#740,.T.);
#10068=EDGE_CURVE('',#7997,#7995,#741,.T.);
#10069=EDGE_CURVE('',#7945,#7998,#6802,.T.);
#10070=EDGE_CURVE('',#7998,#7944,#6803,.T.);
#10071=EDGE_CURVE('',#7944,#7999,#742,.T.);
#10072=EDGE_CURVE('',#7999,#7997,#6804,.T.);
#10073=EDGE_CURVE('',#7999,#7994,#743,.T.);
#10074=EDGE_CURVE('',#7972,#8000,#744,.T.);
#10075=EDGE_CURVE('',#8000,#7968,#745,.T.);
#10076=EDGE_CURVE('',#8000,#7996,#6805,.F.);
#10077=EDGE_CURVE('',#8001,#8001,#6806,.T.);
#10078=EDGE_CURVE('',#8002,#8003,#746,.T.);
#10079=EDGE_CURVE('',#8002,#8004,#4701,.T.);
#10080=EDGE_CURVE('',#8004,#8005,#747,.T.);
#10081=EDGE_CURVE('',#8003,#8005,#4702,.T.);
#10082=EDGE_CURVE('',#8006,#8002,#748,.T.);
#10083=EDGE_CURVE('',#8006,#8007,#4703,.T.);
#10084=EDGE_CURVE('',#8007,#8004,#749,.T.);
#10085=EDGE_CURVE('',#8008,#8006,#750,.T.);
#10086=EDGE_CURVE('',#8008,#8009,#4704,.T.);
#10087=EDGE_CURVE('',#8009,#8007,#751,.T.);
#10088=EDGE_CURVE('',#8010,#8008,#752,.T.);
#10089=EDGE_CURVE('',#8010,#8011,#4705,.T.);
#10090=EDGE_CURVE('',#8011,#8009,#753,.T.);
#10091=EDGE_CURVE('',#8012,#8010,#754,.T.);
#10092=EDGE_CURVE('',#8012,#8013,#4706,.T.);
#10093=EDGE_CURVE('',#8013,#8011,#755,.T.);
#10094=EDGE_CURVE('',#8014,#8012,#756,.T.);
#10095=EDGE_CURVE('',#8014,#8015,#4707,.T.);
#10096=EDGE_CURVE('',#8015,#8013,#757,.T.);
#10097=EDGE_CURVE('',#8016,#8014,#758,.T.);
#10098=EDGE_CURVE('',#8016,#8017,#4708,.T.);
#10099=EDGE_CURVE('',#8017,#8015,#759,.T.);
#10100=EDGE_CURVE('',#8018,#8016,#760,.T.);
#10101=EDGE_CURVE('',#8018,#8019,#4709,.T.);
#10102=EDGE_CURVE('',#8019,#8017,#761,.T.);
#10103=EDGE_CURVE('',#8020,#8018,#762,.T.);
#10104=EDGE_CURVE('',#8020,#8021,#4710,.T.);
#10105=EDGE_CURVE('',#8021,#8019,#763,.T.);
#10106=EDGE_CURVE('',#8022,#8020,#764,.T.);
#10107=EDGE_CURVE('',#8022,#8023,#4711,.T.);
#10108=EDGE_CURVE('',#8023,#8021,#765,.T.);
#10109=EDGE_CURVE('',#8003,#8022,#766,.T.);
#10110=EDGE_CURVE('',#8005,#8023,#767,.T.);
#10111=EDGE_CURVE('',#8024,#8025,#4712,.T.);
#10112=EDGE_CURVE('',#8024,#8026,#4713,.T.);
#10113=EDGE_CURVE('',#8026,#8027,#4714,.T.);
#10114=EDGE_CURVE('',#8025,#8027,#4715,.T.);
#10115=EDGE_CURVE('',#8028,#8024,#4716,.T.);
#10116=EDGE_CURVE('',#8028,#8029,#4717,.T.);
#10117=EDGE_CURVE('',#8029,#8026,#4718,.T.);
#10118=EDGE_CURVE('',#8030,#8028,#4719,.T.);
#10119=EDGE_CURVE('',#8030,#8031,#4720,.T.);
#10120=EDGE_CURVE('',#8031,#8029,#4721,.T.);
#10121=EDGE_CURVE('',#8032,#8030,#4722,.T.);
#10122=EDGE_CURVE('',#8032,#8033,#4723,.T.);
#10123=EDGE_CURVE('',#8033,#8031,#4724,.T.);
#10124=EDGE_CURVE('',#8034,#8032,#4725,.T.);
#10125=EDGE_CURVE('',#8034,#8035,#4726,.T.);
#10126=EDGE_CURVE('',#8035,#8033,#4727,.T.);
#10127=EDGE_CURVE('',#8036,#8034,#4728,.T.);
#10128=EDGE_CURVE('',#8036,#8037,#4729,.T.);
#10129=EDGE_CURVE('',#8037,#8035,#4730,.T.);
#10130=EDGE_CURVE('',#8038,#8036,#4731,.T.);
#10131=EDGE_CURVE('',#8038,#8039,#4732,.T.);
#10132=EDGE_CURVE('',#8039,#8037,#4733,.T.);
#10133=EDGE_CURVE('',#8040,#8038,#4734,.T.);
#10134=EDGE_CURVE('',#8040,#8041,#4735,.T.);
#10135=EDGE_CURVE('',#8041,#8039,#4736,.T.);
#10136=EDGE_CURVE('',#8042,#8040,#4737,.T.);
#10137=EDGE_CURVE('',#8042,#8043,#4738,.T.);
#10138=EDGE_CURVE('',#8043,#8041,#4739,.T.);
#10139=EDGE_CURVE('',#8025,#8042,#4740,.T.);
#10140=EDGE_CURVE('',#8027,#8043,#4741,.T.);
#10141=EDGE_CURVE('',#8044,#8045,#768,.T.);
#10142=EDGE_CURVE('',#8044,#8046,#4742,.T.);
#10143=EDGE_CURVE('',#8046,#8047,#769,.T.);
#10144=EDGE_CURVE('',#8045,#8047,#4743,.T.);
#10145=EDGE_CURVE('',#8048,#8044,#770,.T.);
#10146=EDGE_CURVE('',#8048,#8049,#4744,.T.);
#10147=EDGE_CURVE('',#8049,#8046,#771,.T.);
#10148=EDGE_CURVE('',#8050,#8048,#772,.T.);
#10149=EDGE_CURVE('',#8050,#8051,#4745,.T.);
#10150=EDGE_CURVE('',#8051,#8049,#773,.T.);
#10151=EDGE_CURVE('',#8052,#8050,#774,.T.);
#10152=EDGE_CURVE('',#8052,#8053,#4746,.T.);
#10153=EDGE_CURVE('',#8053,#8051,#775,.T.);
#10154=EDGE_CURVE('',#8054,#8052,#776,.T.);
#10155=EDGE_CURVE('',#8054,#8055,#4747,.T.);
#10156=EDGE_CURVE('',#8055,#8053,#777,.T.);
#10157=EDGE_CURVE('',#8056,#8054,#778,.T.);
#10158=EDGE_CURVE('',#8056,#8057,#4748,.T.);
#10159=EDGE_CURVE('',#8057,#8055,#779,.T.);
#10160=EDGE_CURVE('',#8058,#8056,#780,.T.);
#10161=EDGE_CURVE('',#8058,#8059,#4749,.T.);
#10162=EDGE_CURVE('',#8059,#8057,#781,.T.);
#10163=EDGE_CURVE('',#8060,#8058,#782,.T.);
#10164=EDGE_CURVE('',#8060,#8061,#4750,.T.);
#10165=EDGE_CURVE('',#8061,#8059,#783,.T.);
#10166=EDGE_CURVE('',#8062,#8060,#784,.T.);
#10167=EDGE_CURVE('',#8062,#8063,#4751,.T.);
#10168=EDGE_CURVE('',#8063,#8061,#785,.T.);
#10169=EDGE_CURVE('',#8064,#8062,#786,.T.);
#10170=EDGE_CURVE('',#8064,#8065,#4752,.T.);
#10171=EDGE_CURVE('',#8065,#8063,#787,.T.);
#10172=EDGE_CURVE('',#8045,#8064,#788,.T.);
#10173=EDGE_CURVE('',#8047,#8065,#789,.T.);
#10174=EDGE_CURVE('',#8066,#8067,#4753,.T.);
#10175=EDGE_CURVE('',#8066,#8068,#4754,.T.);
#10176=EDGE_CURVE('',#8068,#8069,#4755,.T.);
#10177=EDGE_CURVE('',#8067,#8069,#4756,.T.);
#10178=EDGE_CURVE('',#8070,#8066,#4757,.T.);
#10179=EDGE_CURVE('',#8070,#8071,#4758,.T.);
#10180=EDGE_CURVE('',#8071,#8068,#4759,.T.);
#10181=EDGE_CURVE('',#8072,#8070,#4760,.T.);
#10182=EDGE_CURVE('',#8072,#8073,#4761,.T.);
#10183=EDGE_CURVE('',#8073,#8071,#4762,.T.);
#10184=EDGE_CURVE('',#8074,#8072,#4763,.T.);
#10185=EDGE_CURVE('',#8074,#8075,#4764,.T.);
#10186=EDGE_CURVE('',#8075,#8073,#4765,.T.);
#10187=EDGE_CURVE('',#8076,#8074,#4766,.T.);
#10188=EDGE_CURVE('',#8076,#8077,#4767,.T.);
#10189=EDGE_CURVE('',#8077,#8075,#4768,.T.);
#10190=EDGE_CURVE('',#8078,#8076,#4769,.T.);
#10191=EDGE_CURVE('',#8078,#8079,#4770,.T.);
#10192=EDGE_CURVE('',#8079,#8077,#4771,.T.);
#10193=EDGE_CURVE('',#8080,#8078,#4772,.T.);
#10194=EDGE_CURVE('',#8080,#8081,#4773,.T.);
#10195=EDGE_CURVE('',#8081,#8079,#4774,.T.);
#10196=EDGE_CURVE('',#8082,#8080,#4775,.T.);
#10197=EDGE_CURVE('',#8082,#8083,#4776,.T.);
#10198=EDGE_CURVE('',#8083,#8081,#4777,.T.);
#10199=EDGE_CURVE('',#8084,#8082,#4778,.T.);
#10200=EDGE_CURVE('',#8084,#8085,#4779,.T.);
#10201=EDGE_CURVE('',#8085,#8083,#4780,.T.);
#10202=EDGE_CURVE('',#8067,#8084,#4781,.T.);
#10203=EDGE_CURVE('',#8069,#8085,#4782,.T.);
#10204=EDGE_CURVE('',#8086,#8087,#4783,.T.);
#10205=EDGE_CURVE('',#8086,#8088,#4784,.T.);
#10206=EDGE_CURVE('',#8088,#8089,#4785,.T.);
#10207=EDGE_CURVE('',#8087,#8089,#4786,.T.);
#10208=EDGE_CURVE('',#8090,#8086,#4787,.T.);
#10209=EDGE_CURVE('',#8090,#8091,#4788,.T.);
#10210=EDGE_CURVE('',#8091,#8088,#4789,.T.);
#10211=EDGE_CURVE('',#8092,#8090,#4790,.T.);
#10212=EDGE_CURVE('',#8092,#8093,#4791,.T.);
#10213=EDGE_CURVE('',#8093,#8091,#4792,.T.);
#10214=EDGE_CURVE('',#8094,#8092,#4793,.T.);
#10215=EDGE_CURVE('',#8094,#8095,#4794,.T.);
#10216=EDGE_CURVE('',#8095,#8093,#4795,.T.);
#10217=EDGE_CURVE('',#8096,#8094,#4796,.T.);
#10218=EDGE_CURVE('',#8096,#8097,#4797,.T.);
#10219=EDGE_CURVE('',#8097,#8095,#4798,.T.);
#10220=EDGE_CURVE('',#8098,#8096,#4799,.T.);
#10221=EDGE_CURVE('',#8098,#8099,#4800,.T.);
#10222=EDGE_CURVE('',#8099,#8097,#4801,.T.);
#10223=EDGE_CURVE('',#8100,#8098,#4802,.T.);
#10224=EDGE_CURVE('',#8100,#8101,#4803,.T.);
#10225=EDGE_CURVE('',#8101,#8099,#4804,.T.);
#10226=EDGE_CURVE('',#8102,#8100,#4805,.T.);
#10227=EDGE_CURVE('',#8102,#8103,#4806,.T.);
#10228=EDGE_CURVE('',#8103,#8101,#4807,.T.);
#10229=EDGE_CURVE('',#8104,#8102,#4808,.T.);
#10230=EDGE_CURVE('',#8104,#8105,#4809,.T.);
#10231=EDGE_CURVE('',#8105,#8103,#4810,.T.);
#10232=EDGE_CURVE('',#8087,#8104,#4811,.T.);
#10233=EDGE_CURVE('',#8089,#8105,#4812,.T.);
#10234=EDGE_CURVE('',#8106,#8106,#6807,.T.);
#10235=EDGE_CURVE('',#8107,#8107,#6808,.T.);
#10236=EDGE_CURVE('',#8106,#8108,#4813,.T.);
#10237=EDGE_CURVE('',#8108,#8108,#6809,.T.);
#10238=EDGE_CURVE('',#8107,#8109,#4814,.T.);
#10239=EDGE_CURVE('',#8109,#8109,#6810,.T.);
#10240=EDGE_CURVE('',#8110,#8111,#4815,.T.);
#10241=EDGE_CURVE('',#8110,#8112,#4816,.T.);
#10242=EDGE_CURVE('',#8113,#8112,#4817,.T.);
#10243=EDGE_CURVE('',#8111,#8113,#4818,.T.);
#10244=EDGE_CURVE('',#8111,#8114,#6811,.T.);
#10245=EDGE_CURVE('',#8113,#8114,#4819,.T.);
#10246=EDGE_CURVE('',#8114,#8115,#4820,.T.);
#10247=EDGE_CURVE('',#8112,#8115,#4821,.T.);
#10248=EDGE_CURVE('',#8115,#8110,#6812,.T.);
#10249=EDGE_CURVE('',#8116,#8117,#4822,.T.);
#10250=EDGE_CURVE('',#8116,#8118,#4823,.T.);
#10251=EDGE_CURVE('',#8119,#8118,#4824,.T.);
#10252=EDGE_CURVE('',#8117,#8119,#4825,.T.);
#10253=EDGE_CURVE('',#8117,#8120,#6813,.T.);
#10254=EDGE_CURVE('',#8119,#8120,#4826,.T.);
#10255=EDGE_CURVE('',#8120,#8121,#4827,.T.);
#10256=EDGE_CURVE('',#8118,#8121,#4828,.T.);
#10257=EDGE_CURVE('',#8121,#8116,#6814,.T.);
#10258=EDGE_CURVE('',#8122,#8123,#4829,.T.);
#10259=EDGE_CURVE('',#8122,#8124,#4830,.T.);
#10260=EDGE_CURVE('',#8125,#8124,#4831,.T.);
#10261=EDGE_CURVE('',#8123,#8125,#4832,.T.);
#10262=EDGE_CURVE('',#8123,#8126,#6815,.T.);
#10263=EDGE_CURVE('',#8125,#8126,#4833,.T.);
#10264=EDGE_CURVE('',#8126,#8127,#4834,.T.);
#10265=EDGE_CURVE('',#8124,#8127,#4835,.T.);
#10266=EDGE_CURVE('',#8127,#8122,#6816,.T.);
#10267=EDGE_CURVE('',#8128,#8129,#4836,.T.);
#10268=EDGE_CURVE('',#8128,#8130,#4837,.T.);
#10269=EDGE_CURVE('',#8131,#8130,#4838,.T.);
#10270=EDGE_CURVE('',#8129,#8131,#4839,.T.);
#10271=EDGE_CURVE('',#8129,#8132,#6817,.T.);
#10272=EDGE_CURVE('',#8131,#8132,#4840,.T.);
#10273=EDGE_CURVE('',#8132,#8133,#4841,.T.);
#10274=EDGE_CURVE('',#8130,#8133,#4842,.T.);
#10275=EDGE_CURVE('',#8133,#8128,#6818,.T.);
#10276=EDGE_CURVE('',#8134,#8135,#4843,.T.);
#10277=EDGE_CURVE('',#8134,#8136,#4844,.T.);
#10278=EDGE_CURVE('',#8137,#8136,#4845,.T.);
#10279=EDGE_CURVE('',#8135,#8137,#4846,.T.);
#10280=EDGE_CURVE('',#8135,#8138,#6819,.T.);
#10281=EDGE_CURVE('',#8137,#8138,#4847,.T.);
#10282=EDGE_CURVE('',#8138,#8139,#4848,.T.);
#10283=EDGE_CURVE('',#8136,#8139,#4849,.T.);
#10284=EDGE_CURVE('',#8139,#8134,#6820,.T.);
#10285=EDGE_CURVE('',#8140,#8141,#4850,.T.);
#10286=EDGE_CURVE('',#8140,#8142,#4851,.T.);
#10287=EDGE_CURVE('',#8143,#8142,#4852,.T.);
#10288=EDGE_CURVE('',#8141,#8143,#4853,.T.);
#10289=EDGE_CURVE('',#8141,#8144,#6821,.T.);
#10290=EDGE_CURVE('',#8143,#8144,#4854,.T.);
#10291=EDGE_CURVE('',#8144,#8145,#4855,.T.);
#10292=EDGE_CURVE('',#8142,#8145,#4856,.T.);
#10293=EDGE_CURVE('',#8145,#8140,#6822,.T.);
#10294=EDGE_CURVE('',#8146,#8147,#4857,.T.);
#10295=EDGE_CURVE('',#8146,#8148,#4858,.T.);
#10296=EDGE_CURVE('',#8149,#8148,#4859,.T.);
#10297=EDGE_CURVE('',#8147,#8149,#4860,.T.);
#10298=EDGE_CURVE('',#8147,#8150,#6823,.T.);
#10299=EDGE_CURVE('',#8149,#8150,#4861,.T.);
#10300=EDGE_CURVE('',#8150,#8151,#4862,.T.);
#10301=EDGE_CURVE('',#8148,#8151,#4863,.T.);
#10302=EDGE_CURVE('',#8151,#8146,#6824,.T.);
#10303=EDGE_CURVE('',#8152,#8153,#4864,.T.);
#10304=EDGE_CURVE('',#8152,#8154,#4865,.T.);
#10305=EDGE_CURVE('',#8155,#8154,#4866,.T.);
#10306=EDGE_CURVE('',#8153,#8155,#4867,.T.);
#10307=EDGE_CURVE('',#8153,#8156,#6825,.T.);
#10308=EDGE_CURVE('',#8155,#8156,#4868,.T.);
#10309=EDGE_CURVE('',#8156,#8157,#4869,.T.);
#10310=EDGE_CURVE('',#8154,#8157,#4870,.T.);
#10311=EDGE_CURVE('',#8157,#8152,#6826,.T.);
#10312=EDGE_CURVE('',#8158,#8159,#4871,.T.);
#10313=EDGE_CURVE('',#8158,#8160,#4872,.T.);
#10314=EDGE_CURVE('',#8161,#8160,#4873,.T.);
#10315=EDGE_CURVE('',#8159,#8161,#4874,.T.);
#10316=EDGE_CURVE('',#8159,#8162,#6827,.T.);
#10317=EDGE_CURVE('',#8161,#8162,#4875,.T.);
#10318=EDGE_CURVE('',#8162,#8163,#4876,.T.);
#10319=EDGE_CURVE('',#8160,#8163,#4877,.T.);
#10320=EDGE_CURVE('',#8163,#8158,#6828,.T.);
#10321=EDGE_CURVE('',#8164,#8165,#4878,.T.);
#10322=EDGE_CURVE('',#8164,#8166,#4879,.T.);
#10323=EDGE_CURVE('',#8167,#8166,#4880,.T.);
#10324=EDGE_CURVE('',#8165,#8167,#4881,.T.);
#10325=EDGE_CURVE('',#8165,#8168,#6829,.T.);
#10326=EDGE_CURVE('',#8167,#8168,#4882,.T.);
#10327=EDGE_CURVE('',#8168,#8169,#4883,.T.);
#10328=EDGE_CURVE('',#8166,#8169,#4884,.T.);
#10329=EDGE_CURVE('',#8169,#8164,#6830,.T.);
#10330=EDGE_CURVE('',#8170,#8171,#4885,.T.);
#10331=EDGE_CURVE('',#8170,#8172,#4886,.T.);
#10332=EDGE_CURVE('',#8173,#8172,#4887,.T.);
#10333=EDGE_CURVE('',#8171,#8173,#4888,.T.);
#10334=EDGE_CURVE('',#8171,#8174,#6831,.T.);
#10335=EDGE_CURVE('',#8173,#8174,#4889,.T.);
#10336=EDGE_CURVE('',#8174,#8175,#4890,.T.);
#10337=EDGE_CURVE('',#8172,#8175,#4891,.T.);
#10338=EDGE_CURVE('',#8175,#8170,#6832,.T.);
#10339=EDGE_CURVE('',#8176,#8177,#4892,.T.);
#10340=EDGE_CURVE('',#8176,#8178,#4893,.T.);
#10341=EDGE_CURVE('',#8179,#8178,#4894,.T.);
#10342=EDGE_CURVE('',#8177,#8179,#4895,.T.);
#10343=EDGE_CURVE('',#8177,#8180,#6833,.T.);
#10344=EDGE_CURVE('',#8179,#8180,#4896,.T.);
#10345=EDGE_CURVE('',#8180,#8181,#4897,.T.);
#10346=EDGE_CURVE('',#8178,#8181,#4898,.T.);
#10347=EDGE_CURVE('',#8181,#8176,#6834,.T.);
#10348=EDGE_CURVE('',#8182,#8183,#4899,.T.);
#10349=EDGE_CURVE('',#8182,#8184,#4900,.T.);
#10350=EDGE_CURVE('',#8185,#8184,#4901,.T.);
#10351=EDGE_CURVE('',#8183,#8185,#4902,.T.);
#10352=EDGE_CURVE('',#8183,#8186,#6835,.T.);
#10353=EDGE_CURVE('',#8185,#8186,#4903,.T.);
#10354=EDGE_CURVE('',#8186,#8187,#4904,.T.);
#10355=EDGE_CURVE('',#8184,#8187,#4905,.T.);
#10356=EDGE_CURVE('',#8187,#8182,#6836,.T.);
#10357=EDGE_CURVE('',#8188,#8189,#4906,.T.);
#10358=EDGE_CURVE('',#8188,#8190,#4907,.T.);
#10359=EDGE_CURVE('',#8191,#8190,#4908,.T.);
#10360=EDGE_CURVE('',#8189,#8191,#4909,.T.);
#10361=EDGE_CURVE('',#8189,#8192,#6837,.T.);
#10362=EDGE_CURVE('',#8191,#8192,#4910,.T.);
#10363=EDGE_CURVE('',#8192,#8193,#4911,.T.);
#10364=EDGE_CURVE('',#8190,#8193,#4912,.T.);
#10365=EDGE_CURVE('',#8193,#8188,#6838,.T.);
#10366=EDGE_CURVE('',#8194,#8195,#4913,.T.);
#10367=EDGE_CURVE('',#8194,#8196,#4914,.T.);
#10368=EDGE_CURVE('',#8197,#8196,#4915,.T.);
#10369=EDGE_CURVE('',#8195,#8197,#4916,.T.);
#10370=EDGE_CURVE('',#8195,#8198,#6839,.T.);
#10371=EDGE_CURVE('',#8197,#8199,#4917,.T.);
#10372=EDGE_CURVE('',#8198,#8199,#6840,.T.);
#10373=EDGE_CURVE('',#8199,#8200,#4918,.T.);
#10374=EDGE_CURVE('',#8196,#8200,#4919,.T.);
#10375=EDGE_CURVE('',#8200,#8201,#6841,.T.);
#10376=EDGE_CURVE('',#8201,#8194,#6842,.T.);
#10377=EDGE_CURVE('',#8202,#8203,#4920,.T.);
#10378=EDGE_CURVE('',#8202,#8204,#4921,.T.);
#10379=EDGE_CURVE('',#8205,#8204,#4922,.T.);
#10380=EDGE_CURVE('',#8203,#8205,#4923,.T.);
#10381=EDGE_CURVE('',#8203,#8206,#6843,.T.);
#10382=EDGE_CURVE('',#8205,#8206,#4924,.T.);
#10383=EDGE_CURVE('',#8206,#8207,#4925,.T.);
#10384=EDGE_CURVE('',#8204,#8207,#4926,.T.);
#10385=EDGE_CURVE('',#8207,#8202,#6844,.T.);
#10386=EDGE_CURVE('',#8208,#8209,#4927,.T.);
#10387=EDGE_CURVE('',#8208,#8210,#4928,.T.);
#10388=EDGE_CURVE('',#8211,#8210,#4929,.T.);
#10389=EDGE_CURVE('',#8209,#8211,#4930,.T.);
#10390=EDGE_CURVE('',#8209,#8212,#6845,.T.);
#10391=EDGE_CURVE('',#8211,#8212,#4931,.T.);
#10392=EDGE_CURVE('',#8212,#8213,#4932,.T.);
#10393=EDGE_CURVE('',#8210,#8213,#4933,.T.);
#10394=EDGE_CURVE('',#8213,#8208,#6846,.T.);
#10395=EDGE_CURVE('',#8214,#8215,#4934,.T.);
#10396=EDGE_CURVE('',#8214,#8216,#4935,.T.);
#10397=EDGE_CURVE('',#8217,#8216,#4936,.T.);
#10398=EDGE_CURVE('',#8215,#8217,#4937,.T.);
#10399=EDGE_CURVE('',#8215,#8218,#6847,.T.);
#10400=EDGE_CURVE('',#8217,#8218,#4938,.T.);
#10401=EDGE_CURVE('',#8218,#8219,#4939,.T.);
#10402=EDGE_CURVE('',#8216,#8219,#4940,.T.);
#10403=EDGE_CURVE('',#8219,#8214,#6848,.T.);
#10404=EDGE_CURVE('',#8220,#8221,#4941,.T.);
#10405=EDGE_CURVE('',#8220,#8222,#4942,.T.);
#10406=EDGE_CURVE('',#8223,#8222,#4943,.T.);
#10407=EDGE_CURVE('',#8221,#8223,#4944,.T.);
#10408=EDGE_CURVE('',#8221,#8224,#6849,.T.);
#10409=EDGE_CURVE('',#8223,#8224,#4945,.T.);
#10410=EDGE_CURVE('',#8224,#8225,#4946,.T.);
#10411=EDGE_CURVE('',#8222,#8225,#4947,.T.);
#10412=EDGE_CURVE('',#8225,#8220,#6850,.T.);
#10413=EDGE_CURVE('',#8226,#8227,#4948,.T.);
#10414=EDGE_CURVE('',#8226,#8228,#4949,.T.);
#10415=EDGE_CURVE('',#8229,#8228,#4950,.T.);
#10416=EDGE_CURVE('',#8227,#8229,#4951,.T.);
#10417=EDGE_CURVE('',#8227,#8230,#6851,.T.);
#10418=EDGE_CURVE('',#8229,#8230,#4952,.T.);
#10419=EDGE_CURVE('',#8230,#8231,#4953,.T.);
#10420=EDGE_CURVE('',#8228,#8231,#4954,.T.);
#10421=EDGE_CURVE('',#8231,#8226,#6852,.T.);
#10422=EDGE_CURVE('',#8232,#8233,#4955,.T.);
#10423=EDGE_CURVE('',#8232,#8234,#4956,.T.);
#10424=EDGE_CURVE('',#8235,#8234,#4957,.T.);
#10425=EDGE_CURVE('',#8233,#8235,#4958,.T.);
#10426=EDGE_CURVE('',#8233,#8236,#6853,.T.);
#10427=EDGE_CURVE('',#8235,#8236,#4959,.T.);
#10428=EDGE_CURVE('',#8236,#8237,#4960,.T.);
#10429=EDGE_CURVE('',#8234,#8237,#4961,.T.);
#10430=EDGE_CURVE('',#8237,#8232,#6854,.T.);
#10431=EDGE_CURVE('',#8238,#8239,#4962,.T.);
#10432=EDGE_CURVE('',#8238,#8240,#4963,.T.);
#10433=EDGE_CURVE('',#8241,#8240,#4964,.T.);
#10434=EDGE_CURVE('',#8239,#8241,#4965,.T.);
#10435=EDGE_CURVE('',#8239,#8242,#6855,.T.);
#10436=EDGE_CURVE('',#8241,#8242,#4966,.T.);
#10437=EDGE_CURVE('',#8242,#8243,#4967,.T.);
#10438=EDGE_CURVE('',#8240,#8243,#4968,.T.);
#10439=EDGE_CURVE('',#8243,#8238,#6856,.T.);
#10440=EDGE_CURVE('',#8244,#8245,#4969,.T.);
#10441=EDGE_CURVE('',#8244,#8246,#4970,.T.);
#10442=EDGE_CURVE('',#8247,#8246,#4971,.T.);
#10443=EDGE_CURVE('',#8245,#8247,#4972,.T.);
#10444=EDGE_CURVE('',#8245,#8248,#6857,.T.);
#10445=EDGE_CURVE('',#8247,#8248,#4973,.T.);
#10446=EDGE_CURVE('',#8248,#8249,#4974,.T.);
#10447=EDGE_CURVE('',#8246,#8249,#4975,.T.);
#10448=EDGE_CURVE('',#8249,#8244,#6858,.T.);
#10449=EDGE_CURVE('',#8250,#8251,#4976,.T.);
#10450=EDGE_CURVE('',#8250,#8252,#4977,.T.);
#10451=EDGE_CURVE('',#8253,#8252,#4978,.T.);
#10452=EDGE_CURVE('',#8251,#8253,#4979,.T.);
#10453=EDGE_CURVE('',#8251,#8254,#6859,.T.);
#10454=EDGE_CURVE('',#8253,#8254,#4980,.T.);
#10455=EDGE_CURVE('',#8254,#8255,#4981,.T.);
#10456=EDGE_CURVE('',#8252,#8255,#4982,.T.);
#10457=EDGE_CURVE('',#8255,#8250,#6860,.T.);
#10458=EDGE_CURVE('',#8256,#8257,#4983,.T.);
#10459=EDGE_CURVE('',#8256,#8258,#4984,.T.);
#10460=EDGE_CURVE('',#8259,#8258,#4985,.T.);
#10461=EDGE_CURVE('',#8257,#8259,#4986,.T.);
#10462=EDGE_CURVE('',#8257,#8260,#6861,.T.);
#10463=EDGE_CURVE('',#8259,#8260,#4987,.T.);
#10464=EDGE_CURVE('',#8260,#8261,#4988,.T.);
#10465=EDGE_CURVE('',#8258,#8261,#4989,.T.);
#10466=EDGE_CURVE('',#8261,#8256,#6862,.T.);
#10467=EDGE_CURVE('',#8262,#8263,#4990,.T.);
#10468=EDGE_CURVE('',#8262,#8264,#4991,.T.);
#10469=EDGE_CURVE('',#8265,#8264,#4992,.T.);
#10470=EDGE_CURVE('',#8263,#8265,#4993,.T.);
#10471=EDGE_CURVE('',#8263,#8266,#6863,.T.);
#10472=EDGE_CURVE('',#8265,#8266,#4994,.T.);
#10473=EDGE_CURVE('',#8266,#8267,#4995,.T.);
#10474=EDGE_CURVE('',#8264,#8267,#4996,.T.);
#10475=EDGE_CURVE('',#8267,#8262,#6864,.T.);
#10476=EDGE_CURVE('',#8268,#8269,#4997,.T.);
#10477=EDGE_CURVE('',#8268,#8270,#4998,.T.);
#10478=EDGE_CURVE('',#8271,#8270,#4999,.T.);
#10479=EDGE_CURVE('',#8269,#8271,#5000,.T.);
#10480=EDGE_CURVE('',#8269,#8272,#6865,.T.);
#10481=EDGE_CURVE('',#8271,#8272,#5001,.T.);
#10482=EDGE_CURVE('',#8272,#8273,#5002,.T.);
#10483=EDGE_CURVE('',#8270,#8273,#5003,.T.);
#10484=EDGE_CURVE('',#8273,#8268,#6866,.T.);
#10485=EDGE_CURVE('',#8274,#8275,#5004,.T.);
#10486=EDGE_CURVE('',#8274,#8276,#5005,.T.);
#10487=EDGE_CURVE('',#8277,#8276,#5006,.T.);
#10488=EDGE_CURVE('',#8275,#8277,#5007,.T.);
#10489=EDGE_CURVE('',#8275,#8278,#6867,.T.);
#10490=EDGE_CURVE('',#8277,#8278,#5008,.T.);
#10491=EDGE_CURVE('',#8278,#8279,#5009,.T.);
#10492=EDGE_CURVE('',#8276,#8279,#5010,.T.);
#10493=EDGE_CURVE('',#8279,#8274,#6868,.T.);
#10494=EDGE_CURVE('',#8280,#8281,#5011,.T.);
#10495=EDGE_CURVE('',#8280,#8282,#5012,.T.);
#10496=EDGE_CURVE('',#8283,#8282,#5013,.T.);
#10497=EDGE_CURVE('',#8281,#8283,#5014,.T.);
#10498=EDGE_CURVE('',#8281,#8284,#6869,.T.);
#10499=EDGE_CURVE('',#8283,#8284,#5015,.T.);
#10500=EDGE_CURVE('',#8284,#8285,#5016,.T.);
#10501=EDGE_CURVE('',#8282,#8285,#5017,.T.);
#10502=EDGE_CURVE('',#8285,#8280,#6870,.T.);
#10503=EDGE_CURVE('',#8286,#8287,#5018,.T.);
#10504=EDGE_CURVE('',#8286,#8288,#5019,.T.);
#10505=EDGE_CURVE('',#8289,#8288,#5020,.T.);
#10506=EDGE_CURVE('',#8287,#8289,#5021,.T.);
#10507=EDGE_CURVE('',#8287,#8290,#6871,.T.);
#10508=EDGE_CURVE('',#8289,#8290,#5022,.T.);
#10509=EDGE_CURVE('',#8290,#8291,#5023,.T.);
#10510=EDGE_CURVE('',#8288,#8291,#5024,.T.);
#10511=EDGE_CURVE('',#8291,#8286,#6872,.T.);
#10512=EDGE_CURVE('',#8292,#8292,#6873,.T.);
#10513=EDGE_CURVE('',#8293,#8293,#6874,.T.);
#10514=EDGE_CURVE('',#8293,#8292,#5025,.T.);
#10515=EDGE_CURVE('',#7998,#8293,#5026,.T.);
#10516=EDGE_CURVE('',#8294,#8294,#6875,.T.);
#10517=EDGE_CURVE('',#8294,#8001,#5027,.T.);
#10518=EDGE_CURVE('',#8295,#8295,#6876,.T.);
#10519=EDGE_CURVE('',#8296,#8296,#6877,.T.);
#10520=EDGE_CURVE('',#8296,#8295,#5028,.T.);
#10521=EDGE_CURVE('',#8297,#8297,#6878,.T.);
#10522=EDGE_CURVE('',#8297,#8201,#5029,.T.);
#10523=EDGE_CURVE('',#8198,#8296,#5030,.T.);
#10524=EDGE_CURVE('',#8298,#8298,#6879,.T.);
#10525=EDGE_CURVE('',#8298,#8297,#5031,.T.);
#10526=EDGE_CURVE('',#8299,#8300,#5032,.F.);
#10527=EDGE_CURVE('',#8300,#8301,#5033,.T.);
#10528=EDGE_CURVE('',#8301,#8302,#5034,.F.);
#10529=EDGE_CURVE('',#8302,#8299,#5035,.T.);
#10530=EDGE_CURVE('',#8303,#8300,#5036,.T.);
#10531=EDGE_CURVE('',#8304,#8303,#5037,.T.);
#10532=EDGE_CURVE('',#8301,#8304,#5038,.T.);
#10533=EDGE_CURVE('',#8305,#8306,#5039,.F.);
#10534=EDGE_CURVE('',#8306,#8307,#5040,.T.);
#10535=EDGE_CURVE('',#8307,#8308,#5041,.F.);
#10536=EDGE_CURVE('',#8308,#8305,#5042,.T.);
#10537=EDGE_CURVE('',#8309,#8306,#5043,.T.);
#10538=EDGE_CURVE('',#8309,#8310,#5044,.T.);
#10539=EDGE_CURVE('',#8307,#8310,#5045,.T.);
#10540=EDGE_CURVE('',#8311,#8312,#5046,.T.);
#10541=EDGE_CURVE('',#8312,#8313,#5047,.F.);
#10542=EDGE_CURVE('',#8313,#8314,#5048,.T.);
#10543=EDGE_CURVE('',#8314,#8315,#5049,.T.);
#10544=EDGE_CURVE('',#8315,#8311,#5050,.T.);
#10545=EDGE_CURVE('',#8315,#8316,#5051,.T.);
#10546=EDGE_CURVE('',#8316,#8317,#5052,.T.);
#10547=EDGE_CURVE('',#8317,#8311,#5053,.T.);
#10548=EDGE_CURVE('',#8318,#8303,#5054,.T.);
#10549=EDGE_CURVE('',#8303,#8317,#6880,.T.);
#10550=EDGE_CURVE('',#8316,#8318,#6881,.T.);
#10551=EDGE_CURVE('',#8319,#8303,#5055,.F.);
#10552=EDGE_CURVE('',#8318,#8319,#5056,.T.);
#10553=EDGE_CURVE('',#8299,#8309,#5057,.T.);
#10554=EDGE_CURVE('',#8305,#8312,#5058,.T.);
#10555=EDGE_CURVE('',#8320,#8320,#6882,.T.);
#10556=EDGE_CURVE('',#8321,#8321,#6883,.T.);
#10557=EDGE_CURVE('',#8322,#8323,#5059,.T.);
#10558=EDGE_CURVE('',#8323,#8324,#5060,.T.);
#10559=EDGE_CURVE('',#8325,#8324,#5061,.T.);
#10560=EDGE_CURVE('',#8325,#8326,#5062,.T.);
#10561=EDGE_CURVE('',#8326,#8322,#5063,.T.);
#10562=EDGE_CURVE('',#8327,#8304,#5064,.T.);
#10563=EDGE_CURVE('',#8327,#8328,#5065,.T.);
#10564=EDGE_CURVE('',#8328,#8304,#5066,.T.);
#10565=EDGE_CURVE('',#8328,#8329,#6884,.T.);
#10566=EDGE_CURVE('',#8329,#8330,#5067,.T.);
#10567=EDGE_CURVE('',#8330,#8304,#6885,.T.);
#10568=EDGE_CURVE('',#8326,#8330,#5068,.T.);
#10569=EDGE_CURVE('',#8329,#8322,#5069,.T.);
#10570=EDGE_CURVE('',#8331,#8324,#5070,.T.);
#10571=EDGE_CURVE('',#8323,#8332,#5071,.T.);
#10572=EDGE_CURVE('',#8333,#8332,#5072,.T.);
#10573=EDGE_CURVE('',#8333,#8334,#5073,.T.);
#10574=EDGE_CURVE('',#8334,#8331,#252,.F.);
#10575=EDGE_CURVE('',#8322,#8335,#5074,.T.);
#10576=EDGE_CURVE('',#8332,#8335,#5075,.T.);
#10577=EDGE_CURVE('',#8329,#8336,#5076,.T.);
#10578=EDGE_CURVE('',#8335,#8336,#5077,.T.);
#10579=EDGE_CURVE('',#8328,#8337,#5078,.T.);
#10580=EDGE_CURVE('',#8336,#8337,#6886,.T.);
#10581=EDGE_CURVE('',#8318,#8338,#5079,.T.);
#10582=EDGE_CURVE('',#8339,#8338,#5080,.T.);
#10583=EDGE_CURVE('',#8340,#8339,#5081,.T.);
#10584=EDGE_CURVE('',#8337,#8340,#5082,.T.);
#10585=EDGE_CURVE('',#8319,#8327,#5083,.T.);
#10586=EDGE_CURVE('',#8341,#8342,#790,.T.);
#10587=EDGE_CURVE('',#8343,#8342,#791,.T.);
#10588=EDGE_CURVE('',#8343,#8344,#792,.T.);
#10589=EDGE_CURVE('',#8344,#8341,#5084,.T.);
#10590=EDGE_CURVE('',#8342,#8345,#793,.T.);
#10591=EDGE_CURVE('',#8345,#8346,#5085,.T.);
#10592=EDGE_CURVE('',#8346,#8343,#794,.T.);
#10593=EDGE_CURVE('',#8313,#8347,#5086,.T.);
#10594=EDGE_CURVE('',#8348,#8347,#253,.T.);
#10595=EDGE_CURVE('',#8348,#8346,#5087,.T.);
#10596=EDGE_CURVE('',#8345,#8314,#5088,.T.);
#10597=EDGE_CURVE('',#8349,#8344,#5089,.T.);
#10598=EDGE_CURVE('',#8350,#8349,#5090,.T.);
#10599=EDGE_CURVE('',#8351,#8350,#5091,.T.);
#10600=EDGE_CURVE('',#8352,#8351,#6887,.T.);
#10601=EDGE_CURVE('',#8353,#8352,#5092,.T.);
#10602=EDGE_CURVE('',#8341,#8353,#5093,.T.);
#10603=EDGE_CURVE('',#8354,#8354,#6888,.T.);
#10604=EDGE_CURVE('',#8355,#8355,#6889,.T.);
#10605=EDGE_CURVE('',#8346,#8356,#5094,.T.);
#10606=EDGE_CURVE('',#8357,#8356,#795,.T.);
#10607=EDGE_CURVE('',#8349,#8357,#796,.T.);
#10608=EDGE_CURVE('',#8348,#8358,#6890,.T.);
#10609=EDGE_CURVE('',#8358,#8334,#6891,.T.);
#10610=EDGE_CURVE('',#8359,#8333,#5095,.T.);
#10611=EDGE_CURVE('',#8356,#8359,#5096,.T.);
#10612=EDGE_CURVE('',#8360,#8361,#797,.T.);
#10613=EDGE_CURVE('',#8362,#8361,#798,.T.);
#10614=EDGE_CURVE('',#8362,#8363,#799,.T.);
#10615=EDGE_CURVE('',#8363,#8360,#5097,.T.);
#10616=EDGE_CURVE('',#8361,#8333,#800,.T.);
#10617=EDGE_CURVE('',#8332,#8362,#801,.T.);
#10618=EDGE_CURVE('',#8364,#8335,#254,.T.);
#10619=EDGE_CURVE('',#8364,#8363,#5098,.T.);
#10620=EDGE_CURVE('',#8325,#8308,#5099,.T.);
#10621=EDGE_CURVE('',#8310,#8302,#5100,.T.);
#10622=EDGE_CURVE('',#8365,#8365,#6892,.T.);
#10623=EDGE_CURVE('',#8366,#8366,#6893,.T.);
#10624=EDGE_CURVE('',#8331,#8367,#5101,.T.);
#10625=EDGE_CURVE('',#8367,#8368,#5102,.T.);
#10626=EDGE_CURVE('',#8368,#8347,#5103,.T.);
#10627=EDGE_CURVE('',#8369,#8357,#802,.T.);
#10628=EDGE_CURVE('',#8369,#8350,#803,.T.);
#10629=EDGE_CURVE('',#8370,#8371,#804,.T.);
#10630=EDGE_CURVE('',#8372,#8371,#805,.T.);
#10631=EDGE_CURVE('',#8372,#8373,#806,.T.);
#10632=EDGE_CURVE('',#8373,#8370,#5104,.T.);
#10633=EDGE_CURVE('',#8371,#8340,#807,.T.);
#10634=EDGE_CURVE('',#8340,#8359,#5105,.T.);
#10635=EDGE_CURVE('',#8359,#8372,#808,.T.);
#10636=EDGE_CURVE('',#8339,#8356,#5106,.T.);
#10637=EDGE_CURVE('',#8339,#8369,#809,.T.);
#10638=EDGE_CURVE('',#8338,#8351,#6894,.T.);
#10639=EDGE_CURVE('',#8370,#8374,#5107,.T.);
#10640=EDGE_CURVE('',#8337,#8374,#6895,.T.);
#10641=EDGE_CURVE('',#8360,#8373,#5108,.T.);
#10642=EDGE_CURVE('',#8336,#8375,#6896,.T.);
#10643=EDGE_CURVE('',#8375,#8364,#5109,.T.);
#10644=EDGE_CURVE('',#8374,#8375,#6897,.T.);
#10645=EDGE_CURVE('',#8376,#8376,#6898,.T.);
#10646=EDGE_CURVE('',#8377,#8377,#6899,.T.);
#10647=EDGE_CURVE('',#8353,#8378,#255,.T.);
#10648=EDGE_CURVE('',#8378,#8345,#5110,.T.);
#10649=EDGE_CURVE('',#8379,#8352,#6900,.T.);
#10650=EDGE_CURVE('',#8338,#8379,#6901,.T.);
#10651=EDGE_CURVE('',#8379,#8378,#5111,.T.);
#10652=EDGE_CURVE('',#8315,#8378,#5112,.T.);
#10653=EDGE_CURVE('',#8316,#8379,#5113,.T.);
#10654=EDGE_CURVE('',#8366,#8377,#5114,.T.);
#10655=EDGE_CURVE('',#8355,#8321,#5115,.T.);
#10656=EDGE_CURVE('',#8365,#8376,#5116,.T.);
#10657=EDGE_CURVE('',#8354,#8320,#5117,.T.);
#10658=EDGE_CURVE('',#8380,#8380,#6902,.T.);
#10659=EDGE_CURVE('',#8380,#8358,#5118,.T.);
#10660=EDGE_CURVE('',#8368,#8367,#6903,.T.);
#10661=EDGE_CURVE('',#8381,#8381,#6904,.T.);
#10662=EDGE_CURVE('',#8381,#8380,#6905,.T.);
#10663=EDGE_CURVE('',#8382,#8382,#6906,.T.);
#10664=EDGE_CURVE('',#8382,#8383,#5119,.T.);
#10665=EDGE_CURVE('',#8383,#8383,#6907,.T.);
#10666=EDGE_CURVE('',#8382,#8384,#5120,.T.);
#10667=EDGE_CURVE('',#8384,#8384,#6908,.T.);
#10668=EDGE_CURVE('',#8385,#8385,#6909,.T.);
#10669=EDGE_CURVE('',#8385,#8383,#5121,.T.);
#10670=EDGE_CURVE('',#8384,#8386,#5122,.T.);
#10671=EDGE_CURVE('',#8386,#8386,#6910,.T.);
#10672=EDGE_CURVE('',#8387,#8387,#6911,.T.);
#10673=EDGE_CURVE('',#8388,#8388,#6912,.T.);
#10674=EDGE_CURVE('',#8388,#8389,#6913,.T.);
#10675=EDGE_CURVE('',#8389,#8390,#6914,.T.);
#10676=EDGE_CURVE('',#8390,#8389,#6915,.T.);
#10677=EDGE_CURVE('',#8390,#8391,#5123,.T.);
#10678=EDGE_CURVE('',#8391,#8392,#6916,.T.);
#10679=EDGE_CURVE('',#8392,#8391,#6917,.T.);
#10680=EDGE_CURVE('',#8393,#8393,#6918,.T.);
#10681=EDGE_CURVE('',#8394,#8394,#6919,.T.);
#10682=EDGE_CURVE('',#8394,#8393,#6920,.T.);
#10683=EDGE_CURVE('',#8387,#8394,#5124,.T.);
#10684=EDGE_CURVE('',#8392,#8385,#6921,.T.);
#10685=EDGE_CURVE('',#8395,#8396,#5125,.T.);
#10686=EDGE_CURVE('',#8396,#8397,#6922,.T.);
#10687=EDGE_CURVE('',#8397,#8398,#5126,.T.);
#10688=EDGE_CURVE('',#8398,#8395,#6923,.T.);
#10689=EDGE_CURVE('',#8399,#8400,#5127,.T.);
#10690=EDGE_CURVE('',#8400,#8396,#5128,.T.);
#10691=EDGE_CURVE('',#8395,#8399,#5129,.T.);
#10692=EDGE_CURVE('',#8401,#8402,#5130,.T.);
#10693=EDGE_CURVE('',#8402,#8400,#6924,.T.);
#10694=EDGE_CURVE('',#8399,#8401,#6925,.T.);
#10695=EDGE_CURVE('',#8397,#8402,#5131,.T.);
#10696=EDGE_CURVE('',#8401,#8398,#5132,.T.);
#10697=EDGE_CURVE('',#8397,#8403,#5133,.T.);
#10698=EDGE_CURVE('',#8404,#8403,#5134,.T.);
#10699=EDGE_CURVE('',#8402,#8404,#5135,.T.);
#10700=EDGE_CURVE('',#8396,#8405,#5136,.T.);
#10701=EDGE_CURVE('',#8403,#8405,#6926,.T.);
#10702=EDGE_CURVE('',#8406,#8406,#6927,.T.);
#10703=EDGE_CURVE('',#8407,#8407,#6928,.T.);
#10704=EDGE_CURVE('',#8403,#8408,#5137,.T.);
#10705=EDGE_CURVE('',#8408,#8409,#5138,.T.);
#10706=EDGE_CURVE('',#8409,#8404,#5139,.T.);
#10707=EDGE_CURVE('',#8405,#8410,#5140,.T.);
#10708=EDGE_CURVE('',#8410,#8408,#6929,.T.);
#10709=EDGE_CURVE('',#8411,#8412,#5141,.T.);
#10710=EDGE_CURVE('',#8412,#8410,#5142,.T.);
#10711=EDGE_CURVE('',#8405,#8411,#5143,.T.);
#10712=EDGE_CURVE('',#8409,#8412,#6930,.T.);
#10713=EDGE_CURVE('',#8411,#8404,#6931,.T.);
#10714=EDGE_CURVE('',#8413,#8409,#5144,.T.);
#10715=EDGE_CURVE('',#8414,#8413,#6932,.T.);
#10716=EDGE_CURVE('',#8412,#8414,#5145,.T.);
#10717=EDGE_CURVE('',#8408,#8415,#5146,.T.);
#10718=EDGE_CURVE('',#8413,#8415,#5147,.T.);
#10719=EDGE_CURVE('',#8416,#8413,#5148,.T.);
#10720=EDGE_CURVE('',#8415,#8417,#5149,.T.);
#10721=EDGE_CURVE('',#8417,#8416,#5150,.T.);
#10722=EDGE_CURVE('',#8418,#8414,#5151,.T.);
#10723=EDGE_CURVE('',#8416,#8418,#6933,.T.);
#10724=EDGE_CURVE('',#8419,#8420,#5152,.T.);
#10725=EDGE_CURVE('',#8420,#8414,#5153,.T.);
#10726=EDGE_CURVE('',#8418,#8419,#5154,.T.);
#10727=EDGE_CURVE('',#8415,#8420,#6934,.T.);
#10728=EDGE_CURVE('',#8419,#8417,#6935,.T.);
#10729=EDGE_CURVE('',#8410,#8420,#5155,.T.);
#10730=EDGE_CURVE('',#8421,#8421,#6936,.T.);
#10731=EDGE_CURVE('',#8422,#8422,#6937,.T.);
#10732=EDGE_CURVE('',#8407,#8421,#5156,.T.);
#10733=EDGE_CURVE('',#8406,#8422,#5157,.T.);
#10734=EDGE_CURVE('',#8400,#8411,#5158,.T.);
#10735=EDGE_CURVE('',#8423,#8423,#6938,.T.);
#10736=EDGE_CURVE('',#8424,#8424,#6939,.T.);
#10737=EDGE_CURVE('',#8424,#8423,#5159,.T.);
#10738=EDGE_CURVE('',#8425,#8425,#6940,.T.);
#10739=EDGE_CURVE('',#8425,#8424,#5160,.T.);
#10740=EDGE_CURVE('',#8426,#8426,#6941,.T.);
#10741=EDGE_CURVE('',#8427,#8427,#6942,.T.);
#10742=EDGE_CURVE('',#8427,#8426,#5161,.T.);
#10743=EDGE_CURVE('',#8428,#8428,#6943,.T.);
#10744=EDGE_CURVE('',#8429,#8429,#6944,.T.);
#10745=EDGE_CURVE('',#8429,#8428,#5162,.T.);
#10746=EDGE_CURVE('',#8430,#8430,#6945,.T.);
#10747=EDGE_CURVE('',#8431,#8431,#6946,.T.);
#10748=EDGE_CURVE('',#8431,#8430,#5163,.T.);
#10749=EDGE_CURVE('',#8432,#8432,#6947,.T.);
#10750=EDGE_CURVE('',#8433,#8433,#6948,.T.);
#10751=EDGE_CURVE('',#8433,#8432,#5164,.T.);
#10752=EDGE_CURVE('',#8434,#8434,#6949,.T.);
#10753=EDGE_CURVE('',#8434,#8433,#5165,.T.);
#10754=EDGE_CURVE('',#8435,#8436,#6950,.T.);
#10755=EDGE_CURVE('',#8436,#8437,#810,.T.);
#10756=EDGE_CURVE('',#8437,#8438,#6951,.T.);
#10757=EDGE_CURVE('',#8435,#8438,#811,.T.);
#10758=EDGE_CURVE('',#8436,#8439,#5166,.T.);
#10759=EDGE_CURVE('',#8439,#8440,#5167,.T.);
#10760=EDGE_CURVE('',#8440,#8437,#5168,.T.);
#10761=EDGE_CURVE('',#8439,#8441,#5169,.T.);
#10762=EDGE_CURVE('',#8441,#8442,#5170,.T.);
#10763=EDGE_CURVE('',#8442,#8440,#5171,.T.);
#10764=EDGE_CURVE('',#8438,#8442,#5172,.T.);
#10765=EDGE_CURVE('',#8441,#8435,#5173,.T.);
#10766=EDGE_CURVE('',#8443,#8438,#5174,.T.);
#10767=EDGE_CURVE('',#8444,#8443,#5175,.T.);
#10768=EDGE_CURVE('',#8444,#8442,#5176,.T.);
#10769=EDGE_CURVE('',#8445,#8437,#5177,.T.);
#10770=EDGE_CURVE('',#8443,#8445,#6952,.T.);
#10771=EDGE_CURVE('',#8446,#8446,#6953,.T.);
#10772=EDGE_CURVE('',#8445,#8447,#812,.T.);
#10773=EDGE_CURVE('',#8447,#8448,#6954,.T.);
#10774=EDGE_CURVE('',#8448,#8443,#813,.T.);
#10775=EDGE_CURVE('',#8448,#8449,#5178,.T.);
#10776=EDGE_CURVE('',#8449,#8444,#5179,.T.);
#10777=EDGE_CURVE('',#8449,#8450,#5180,.T.);
#10778=EDGE_CURVE('',#8450,#8451,#5181,.T.);
#10779=EDGE_CURVE('',#8451,#8444,#5182,.T.);
#10780=EDGE_CURVE('',#8445,#8451,#5183,.T.);
#10781=EDGE_CURVE('',#8450,#8447,#5184,.T.);
#10782=EDGE_CURVE('',#8451,#8440,#5185,.T.);
#10783=EDGE_CURVE('',#8452,#8452,#6955,.T.);
#10784=EDGE_CURVE('',#8452,#8446,#5186,.T.);
#10785=EDGE_CURVE('',#8453,#8453,#6956,.T.);
#10786=EDGE_CURVE('',#8454,#8454,#6957,.T.);
#10787=EDGE_CURVE('',#8455,#8455,#6958,.T.);
#10788=EDGE_CURVE('',#8455,#8454,#5187,.T.);
#10789=EDGE_CURVE('',#8453,#8455,#5188,.T.);
#10790=EDGE_CURVE('',#8456,#8457,#6959,.T.);
#10791=EDGE_CURVE('',#8457,#8458,#5189,.T.);
#10792=EDGE_CURVE('',#8459,#8458,#6960,.T.);
#10793=EDGE_CURVE('',#8456,#8459,#5190,.T.);
#10794=EDGE_CURVE('',#8456,#8460,#5191,.T.);
#10795=EDGE_CURVE('',#8461,#8459,#5192,.T.);
#10796=EDGE_CURVE('',#8460,#8461,#5193,.T.);
#10797=EDGE_CURVE('',#8460,#8462,#6961,.T.);
#10798=EDGE_CURVE('',#8463,#8461,#6962,.T.);
#10799=EDGE_CURVE('',#8462,#8463,#5194,.T.);
#10800=EDGE_CURVE('',#8457,#8462,#5195,.T.);
#10801=EDGE_CURVE('',#8458,#8463,#5196,.T.);
#10802=ORIENTED_EDGE('',*,*,#8464,.T.);
#10803=ORIENTED_EDGE('',*,*,#8465,.T.);
#10804=ORIENTED_EDGE('',*,*,#8466,.T.);
#10805=ORIENTED_EDGE('',*,*,#8467,.T.);
#10806=ORIENTED_EDGE('',*,*,#8466,.F.);
#10807=ORIENTED_EDGE('',*,*,#8468,.F.);
#10808=ORIENTED_EDGE('',*,*,#8469,.T.);
#10809=ORIENTED_EDGE('',*,*,#8464,.F.);
#10810=ORIENTED_EDGE('',*,*,#8465,.F.);
#10811=ORIENTED_EDGE('',*,*,#8469,.F.);
#10812=ORIENTED_EDGE('',*,*,#8470,.T.);
#10813=ORIENTED_EDGE('',*,*,#8467,.F.);
#10814=ORIENTED_EDGE('',*,*,#8471,.T.);
#10815=ORIENTED_EDGE('',*,*,#8472,.T.);
#10816=ORIENTED_EDGE('',*,*,#8468,.T.);
#10817=ORIENTED_EDGE('',*,*,#8472,.F.);
#10818=ORIENTED_EDGE('',*,*,#8473,.F.);
#10819=ORIENTED_EDGE('',*,*,#8474,.F.);
#10820=ORIENTED_EDGE('',*,*,#8475,.F.);
#10821=ORIENTED_EDGE('',*,*,#8476,.F.);
#10822=ORIENTED_EDGE('',*,*,#8477,.F.);
#10823=ORIENTED_EDGE('',*,*,#8478,.F.);
#10824=ORIENTED_EDGE('',*,*,#8479,.F.);
#10825=ORIENTED_EDGE('',*,*,#8480,.F.);
#10826=ORIENTED_EDGE('',*,*,#8481,.F.);
#10827=ORIENTED_EDGE('',*,*,#8482,.F.);
#10828=ORIENTED_EDGE('',*,*,#8471,.F.);
#10829=ORIENTED_EDGE('',*,*,#8483,.T.);
#10830=ORIENTED_EDGE('',*,*,#8484,.F.);
#10831=ORIENTED_EDGE('',*,*,#8485,.T.);
#10832=ORIENTED_EDGE('',*,*,#8486,.T.);
#10833=ORIENTED_EDGE('',*,*,#8484,.T.);
#10834=ORIENTED_EDGE('',*,*,#8487,.T.);
#10835=ORIENTED_EDGE('',*,*,#8488,.T.);
#10836=ORIENTED_EDGE('',*,*,#8489,.T.);
#10837=ORIENTED_EDGE('',*,*,#8490,.T.);
#10838=ORIENTED_EDGE('',*,*,#8491,.T.);
#10839=ORIENTED_EDGE('',*,*,#8488,.F.);
#10840=ORIENTED_EDGE('',*,*,#8492,.T.);
#10841=ORIENTED_EDGE('',*,*,#8486,.F.);
#10842=ORIENTED_EDGE('',*,*,#8493,.F.);
#10843=ORIENTED_EDGE('',*,*,#8494,.F.);
#10844=ORIENTED_EDGE('',*,*,#8495,.F.);
#10845=ORIENTED_EDGE('',*,*,#8496,.F.);
#10846=ORIENTED_EDGE('',*,*,#8497,.F.);
#10847=ORIENTED_EDGE('',*,*,#8498,.F.);
#10848=ORIENTED_EDGE('',*,*,#8499,.F.);
#10849=ORIENTED_EDGE('',*,*,#8500,.F.);
#10850=ORIENTED_EDGE('',*,*,#8501,.F.);
#10851=ORIENTED_EDGE('',*,*,#8502,.F.);
#10852=ORIENTED_EDGE('',*,*,#8503,.F.);
#10853=ORIENTED_EDGE('',*,*,#8504,.T.);
#10854=ORIENTED_EDGE('',*,*,#8505,.F.);
#10855=ORIENTED_EDGE('',*,*,#8485,.F.);
#10856=ORIENTED_EDGE('',*,*,#8489,.F.);
#10857=ORIENTED_EDGE('',*,*,#8506,.T.);
#10858=ORIENTED_EDGE('',*,*,#8507,.F.);
#10859=ORIENTED_EDGE('',*,*,#8493,.T.);
#10860=ORIENTED_EDGE('',*,*,#8491,.F.);
#10861=ORIENTED_EDGE('',*,*,#8508,.T.);
#10862=ORIENTED_EDGE('',*,*,#8509,.F.);
#10863=ORIENTED_EDGE('',*,*,#8510,.F.);
#10864=ORIENTED_EDGE('',*,*,#8511,.F.);
#10865=ORIENTED_EDGE('',*,*,#8506,.F.);
#10866=ORIENTED_EDGE('',*,*,#8512,.T.);
#10867=ORIENTED_EDGE('',*,*,#8513,.F.);
#10868=ORIENTED_EDGE('',*,*,#8514,.T.);
#10869=ORIENTED_EDGE('',*,*,#8515,.T.);
#10870=ORIENTED_EDGE('',*,*,#8516,.T.);
#10871=ORIENTED_EDGE('',*,*,#8517,.F.);
#10872=ORIENTED_EDGE('',*,*,#8518,.T.);
#10873=ORIENTED_EDGE('',*,*,#8519,.T.);
#10874=ORIENTED_EDGE('',*,*,#8517,.T.);
#10875=ORIENTED_EDGE('',*,*,#8520,.T.);
#10876=ORIENTED_EDGE('',*,*,#8521,.T.);
#10877=ORIENTED_EDGE('',*,*,#8522,.T.);
#10878=ORIENTED_EDGE('',*,*,#8523,.T.);
#10879=ORIENTED_EDGE('',*,*,#8524,.T.);
#10880=ORIENTED_EDGE('',*,*,#8525,.T.);
#10881=ORIENTED_EDGE('',*,*,#8526,.T.);
#10882=ORIENTED_EDGE('',*,*,#8525,.F.);
#10883=ORIENTED_EDGE('',*,*,#8527,.T.);
#10884=ORIENTED_EDGE('',*,*,#8521,.F.);
#10885=ORIENTED_EDGE('',*,*,#8528,.T.);
#10886=ORIENTED_EDGE('',*,*,#8529,.T.);
#10887=ORIENTED_EDGE('',*,*,#8530,.T.);
#10888=ORIENTED_EDGE('',*,*,#8531,.T.);
#10889=ORIENTED_EDGE('',*,*,#8532,.T.);
#10890=ORIENTED_EDGE('',*,*,#8529,.F.);
#10891=ORIENTED_EDGE('',*,*,#8533,.T.);
#10892=ORIENTED_EDGE('',*,*,#8523,.F.);
#10893=ORIENTED_EDGE('',*,*,#8534,.T.);
#10894=ORIENTED_EDGE('',*,*,#8535,.T.);
#10895=ORIENTED_EDGE('',*,*,#8536,.T.);
#10896=ORIENTED_EDGE('',*,*,#8537,.T.);
#10897=ORIENTED_EDGE('',*,*,#8538,.T.);
#10898=ORIENTED_EDGE('',*,*,#8535,.F.);
#10899=ORIENTED_EDGE('',*,*,#8539,.T.);
#10900=ORIENTED_EDGE('',*,*,#8531,.F.);
#10901=ORIENTED_EDGE('',*,*,#8540,.T.);
#10902=ORIENTED_EDGE('',*,*,#8513,.T.);
#10903=ORIENTED_EDGE('',*,*,#8541,.T.);
#10904=ORIENTED_EDGE('',*,*,#8542,.T.);
#10905=ORIENTED_EDGE('',*,*,#8543,.T.);
#10906=ORIENTED_EDGE('',*,*,#8542,.F.);
#10907=ORIENTED_EDGE('',*,*,#8544,.T.);
#10908=ORIENTED_EDGE('',*,*,#8537,.F.);
#10909=ORIENTED_EDGE('',*,*,#8545,.T.);
#10910=ORIENTED_EDGE('',*,*,#8526,.F.);
#10911=ORIENTED_EDGE('',*,*,#8528,.F.);
#10912=ORIENTED_EDGE('',*,*,#8520,.F.);
#10913=ORIENTED_EDGE('',*,*,#8516,.F.);
#10914=ORIENTED_EDGE('',*,*,#8546,.T.);
#10915=ORIENTED_EDGE('',*,*,#8547,.T.);
#10916=ORIENTED_EDGE('',*,*,#8548,.T.);
#10917=ORIENTED_EDGE('',*,*,#8519,.F.);
#10918=ORIENTED_EDGE('',*,*,#8549,.F.);
#10919=ORIENTED_EDGE('',*,*,#8550,.F.);
#10920=ORIENTED_EDGE('',*,*,#8551,.F.);
#10921=ORIENTED_EDGE('',*,*,#8546,.F.);
#10922=ORIENTED_EDGE('',*,*,#8518,.F.);
#10923=ORIENTED_EDGE('',*,*,#8522,.F.);
#10924=ORIENTED_EDGE('',*,*,#8552,.T.);
#10925=ORIENTED_EDGE('',*,*,#8553,.T.);
#10926=ORIENTED_EDGE('',*,*,#8549,.T.);
#10927=ORIENTED_EDGE('',*,*,#8527,.F.);
#10928=ORIENTED_EDGE('',*,*,#8524,.F.);
#10929=ORIENTED_EDGE('',*,*,#8533,.F.);
#10930=ORIENTED_EDGE('',*,*,#8532,.F.);
#10931=ORIENTED_EDGE('',*,*,#8539,.F.);
#10932=ORIENTED_EDGE('',*,*,#8538,.F.);
#10933=ORIENTED_EDGE('',*,*,#8544,.F.);
#10934=ORIENTED_EDGE('',*,*,#8554,.F.);
#10935=ORIENTED_EDGE('',*,*,#8555,.F.);
#10936=ORIENTED_EDGE('',*,*,#8552,.F.);
#10937=ORIENTED_EDGE('',*,*,#8556,.T.);
#10938=ORIENTED_EDGE('',*,*,#8557,.T.);
#10939=ORIENTED_EDGE('',*,*,#8558,.T.);
#10940=ORIENTED_EDGE('',*,*,#8559,.T.);
#10941=ORIENTED_EDGE('',*,*,#8558,.F.);
#10942=ORIENTED_EDGE('',*,*,#8560,.T.);
#10943=ORIENTED_EDGE('',*,*,#8561,.T.);
#10944=ORIENTED_EDGE('',*,*,#8556,.F.);
#10945=ORIENTED_EDGE('',*,*,#8562,.T.);
#10946=ORIENTED_EDGE('',*,*,#8563,.T.);
#10947=ORIENTED_EDGE('',*,*,#8561,.F.);
#10948=ORIENTED_EDGE('',*,*,#8564,.T.);
#10949=ORIENTED_EDGE('',*,*,#8565,.T.);
#10950=ORIENTED_EDGE('',*,*,#8566,.T.);
#10951=ORIENTED_EDGE('',*,*,#8560,.F.);
#10952=ORIENTED_EDGE('',*,*,#8567,.T.);
#10953=ORIENTED_EDGE('',*,*,#8568,.T.);
#10954=ORIENTED_EDGE('',*,*,#8569,.T.);
#10955=ORIENTED_EDGE('',*,*,#8557,.F.);
#10956=ORIENTED_EDGE('',*,*,#8570,.F.);
#10957=ORIENTED_EDGE('',*,*,#8571,.T.);
#10958=ORIENTED_EDGE('',*,*,#8567,.F.);
#10959=ORIENTED_EDGE('',*,*,#8572,.F.);
#10960=ORIENTED_EDGE('',*,*,#8573,.F.);
#10961=ORIENTED_EDGE('',*,*,#8574,.F.);
#10962=ORIENTED_EDGE('',*,*,#8575,.T.);
#10963=ORIENTED_EDGE('',*,*,#8576,.T.);
#10964=ORIENTED_EDGE('',*,*,#8573,.T.);
#10965=ORIENTED_EDGE('',*,*,#8509,.T.);
#10966=ORIENTED_EDGE('',*,*,#8577,.T.);
#10967=ORIENTED_EDGE('',*,*,#8578,.T.);
#10968=ORIENTED_EDGE('',*,*,#8574,.T.);
#10969=ORIENTED_EDGE('',*,*,#8579,.T.);
#10970=ORIENTED_EDGE('',*,*,#8580,.F.);
#10971=ORIENTED_EDGE('',*,*,#8581,.F.);
#10972=ORIENTED_EDGE('',*,*,#8582,.F.);
#10973=ORIENTED_EDGE('',*,*,#8583,.T.);
#10974=ORIENTED_EDGE('',*,*,#8584,.T.);
#10975=ORIENTED_EDGE('',*,*,#8507,.T.);
#10976=ORIENTED_EDGE('',*,*,#8583,.F.);
#10977=ORIENTED_EDGE('',*,*,#8511,.T.);
#10978=ORIENTED_EDGE('',*,*,#8581,.T.);
#10979=ORIENTED_EDGE('',*,*,#8585,.T.);
#10980=ORIENTED_EDGE('',*,*,#8572,.T.);
#10981=ORIENTED_EDGE('',*,*,#8586,.T.);
#10982=ORIENTED_EDGE('',*,*,#8582,.T.);
#10983=ORIENTED_EDGE('',*,*,#8510,.T.);
#10984=ORIENTED_EDGE('',*,*,#8587,.F.);
#10985=ORIENTED_EDGE('',*,*,#8588,.F.);
#10986=ORIENTED_EDGE('',*,*,#8589,.F.);
#10987=ORIENTED_EDGE('',*,*,#8590,.T.);
#10988=ORIENTED_EDGE('',*,*,#8591,.T.);
#10989=ORIENTED_EDGE('',*,*,#8592,.T.);
#10990=ORIENTED_EDGE('',*,*,#8590,.F.);
#10991=ORIENTED_EDGE('',*,*,#8593,.T.);
#10992=ORIENTED_EDGE('',*,*,#8588,.T.);
#10993=ORIENTED_EDGE('',*,*,#8594,.T.);
#10994=ORIENTED_EDGE('',*,*,#8580,.T.);
#10995=ORIENTED_EDGE('',*,*,#8595,.T.);
#10996=ORIENTED_EDGE('',*,*,#8589,.T.);
#10997=ORIENTED_EDGE('',*,*,#8596,.T.);
#10998=ORIENTED_EDGE('',*,*,#8547,.F.);
#10999=ORIENTED_EDGE('',*,*,#8597,.F.);
#11000=ORIENTED_EDGE('',*,*,#8598,.F.);
#11001=ORIENTED_EDGE('',*,*,#8599,.T.);
#11002=ORIENTED_EDGE('',*,*,#8600,.T.);
#11003=ORIENTED_EDGE('',*,*,#8601,.T.);
#11004=ORIENTED_EDGE('',*,*,#8599,.F.);
#11005=ORIENTED_EDGE('',*,*,#8602,.T.);
#11006=ORIENTED_EDGE('',*,*,#8597,.T.);
#11007=ORIENTED_EDGE('',*,*,#8551,.T.);
#11008=ORIENTED_EDGE('',*,*,#8587,.T.);
#11009=ORIENTED_EDGE('',*,*,#8603,.T.);
#11010=ORIENTED_EDGE('',*,*,#8598,.T.);
#11011=ORIENTED_EDGE('',*,*,#8604,.T.);
#11012=ORIENTED_EDGE('',*,*,#8605,.F.);
#11013=ORIENTED_EDGE('',*,*,#8606,.F.);
#11014=ORIENTED_EDGE('',*,*,#8607,.F.);
#11015=ORIENTED_EDGE('',*,*,#8608,.T.);
#11016=ORIENTED_EDGE('',*,*,#8498,.T.);
#11017=ORIENTED_EDGE('',*,*,#8606,.T.);
#11018=ORIENTED_EDGE('',*,*,#8609,.T.);
#11019=ORIENTED_EDGE('',*,*,#8608,.F.);
#11020=ORIENTED_EDGE('',*,*,#8610,.T.);
#11021=ORIENTED_EDGE('',*,*,#8611,.T.);
#11022=ORIENTED_EDGE('',*,*,#8612,.T.);
#11023=ORIENTED_EDGE('',*,*,#8555,.T.);
#11024=ORIENTED_EDGE('',*,*,#8607,.T.);
#11025=ORIENTED_EDGE('',*,*,#8497,.T.);
#11026=ORIENTED_EDGE('',*,*,#8512,.F.);
#11027=ORIENTED_EDGE('',*,*,#8613,.T.);
#11028=ORIENTED_EDGE('',*,*,#8605,.T.);
#11029=ORIENTED_EDGE('',*,*,#8554,.T.);
#11030=ORIENTED_EDGE('',*,*,#8541,.F.);
#11031=ORIENTED_EDGE('',*,*,#8614,.T.);
#11032=ORIENTED_EDGE('',*,*,#8615,.T.);
#11033=ORIENTED_EDGE('',*,*,#8616,.T.);
#11034=ORIENTED_EDGE('',*,*,#8536,.F.);
#11035=ORIENTED_EDGE('',*,*,#8617,.T.);
#11036=ORIENTED_EDGE('',*,*,#8614,.F.);
#11037=ORIENTED_EDGE('',*,*,#8618,.T.);
#11038=ORIENTED_EDGE('',*,*,#8514,.F.);
#11039=ORIENTED_EDGE('',*,*,#8543,.F.);
#11040=ORIENTED_EDGE('',*,*,#8545,.F.);
#11041=ORIENTED_EDGE('',*,*,#8612,.F.);
#11042=ORIENTED_EDGE('',*,*,#8619,.T.);
#11043=ORIENTED_EDGE('',*,*,#8553,.F.);
#11044=ORIENTED_EDGE('',*,*,#8585,.F.);
#11045=ORIENTED_EDGE('',*,*,#8596,.F.);
#11046=ORIENTED_EDGE('',*,*,#8593,.F.);
#11047=ORIENTED_EDGE('',*,*,#8620,.F.);
#11048=ORIENTED_EDGE('',*,*,#8621,.T.);
#11049=ORIENTED_EDGE('',*,*,#8622,.T.);
#11050=ORIENTED_EDGE('',*,*,#8623,.T.);
#11051=ORIENTED_EDGE('',*,*,#8624,.T.);
#11052=ORIENTED_EDGE('',*,*,#8625,.T.);
#11053=ORIENTED_EDGE('',*,*,#8626,.T.);
#11054=ORIENTED_EDGE('',*,*,#8627,.T.);
#11055=ORIENTED_EDGE('',*,*,#8628,.T.);
#11056=ORIENTED_EDGE('',*,*,#8629,.T.);
#11057=ORIENTED_EDGE('',*,*,#8630,.T.);
#11058=ORIENTED_EDGE('',*,*,#8631,.T.);
#11059=ORIENTED_EDGE('',*,*,#8632,.T.);
#11060=ORIENTED_EDGE('',*,*,#8633,.T.);
#11061=ORIENTED_EDGE('',*,*,#8634,.T.);
#11062=ORIENTED_EDGE('',*,*,#8635,.T.);
#11063=ORIENTED_EDGE('',*,*,#8636,.T.);
#11064=ORIENTED_EDGE('',*,*,#8637,.T.);
#11065=ORIENTED_EDGE('',*,*,#8638,.T.);
#11066=ORIENTED_EDGE('',*,*,#8639,.T.);
#11067=ORIENTED_EDGE('',*,*,#8640,.T.);
#11068=ORIENTED_EDGE('',*,*,#8641,.T.);
#11069=ORIENTED_EDGE('',*,*,#8642,.T.);
#11070=ORIENTED_EDGE('',*,*,#8643,.T.);
#11071=ORIENTED_EDGE('',*,*,#8644,.T.);
#11072=ORIENTED_EDGE('',*,*,#8645,.T.);
#11073=ORIENTED_EDGE('',*,*,#8646,.T.);
#11074=ORIENTED_EDGE('',*,*,#8647,.T.);
#11075=ORIENTED_EDGE('',*,*,#8648,.T.);
#11076=ORIENTED_EDGE('',*,*,#8649,.T.);
#11077=ORIENTED_EDGE('',*,*,#8650,.T.);
#11078=ORIENTED_EDGE('',*,*,#8651,.T.);
#11079=ORIENTED_EDGE('',*,*,#8652,.T.);
#11080=ORIENTED_EDGE('',*,*,#8653,.T.);
#11081=ORIENTED_EDGE('',*,*,#8654,.T.);
#11082=ORIENTED_EDGE('',*,*,#8655,.T.);
#11083=ORIENTED_EDGE('',*,*,#8656,.T.);
#11084=ORIENTED_EDGE('',*,*,#8657,.T.);
#11085=ORIENTED_EDGE('',*,*,#8658,.T.);
#11086=ORIENTED_EDGE('',*,*,#8659,.T.);
#11087=ORIENTED_EDGE('',*,*,#8660,.T.);
#11088=ORIENTED_EDGE('',*,*,#8661,.T.);
#11089=ORIENTED_EDGE('',*,*,#8662,.T.);
#11090=ORIENTED_EDGE('',*,*,#8663,.T.);
#11091=ORIENTED_EDGE('',*,*,#8664,.T.);
#11092=ORIENTED_EDGE('',*,*,#8665,.T.);
#11093=ORIENTED_EDGE('',*,*,#8594,.F.);
#11094=ORIENTED_EDGE('',*,*,#8604,.F.);
#11095=ORIENTED_EDGE('',*,*,#8602,.F.);
#11096=ORIENTED_EDGE('',*,*,#8666,.F.);
#11097=ORIENTED_EDGE('',*,*,#8591,.F.);
#11098=ORIENTED_EDGE('',*,*,#8666,.T.);
#11099=ORIENTED_EDGE('',*,*,#8601,.F.);
#11100=ORIENTED_EDGE('',*,*,#8495,.T.);
#11101=ORIENTED_EDGE('',*,*,#8600,.F.);
#11102=ORIENTED_EDGE('',*,*,#8550,.T.);
#11103=ORIENTED_EDGE('',*,*,#8619,.F.);
#11104=ORIENTED_EDGE('',*,*,#8496,.T.);
#11105=ORIENTED_EDGE('',*,*,#8611,.F.);
#11106=ORIENTED_EDGE('',*,*,#8667,.T.);
#11107=ORIENTED_EDGE('',*,*,#8668,.F.);
#11108=ORIENTED_EDGE('',*,*,#8499,.T.);
#11109=ORIENTED_EDGE('',*,*,#8515,.F.);
#11110=ORIENTED_EDGE('',*,*,#8618,.F.);
#11111=ORIENTED_EDGE('',*,*,#8669,.F.);
#11112=ORIENTED_EDGE('',*,*,#8609,.F.);
#11113=ORIENTED_EDGE('',*,*,#8613,.F.);
#11114=ORIENTED_EDGE('',*,*,#8610,.F.);
#11115=ORIENTED_EDGE('',*,*,#8669,.T.);
#11116=ORIENTED_EDGE('',*,*,#8616,.F.);
#11117=ORIENTED_EDGE('',*,*,#8670,.T.);
#11118=ORIENTED_EDGE('',*,*,#8615,.F.);
#11119=ORIENTED_EDGE('',*,*,#8671,.T.);
#11120=ORIENTED_EDGE('',*,*,#8672,.F.);
#11121=ORIENTED_EDGE('',*,*,#8673,.T.);
#11122=ORIENTED_EDGE('',*,*,#8584,.F.);
#11123=ORIENTED_EDGE('',*,*,#8620,.T.);
#11124=ORIENTED_EDGE('',*,*,#8592,.F.);
#11125=ORIENTED_EDGE('',*,*,#8494,.T.);
#11126=ORIENTED_EDGE('',*,*,#8483,.F.);
#11127=ORIENTED_EDGE('',*,*,#8505,.T.);
#11128=ORIENTED_EDGE('',*,*,#8674,.T.);
#11129=ORIENTED_EDGE('',*,*,#8675,.T.);
#11130=ORIENTED_EDGE('',*,*,#8487,.F.);
#11131=ORIENTED_EDGE('',*,*,#8492,.F.);
#11132=ORIENTED_EDGE('',*,*,#8675,.F.);
#11133=ORIENTED_EDGE('',*,*,#8676,.T.);
#11134=ORIENTED_EDGE('',*,*,#8564,.F.);
#11135=ORIENTED_EDGE('',*,*,#8569,.F.);
#11136=ORIENTED_EDGE('',*,*,#8677,.T.);
#11137=ORIENTED_EDGE('',*,*,#8562,.F.);
#11138=ORIENTED_EDGE('',*,*,#8678,.T.);
#11139=ORIENTED_EDGE('',*,*,#8679,.T.);
#11140=ORIENTED_EDGE('',*,*,#8482,.T.);
#11141=ORIENTED_EDGE('',*,*,#8563,.F.);
#11142=ORIENTED_EDGE('',*,*,#8481,.T.);
#11143=ORIENTED_EDGE('',*,*,#8680,.T.);
#11144=ORIENTED_EDGE('',*,*,#8570,.T.);
#11145=ORIENTED_EDGE('',*,*,#8559,.F.);
#11146=ORIENTED_EDGE('',*,*,#8566,.F.);
#11147=ORIENTED_EDGE('',*,*,#8681,.T.);
#11148=ORIENTED_EDGE('',*,*,#8678,.F.);
#11149=ORIENTED_EDGE('',*,*,#8682,.F.);
#11150=ORIENTED_EDGE('',*,*,#8683,.F.);
#11151=ORIENTED_EDGE('',*,*,#8684,.F.);
#11152=ORIENTED_EDGE('',*,*,#8685,.T.);
#11153=ORIENTED_EDGE('',*,*,#8479,.T.);
#11154=ORIENTED_EDGE('',*,*,#8683,.T.);
#11155=ORIENTED_EDGE('',*,*,#8686,.T.);
#11156=ORIENTED_EDGE('',*,*,#8687,.T.);
#11157=ORIENTED_EDGE('',*,*,#8688,.T.);
#11158=ORIENTED_EDGE('',*,*,#8684,.T.);
#11159=ORIENTED_EDGE('',*,*,#8478,.T.);
#11160=ORIENTED_EDGE('',*,*,#8689,.T.);
#11161=ORIENTED_EDGE('',*,*,#8690,.T.);
#11162=ORIENTED_EDGE('',*,*,#8691,.T.);
#11163=ORIENTED_EDGE('',*,*,#8689,.F.);
#11164=ORIENTED_EDGE('',*,*,#8692,.T.);
#11165=ORIENTED_EDGE('',*,*,#8682,.T.);
#11166=ORIENTED_EDGE('',*,*,#8693,.T.);
#11167=ORIENTED_EDGE('',*,*,#8686,.F.);
#11168=ORIENTED_EDGE('',*,*,#8692,.F.);
#11169=ORIENTED_EDGE('',*,*,#8694,.F.);
#11170=ORIENTED_EDGE('',*,*,#8695,.T.);
#11171=ORIENTED_EDGE('',*,*,#8691,.F.);
#11172=ORIENTED_EDGE('',*,*,#8696,.T.);
#11173=ORIENTED_EDGE('',*,*,#8697,.T.);
#11174=ORIENTED_EDGE('',*,*,#8694,.T.);
#11175=ORIENTED_EDGE('',*,*,#8690,.F.);
#11176=ORIENTED_EDGE('',*,*,#8698,.T.);
#11177=ORIENTED_EDGE('',*,*,#8699,.T.);
#11178=ORIENTED_EDGE('',*,*,#8700,.T.);
#11179=ORIENTED_EDGE('',*,*,#8696,.F.);
#11180=ORIENTED_EDGE('',*,*,#8700,.F.);
#11181=ORIENTED_EDGE('',*,*,#8701,.T.);
#11182=ORIENTED_EDGE('',*,*,#8702,.T.);
#11183=ORIENTED_EDGE('',*,*,#8703,.T.);
#11184=ORIENTED_EDGE('',*,*,#8704,.T.);
#11185=ORIENTED_EDGE('',*,*,#8705,.T.);
#11186=ORIENTED_EDGE('',*,*,#8703,.F.);
#11187=ORIENTED_EDGE('',*,*,#8705,.F.);
#11188=ORIENTED_EDGE('',*,*,#8706,.T.);
#11189=ORIENTED_EDGE('',*,*,#8707,.F.);
#11190=ORIENTED_EDGE('',*,*,#8708,.F.);
#11191=ORIENTED_EDGE('',*,*,#8706,.F.);
#11192=ORIENTED_EDGE('',*,*,#8704,.F.);
#11193=ORIENTED_EDGE('',*,*,#8702,.F.);
#11194=ORIENTED_EDGE('',*,*,#8709,.T.);
#11195=ORIENTED_EDGE('',*,*,#8707,.T.);
#11196=ORIENTED_EDGE('',*,*,#8708,.T.);
#11197=ORIENTED_EDGE('',*,*,#8710,.T.);
#11198=ORIENTED_EDGE('',*,*,#8711,.T.);
#11199=ORIENTED_EDGE('',*,*,#8712,.T.);
#11200=ORIENTED_EDGE('',*,*,#8710,.F.);
#11201=ORIENTED_EDGE('',*,*,#8712,.F.);
#11202=ORIENTED_EDGE('',*,*,#8713,.T.);
#11203=ORIENTED_EDGE('',*,*,#8714,.F.);
#11204=ORIENTED_EDGE('',*,*,#8681,.F.);
#11205=ORIENTED_EDGE('',*,*,#8565,.F.);
#11206=ORIENTED_EDGE('',*,*,#8677,.F.);
#11207=ORIENTED_EDGE('',*,*,#8568,.F.);
#11208=ORIENTED_EDGE('',*,*,#8571,.F.);
#11209=ORIENTED_EDGE('',*,*,#8715,.F.);
#11210=ORIENTED_EDGE('',*,*,#8695,.F.);
#11211=ORIENTED_EDGE('',*,*,#8697,.F.);
#11212=ORIENTED_EDGE('',*,*,#8701,.F.);
#11213=ORIENTED_EDGE('',*,*,#8699,.F.);
#11214=ORIENTED_EDGE('',*,*,#8716,.F.);
#11215=ORIENTED_EDGE('',*,*,#8717,.F.);
#11216=ORIENTED_EDGE('',*,*,#8718,.F.);
#11217=ORIENTED_EDGE('',*,*,#8577,.F.);
#11218=ORIENTED_EDGE('',*,*,#8719,.F.);
#11219=ORIENTED_EDGE('',*,*,#8575,.F.);
#11220=ORIENTED_EDGE('',*,*,#8508,.F.);
#11221=ORIENTED_EDGE('',*,*,#8490,.F.);
#11222=ORIENTED_EDGE('',*,*,#8676,.F.);
#11223=ORIENTED_EDGE('',*,*,#8674,.F.);
#11224=ORIENTED_EDGE('',*,*,#8504,.F.);
#11225=ORIENTED_EDGE('',*,*,#8720,.F.);
#11226=ORIENTED_EDGE('',*,*,#8713,.F.);
#11227=ORIENTED_EDGE('',*,*,#8711,.F.);
#11228=ORIENTED_EDGE('',*,*,#8480,.T.);
#11229=ORIENTED_EDGE('',*,*,#8685,.F.);
#11230=ORIENTED_EDGE('',*,*,#8715,.T.);
#11231=ORIENTED_EDGE('',*,*,#8680,.F.);
#11232=ORIENTED_EDGE('',*,*,#8721,.T.);
#11233=ORIENTED_EDGE('',*,*,#8722,.T.);
#11234=ORIENTED_EDGE('',*,*,#8723,.T.);
#11235=ORIENTED_EDGE('',*,*,#8724,.T.);
#11236=ORIENTED_EDGE('',*,*,#8672,.T.);
#11237=ORIENTED_EDGE('',*,*,#8725,.T.);
#11238=ORIENTED_EDGE('',*,*,#8723,.F.);
#11239=ORIENTED_EDGE('',*,*,#8726,.T.);
#11240=ORIENTED_EDGE('',*,*,#8727,.T.);
#11241=ORIENTED_EDGE('',*,*,#8728,.T.);
#11242=ORIENTED_EDGE('',*,*,#8729,.T.);
#11243=ORIENTED_EDGE('',*,*,#8501,.T.);
#11244=ORIENTED_EDGE('',*,*,#8730,.T.);
#11245=ORIENTED_EDGE('',*,*,#8502,.T.);
#11246=ORIENTED_EDGE('',*,*,#8729,.F.);
#11247=ORIENTED_EDGE('',*,*,#8731,.T.);
#11248=ORIENTED_EDGE('',*,*,#8503,.T.);
#11249=ORIENTED_EDGE('',*,*,#8730,.F.);
#11250=ORIENTED_EDGE('',*,*,#8474,.T.);
#11251=ORIENTED_EDGE('',*,*,#8732,.T.);
#11252=ORIENTED_EDGE('',*,*,#8668,.T.);
#11253=ORIENTED_EDGE('',*,*,#8733,.T.);
#11254=ORIENTED_EDGE('',*,*,#8727,.F.);
#11255=ORIENTED_EDGE('',*,*,#8500,.T.);
#11256=ORIENTED_EDGE('',*,*,#8473,.T.);
#11257=ORIENTED_EDGE('',*,*,#8679,.F.);
#11258=ORIENTED_EDGE('',*,*,#8714,.T.);
#11259=ORIENTED_EDGE('',*,*,#8720,.T.);
#11260=ORIENTED_EDGE('',*,*,#8732,.F.);
#11261=ORIENTED_EDGE('',*,*,#8734,.T.);
#11262=ORIENTED_EDGE('',*,*,#8735,.T.);
#11263=ORIENTED_EDGE('',*,*,#8721,.F.);
#11264=ORIENTED_EDGE('',*,*,#8736,.T.);
#11265=ORIENTED_EDGE('',*,*,#8476,.T.);
#11266=ORIENTED_EDGE('',*,*,#8734,.F.);
#11267=ORIENTED_EDGE('',*,*,#8737,.T.);
#11268=ORIENTED_EDGE('',*,*,#8738,.T.);
#11269=ORIENTED_EDGE('',*,*,#8717,.T.);
#11270=ORIENTED_EDGE('',*,*,#8687,.F.);
#11271=ORIENTED_EDGE('',*,*,#8477,.T.);
#11272=ORIENTED_EDGE('',*,*,#8738,.F.);
#11273=ORIENTED_EDGE('',*,*,#8667,.F.);
#11274=ORIENTED_EDGE('',*,*,#8670,.F.);
#11275=ORIENTED_EDGE('',*,*,#8673,.F.);
#11276=ORIENTED_EDGE('',*,*,#8739,.F.);
#11277=ORIENTED_EDGE('',*,*,#8740,.T.);
#11278=ORIENTED_EDGE('',*,*,#8733,.F.);
#11279=ORIENTED_EDGE('',*,*,#8739,.T.);
#11280=ORIENTED_EDGE('',*,*,#8726,.F.);
#11281=ORIENTED_EDGE('',*,*,#8741,.T.);
#11282=ORIENTED_EDGE('',*,*,#8728,.F.);
#11283=ORIENTED_EDGE('',*,*,#8741,.F.);
#11284=ORIENTED_EDGE('',*,*,#8722,.F.);
#11285=ORIENTED_EDGE('',*,*,#8742,.F.);
#11286=ORIENTED_EDGE('',*,*,#8731,.F.);
#11287=ORIENTED_EDGE('',*,*,#8742,.T.);
#11288=ORIENTED_EDGE('',*,*,#8735,.F.);
#11289=ORIENTED_EDGE('',*,*,#8475,.T.);
#11290=ORIENTED_EDGE('',*,*,#8621,.F.);
#11291=ORIENTED_EDGE('',*,*,#8743,.T.);
#11292=ORIENTED_EDGE('',*,*,#8744,.T.);
#11293=ORIENTED_EDGE('',*,*,#8745,.F.);
#11294=ORIENTED_EDGE('',*,*,#8631,.F.);
#11295=ORIENTED_EDGE('',*,*,#8746,.T.);
#11296=ORIENTED_EDGE('',*,*,#8747,.T.);
#11297=ORIENTED_EDGE('',*,*,#8743,.F.);
#11298=ORIENTED_EDGE('',*,*,#8630,.F.);
#11299=ORIENTED_EDGE('',*,*,#8748,.T.);
#11300=ORIENTED_EDGE('',*,*,#8749,.T.);
#11301=ORIENTED_EDGE('',*,*,#8746,.F.);
#11302=ORIENTED_EDGE('',*,*,#8629,.F.);
#11303=ORIENTED_EDGE('',*,*,#8750,.T.);
#11304=ORIENTED_EDGE('',*,*,#8751,.T.);
#11305=ORIENTED_EDGE('',*,*,#8748,.F.);
#11306=ORIENTED_EDGE('',*,*,#8628,.F.);
#11307=ORIENTED_EDGE('',*,*,#8752,.T.);
#11308=ORIENTED_EDGE('',*,*,#8753,.T.);
#11309=ORIENTED_EDGE('',*,*,#8750,.F.);
#11310=ORIENTED_EDGE('',*,*,#8627,.F.);
#11311=ORIENTED_EDGE('',*,*,#8754,.T.);
#11312=ORIENTED_EDGE('',*,*,#8755,.T.);
#11313=ORIENTED_EDGE('',*,*,#8752,.F.);
#11314=ORIENTED_EDGE('',*,*,#8626,.F.);
#11315=ORIENTED_EDGE('',*,*,#8756,.T.);
#11316=ORIENTED_EDGE('',*,*,#8757,.T.);
#11317=ORIENTED_EDGE('',*,*,#8754,.F.);
#11318=ORIENTED_EDGE('',*,*,#8625,.F.);
#11319=ORIENTED_EDGE('',*,*,#8758,.T.);
#11320=ORIENTED_EDGE('',*,*,#8759,.T.);
#11321=ORIENTED_EDGE('',*,*,#8756,.F.);
#11322=ORIENTED_EDGE('',*,*,#8624,.F.);
#11323=ORIENTED_EDGE('',*,*,#8760,.T.);
#11324=ORIENTED_EDGE('',*,*,#8761,.T.);
#11325=ORIENTED_EDGE('',*,*,#8758,.F.);
#11326=ORIENTED_EDGE('',*,*,#8623,.F.);
#11327=ORIENTED_EDGE('',*,*,#8762,.T.);
#11328=ORIENTED_EDGE('',*,*,#8763,.T.);
#11329=ORIENTED_EDGE('',*,*,#8760,.F.);
#11330=ORIENTED_EDGE('',*,*,#8622,.F.);
#11331=ORIENTED_EDGE('',*,*,#8745,.T.);
#11332=ORIENTED_EDGE('',*,*,#8764,.T.);
#11333=ORIENTED_EDGE('',*,*,#8762,.F.);
#11334=ORIENTED_EDGE('',*,*,#8764,.F.);
#11335=ORIENTED_EDGE('',*,*,#8744,.F.);
#11336=ORIENTED_EDGE('',*,*,#8747,.F.);
#11337=ORIENTED_EDGE('',*,*,#8749,.F.);
#11338=ORIENTED_EDGE('',*,*,#8751,.F.);
#11339=ORIENTED_EDGE('',*,*,#8753,.F.);
#11340=ORIENTED_EDGE('',*,*,#8755,.F.);
#11341=ORIENTED_EDGE('',*,*,#8757,.F.);
#11342=ORIENTED_EDGE('',*,*,#8759,.F.);
#11343=ORIENTED_EDGE('',*,*,#8761,.F.);
#11344=ORIENTED_EDGE('',*,*,#8763,.F.);
#11345=ORIENTED_EDGE('',*,*,#8632,.F.);
#11346=ORIENTED_EDGE('',*,*,#8765,.T.);
#11347=ORIENTED_EDGE('',*,*,#8766,.T.);
#11348=ORIENTED_EDGE('',*,*,#8767,.F.);
#11349=ORIENTED_EDGE('',*,*,#8639,.F.);
#11350=ORIENTED_EDGE('',*,*,#8768,.T.);
#11351=ORIENTED_EDGE('',*,*,#8769,.T.);
#11352=ORIENTED_EDGE('',*,*,#8765,.F.);
#11353=ORIENTED_EDGE('',*,*,#8638,.F.);
#11354=ORIENTED_EDGE('',*,*,#8770,.T.);
#11355=ORIENTED_EDGE('',*,*,#8771,.T.);
#11356=ORIENTED_EDGE('',*,*,#8768,.F.);
#11357=ORIENTED_EDGE('',*,*,#8637,.F.);
#11358=ORIENTED_EDGE('',*,*,#8772,.T.);
#11359=ORIENTED_EDGE('',*,*,#8773,.T.);
#11360=ORIENTED_EDGE('',*,*,#8770,.F.);
#11361=ORIENTED_EDGE('',*,*,#8636,.F.);
#11362=ORIENTED_EDGE('',*,*,#8774,.T.);
#11363=ORIENTED_EDGE('',*,*,#8775,.T.);
#11364=ORIENTED_EDGE('',*,*,#8772,.F.);
#11365=ORIENTED_EDGE('',*,*,#8635,.F.);
#11366=ORIENTED_EDGE('',*,*,#8776,.T.);
#11367=ORIENTED_EDGE('',*,*,#8777,.T.);
#11368=ORIENTED_EDGE('',*,*,#8774,.F.);
#11369=ORIENTED_EDGE('',*,*,#8634,.F.);
#11370=ORIENTED_EDGE('',*,*,#8778,.T.);
#11371=ORIENTED_EDGE('',*,*,#8779,.T.);
#11372=ORIENTED_EDGE('',*,*,#8776,.F.);
#11373=ORIENTED_EDGE('',*,*,#8633,.F.);
#11374=ORIENTED_EDGE('',*,*,#8767,.T.);
#11375=ORIENTED_EDGE('',*,*,#8780,.T.);
#11376=ORIENTED_EDGE('',*,*,#8778,.F.);
#11377=ORIENTED_EDGE('',*,*,#8780,.F.);
#11378=ORIENTED_EDGE('',*,*,#8766,.F.);
#11379=ORIENTED_EDGE('',*,*,#8769,.F.);
#11380=ORIENTED_EDGE('',*,*,#8771,.F.);
#11381=ORIENTED_EDGE('',*,*,#8773,.F.);
#11382=ORIENTED_EDGE('',*,*,#8775,.F.);
#11383=ORIENTED_EDGE('',*,*,#8777,.F.);
#11384=ORIENTED_EDGE('',*,*,#8779,.F.);
#11385=ORIENTED_EDGE('',*,*,#8640,.F.);
#11386=ORIENTED_EDGE('',*,*,#8781,.T.);
#11387=ORIENTED_EDGE('',*,*,#8782,.T.);
#11388=ORIENTED_EDGE('',*,*,#8783,.F.);
#11389=ORIENTED_EDGE('',*,*,#8655,.F.);
#11390=ORIENTED_EDGE('',*,*,#8784,.T.);
#11391=ORIENTED_EDGE('',*,*,#8785,.T.);
#11392=ORIENTED_EDGE('',*,*,#8781,.F.);
#11393=ORIENTED_EDGE('',*,*,#8654,.F.);
#11394=ORIENTED_EDGE('',*,*,#8786,.T.);
#11395=ORIENTED_EDGE('',*,*,#8787,.T.);
#11396=ORIENTED_EDGE('',*,*,#8784,.F.);
#11397=ORIENTED_EDGE('',*,*,#8653,.F.);
#11398=ORIENTED_EDGE('',*,*,#8788,.T.);
#11399=ORIENTED_EDGE('',*,*,#8789,.T.);
#11400=ORIENTED_EDGE('',*,*,#8786,.F.);
#11401=ORIENTED_EDGE('',*,*,#8652,.F.);
#11402=ORIENTED_EDGE('',*,*,#8790,.T.);
#11403=ORIENTED_EDGE('',*,*,#8791,.T.);
#11404=ORIENTED_EDGE('',*,*,#8788,.F.);
#11405=ORIENTED_EDGE('',*,*,#8651,.F.);
#11406=ORIENTED_EDGE('',*,*,#8792,.T.);
#11407=ORIENTED_EDGE('',*,*,#8793,.T.);
#11408=ORIENTED_EDGE('',*,*,#8790,.F.);
#11409=ORIENTED_EDGE('',*,*,#8650,.F.);
#11410=ORIENTED_EDGE('',*,*,#8794,.T.);
#11411=ORIENTED_EDGE('',*,*,#8795,.T.);
#11412=ORIENTED_EDGE('',*,*,#8792,.F.);
#11413=ORIENTED_EDGE('',*,*,#8649,.F.);
#11414=ORIENTED_EDGE('',*,*,#8796,.T.);
#11415=ORIENTED_EDGE('',*,*,#8797,.T.);
#11416=ORIENTED_EDGE('',*,*,#8794,.F.);
#11417=ORIENTED_EDGE('',*,*,#8648,.F.);
#11418=ORIENTED_EDGE('',*,*,#8798,.T.);
#11419=ORIENTED_EDGE('',*,*,#8799,.T.);
#11420=ORIENTED_EDGE('',*,*,#8796,.F.);
#11421=ORIENTED_EDGE('',*,*,#8647,.F.);
#11422=ORIENTED_EDGE('',*,*,#8800,.T.);
#11423=ORIENTED_EDGE('',*,*,#8801,.T.);
#11424=ORIENTED_EDGE('',*,*,#8798,.F.);
#11425=ORIENTED_EDGE('',*,*,#8646,.F.);
#11426=ORIENTED_EDGE('',*,*,#8802,.T.);
#11427=ORIENTED_EDGE('',*,*,#8803,.T.);
#11428=ORIENTED_EDGE('',*,*,#8800,.F.);
#11429=ORIENTED_EDGE('',*,*,#8645,.F.);
#11430=ORIENTED_EDGE('',*,*,#8804,.T.);
#11431=ORIENTED_EDGE('',*,*,#8805,.T.);
#11432=ORIENTED_EDGE('',*,*,#8802,.F.);
#11433=ORIENTED_EDGE('',*,*,#8644,.F.);
#11434=ORIENTED_EDGE('',*,*,#8806,.T.);
#11435=ORIENTED_EDGE('',*,*,#8807,.T.);
#11436=ORIENTED_EDGE('',*,*,#8804,.F.);
#11437=ORIENTED_EDGE('',*,*,#8643,.F.);
#11438=ORIENTED_EDGE('',*,*,#8808,.T.);
#11439=ORIENTED_EDGE('',*,*,#8809,.T.);
#11440=ORIENTED_EDGE('',*,*,#8806,.F.);
#11441=ORIENTED_EDGE('',*,*,#8642,.F.);
#11442=ORIENTED_EDGE('',*,*,#8810,.T.);
#11443=ORIENTED_EDGE('',*,*,#8811,.T.);
#11444=ORIENTED_EDGE('',*,*,#8808,.F.);
#11445=ORIENTED_EDGE('',*,*,#8641,.F.);
#11446=ORIENTED_EDGE('',*,*,#8783,.T.);
#11447=ORIENTED_EDGE('',*,*,#8812,.T.);
#11448=ORIENTED_EDGE('',*,*,#8810,.F.);
#11449=ORIENTED_EDGE('',*,*,#8812,.F.);
#11450=ORIENTED_EDGE('',*,*,#8782,.F.);
#11451=ORIENTED_EDGE('',*,*,#8785,.F.);
#11452=ORIENTED_EDGE('',*,*,#8787,.F.);
#11453=ORIENTED_EDGE('',*,*,#8789,.F.);
#11454=ORIENTED_EDGE('',*,*,#8791,.F.);
#11455=ORIENTED_EDGE('',*,*,#8793,.F.);
#11456=ORIENTED_EDGE('',*,*,#8795,.F.);
#11457=ORIENTED_EDGE('',*,*,#8797,.F.);
#11458=ORIENTED_EDGE('',*,*,#8799,.F.);
#11459=ORIENTED_EDGE('',*,*,#8801,.F.);
#11460=ORIENTED_EDGE('',*,*,#8803,.F.);
#11461=ORIENTED_EDGE('',*,*,#8805,.F.);
#11462=ORIENTED_EDGE('',*,*,#8807,.F.);
#11463=ORIENTED_EDGE('',*,*,#8809,.F.);
#11464=ORIENTED_EDGE('',*,*,#8811,.F.);
#11465=ORIENTED_EDGE('',*,*,#8656,.F.);
#11466=ORIENTED_EDGE('',*,*,#8813,.T.);
#11467=ORIENTED_EDGE('',*,*,#8814,.T.);
#11468=ORIENTED_EDGE('',*,*,#8815,.F.);
#11469=ORIENTED_EDGE('',*,*,#8665,.F.);
#11470=ORIENTED_EDGE('',*,*,#8816,.T.);
#11471=ORIENTED_EDGE('',*,*,#8817,.T.);
#11472=ORIENTED_EDGE('',*,*,#8813,.F.);
#11473=ORIENTED_EDGE('',*,*,#8664,.F.);
#11474=ORIENTED_EDGE('',*,*,#8818,.T.);
#11475=ORIENTED_EDGE('',*,*,#8819,.T.);
#11476=ORIENTED_EDGE('',*,*,#8816,.F.);
#11477=ORIENTED_EDGE('',*,*,#8663,.F.);
#11478=ORIENTED_EDGE('',*,*,#8820,.T.);
#11479=ORIENTED_EDGE('',*,*,#8821,.T.);
#11480=ORIENTED_EDGE('',*,*,#8818,.F.);
#11481=ORIENTED_EDGE('',*,*,#8662,.F.);
#11482=ORIENTED_EDGE('',*,*,#8822,.T.);
#11483=ORIENTED_EDGE('',*,*,#8823,.T.);
#11484=ORIENTED_EDGE('',*,*,#8820,.F.);
#11485=ORIENTED_EDGE('',*,*,#8661,.F.);
#11486=ORIENTED_EDGE('',*,*,#8824,.T.);
#11487=ORIENTED_EDGE('',*,*,#8825,.T.);
#11488=ORIENTED_EDGE('',*,*,#8822,.F.);
#11489=ORIENTED_EDGE('',*,*,#8660,.F.);
#11490=ORIENTED_EDGE('',*,*,#8826,.T.);
#11491=ORIENTED_EDGE('',*,*,#8827,.T.);
#11492=ORIENTED_EDGE('',*,*,#8824,.F.);
#11493=ORIENTED_EDGE('',*,*,#8659,.F.);
#11494=ORIENTED_EDGE('',*,*,#8828,.T.);
#11495=ORIENTED_EDGE('',*,*,#8829,.T.);
#11496=ORIENTED_EDGE('',*,*,#8826,.F.);
#11497=ORIENTED_EDGE('',*,*,#8658,.F.);
#11498=ORIENTED_EDGE('',*,*,#8830,.T.);
#11499=ORIENTED_EDGE('',*,*,#8831,.T.);
#11500=ORIENTED_EDGE('',*,*,#8828,.F.);
#11501=ORIENTED_EDGE('',*,*,#8657,.F.);
#11502=ORIENTED_EDGE('',*,*,#8815,.T.);
#11503=ORIENTED_EDGE('',*,*,#8832,.T.);
#11504=ORIENTED_EDGE('',*,*,#8830,.F.);
#11505=ORIENTED_EDGE('',*,*,#8832,.F.);
#11506=ORIENTED_EDGE('',*,*,#8814,.F.);
#11507=ORIENTED_EDGE('',*,*,#8817,.F.);
#11508=ORIENTED_EDGE('',*,*,#8819,.F.);
#11509=ORIENTED_EDGE('',*,*,#8821,.F.);
#11510=ORIENTED_EDGE('',*,*,#8823,.F.);
#11511=ORIENTED_EDGE('',*,*,#8825,.F.);
#11512=ORIENTED_EDGE('',*,*,#8827,.F.);
#11513=ORIENTED_EDGE('',*,*,#8829,.F.);
#11514=ORIENTED_EDGE('',*,*,#8831,.F.);
#11515=ORIENTED_EDGE('',*,*,#8740,.F.);
#11516=ORIENTED_EDGE('',*,*,#8833,.T.);
#11517=ORIENTED_EDGE('',*,*,#8834,.T.);
#11518=ORIENTED_EDGE('',*,*,#8833,.F.);
#11519=ORIENTED_EDGE('',*,*,#8834,.F.);
#11520=ORIENTED_EDGE('',*,*,#8835,.F.);
#11521=ORIENTED_EDGE('',*,*,#8836,.T.);
#11522=ORIENTED_EDGE('',*,*,#8709,.F.);
#11523=ORIENTED_EDGE('',*,*,#8836,.F.);
#11524=ORIENTED_EDGE('',*,*,#8470,.F.);
#11525=ORIENTED_EDGE('',*,*,#8837,.T.);
#11526=ORIENTED_EDGE('',*,*,#8835,.T.);
#11527=ORIENTED_EDGE('',*,*,#8837,.F.);
#11528=ORIENTED_EDGE('',*,*,#8534,.F.);
#11529=ORIENTED_EDGE('',*,*,#8548,.F.);
#11530=ORIENTED_EDGE('',*,*,#8603,.F.);
#11531=ORIENTED_EDGE('',*,*,#8595,.F.);
#11532=ORIENTED_EDGE('',*,*,#8586,.F.);
#11533=ORIENTED_EDGE('',*,*,#8578,.F.);
#11534=ORIENTED_EDGE('',*,*,#8718,.T.);
#11535=ORIENTED_EDGE('',*,*,#8737,.F.);
#11536=ORIENTED_EDGE('',*,*,#8736,.F.);
#11537=ORIENTED_EDGE('',*,*,#8724,.F.);
#11538=ORIENTED_EDGE('',*,*,#8725,.F.);
#11539=ORIENTED_EDGE('',*,*,#8671,.F.);
#11540=ORIENTED_EDGE('',*,*,#8617,.F.);
#11541=ORIENTED_EDGE('',*,*,#8540,.F.);
#11542=ORIENTED_EDGE('',*,*,#8530,.F.);
#11543=ORIENTED_EDGE('',*,*,#8576,.F.);
#11544=ORIENTED_EDGE('',*,*,#8719,.T.);
#11545=ORIENTED_EDGE('',*,*,#8579,.F.);
#11546=ORIENTED_EDGE('',*,*,#8688,.F.);
#11547=ORIENTED_EDGE('',*,*,#8716,.T.);
#11548=ORIENTED_EDGE('',*,*,#8698,.F.);
#11549=ORIENTED_EDGE('',*,*,#8693,.F.);
#11550=ORIENTED_EDGE('',*,*,#8838,.F.);
#11551=ORIENTED_EDGE('',*,*,#8839,.T.);
#11552=ORIENTED_EDGE('',*,*,#8840,.T.);
#11553=ORIENTED_EDGE('',*,*,#8841,.T.);
#11554=ORIENTED_EDGE('',*,*,#8842,.F.);
#11555=ORIENTED_EDGE('',*,*,#8843,.T.);
#11556=ORIENTED_EDGE('',*,*,#8838,.T.);
#11557=ORIENTED_EDGE('',*,*,#8844,.T.);
#11558=ORIENTED_EDGE('',*,*,#8845,.F.);
#11559=ORIENTED_EDGE('',*,*,#8846,.T.);
#11560=ORIENTED_EDGE('',*,*,#8842,.T.);
#11561=ORIENTED_EDGE('',*,*,#8847,.T.);
#11562=ORIENTED_EDGE('',*,*,#8848,.F.);
#11563=ORIENTED_EDGE('',*,*,#8849,.T.);
#11564=ORIENTED_EDGE('',*,*,#8845,.T.);
#11565=ORIENTED_EDGE('',*,*,#8850,.T.);
#11566=ORIENTED_EDGE('',*,*,#8851,.F.);
#11567=ORIENTED_EDGE('',*,*,#8852,.T.);
#11568=ORIENTED_EDGE('',*,*,#8848,.T.);
#11569=ORIENTED_EDGE('',*,*,#8853,.T.);
#11570=ORIENTED_EDGE('',*,*,#8854,.F.);
#11571=ORIENTED_EDGE('',*,*,#8855,.T.);
#11572=ORIENTED_EDGE('',*,*,#8851,.T.);
#11573=ORIENTED_EDGE('',*,*,#8856,.T.);
#11574=ORIENTED_EDGE('',*,*,#8857,.F.);
#11575=ORIENTED_EDGE('',*,*,#8858,.T.);
#11576=ORIENTED_EDGE('',*,*,#8854,.T.);
#11577=ORIENTED_EDGE('',*,*,#8859,.T.);
#11578=ORIENTED_EDGE('',*,*,#8860,.F.);
#11579=ORIENTED_EDGE('',*,*,#8861,.T.);
#11580=ORIENTED_EDGE('',*,*,#8857,.T.);
#11581=ORIENTED_EDGE('',*,*,#8862,.T.);
#11582=ORIENTED_EDGE('',*,*,#8863,.F.);
#11583=ORIENTED_EDGE('',*,*,#8864,.T.);
#11584=ORIENTED_EDGE('',*,*,#8860,.T.);
#11585=ORIENTED_EDGE('',*,*,#8865,.T.);
#11586=ORIENTED_EDGE('',*,*,#8866,.F.);
#11587=ORIENTED_EDGE('',*,*,#8867,.T.);
#11588=ORIENTED_EDGE('',*,*,#8863,.T.);
#11589=ORIENTED_EDGE('',*,*,#8868,.T.);
#11590=ORIENTED_EDGE('',*,*,#8869,.F.);
#11591=ORIENTED_EDGE('',*,*,#8870,.T.);
#11592=ORIENTED_EDGE('',*,*,#8866,.T.);
#11593=ORIENTED_EDGE('',*,*,#8871,.T.);
#11594=ORIENTED_EDGE('',*,*,#8872,.F.);
#11595=ORIENTED_EDGE('',*,*,#8873,.T.);
#11596=ORIENTED_EDGE('',*,*,#8869,.T.);
#11597=ORIENTED_EDGE('',*,*,#8874,.T.);
#11598=ORIENTED_EDGE('',*,*,#8875,.F.);
#11599=ORIENTED_EDGE('',*,*,#8876,.T.);
#11600=ORIENTED_EDGE('',*,*,#8872,.T.);
#11601=ORIENTED_EDGE('',*,*,#8877,.T.);
#11602=ORIENTED_EDGE('',*,*,#8878,.F.);
#11603=ORIENTED_EDGE('',*,*,#8879,.T.);
#11604=ORIENTED_EDGE('',*,*,#8875,.T.);
#11605=ORIENTED_EDGE('',*,*,#8880,.T.);
#11606=ORIENTED_EDGE('',*,*,#8881,.F.);
#11607=ORIENTED_EDGE('',*,*,#8882,.T.);
#11608=ORIENTED_EDGE('',*,*,#8878,.T.);
#11609=ORIENTED_EDGE('',*,*,#8883,.T.);
#11610=ORIENTED_EDGE('',*,*,#8884,.F.);
#11611=ORIENTED_EDGE('',*,*,#8885,.T.);
#11612=ORIENTED_EDGE('',*,*,#8881,.T.);
#11613=ORIENTED_EDGE('',*,*,#8886,.T.);
#11614=ORIENTED_EDGE('',*,*,#8887,.F.);
#11615=ORIENTED_EDGE('',*,*,#8888,.T.);
#11616=ORIENTED_EDGE('',*,*,#8889,.F.);
#11617=ORIENTED_EDGE('',*,*,#8890,.F.);
#11618=ORIENTED_EDGE('',*,*,#8891,.F.);
#11619=ORIENTED_EDGE('',*,*,#8892,.T.);
#11620=ORIENTED_EDGE('',*,*,#8887,.T.);
#11621=ORIENTED_EDGE('',*,*,#8893,.F.);
#11622=ORIENTED_EDGE('',*,*,#8894,.F.);
#11623=ORIENTED_EDGE('',*,*,#8895,.T.);
#11624=ORIENTED_EDGE('',*,*,#8891,.T.);
#11625=ORIENTED_EDGE('',*,*,#8896,.F.);
#11626=ORIENTED_EDGE('',*,*,#8897,.F.);
#11627=ORIENTED_EDGE('',*,*,#8898,.T.);
#11628=ORIENTED_EDGE('',*,*,#8894,.T.);
#11629=ORIENTED_EDGE('',*,*,#8899,.F.);
#11630=ORIENTED_EDGE('',*,*,#8900,.F.);
#11631=ORIENTED_EDGE('',*,*,#8901,.T.);
#11632=ORIENTED_EDGE('',*,*,#8897,.T.);
#11633=ORIENTED_EDGE('',*,*,#8902,.F.);
#11634=ORIENTED_EDGE('',*,*,#8903,.F.);
#11635=ORIENTED_EDGE('',*,*,#8904,.T.);
#11636=ORIENTED_EDGE('',*,*,#8900,.T.);
#11637=ORIENTED_EDGE('',*,*,#8905,.F.);
#11638=ORIENTED_EDGE('',*,*,#8906,.F.);
#11639=ORIENTED_EDGE('',*,*,#8907,.T.);
#11640=ORIENTED_EDGE('',*,*,#8903,.T.);
#11641=ORIENTED_EDGE('',*,*,#8908,.F.);
#11642=ORIENTED_EDGE('',*,*,#8909,.F.);
#11643=ORIENTED_EDGE('',*,*,#8910,.T.);
#11644=ORIENTED_EDGE('',*,*,#8906,.T.);
#11645=ORIENTED_EDGE('',*,*,#8911,.F.);
#11646=ORIENTED_EDGE('',*,*,#8912,.F.);
#11647=ORIENTED_EDGE('',*,*,#8913,.T.);
#11648=ORIENTED_EDGE('',*,*,#8909,.T.);
#11649=ORIENTED_EDGE('',*,*,#8914,.F.);
#11650=ORIENTED_EDGE('',*,*,#8915,.F.);
#11651=ORIENTED_EDGE('',*,*,#8916,.T.);
#11652=ORIENTED_EDGE('',*,*,#8912,.T.);
#11653=ORIENTED_EDGE('',*,*,#8917,.F.);
#11654=ORIENTED_EDGE('',*,*,#8918,.F.);
#11655=ORIENTED_EDGE('',*,*,#8919,.T.);
#11656=ORIENTED_EDGE('',*,*,#8915,.T.);
#11657=ORIENTED_EDGE('',*,*,#8920,.F.);
#11658=ORIENTED_EDGE('',*,*,#8921,.F.);
#11659=ORIENTED_EDGE('',*,*,#8922,.T.);
#11660=ORIENTED_EDGE('',*,*,#8918,.T.);
#11661=ORIENTED_EDGE('',*,*,#8923,.F.);
#11662=ORIENTED_EDGE('',*,*,#8924,.F.);
#11663=ORIENTED_EDGE('',*,*,#8925,.T.);
#11664=ORIENTED_EDGE('',*,*,#8921,.T.);
#11665=ORIENTED_EDGE('',*,*,#8926,.F.);
#11666=ORIENTED_EDGE('',*,*,#8927,.F.);
#11667=ORIENTED_EDGE('',*,*,#8928,.T.);
#11668=ORIENTED_EDGE('',*,*,#8924,.T.);
#11669=ORIENTED_EDGE('',*,*,#8929,.F.);
#11670=ORIENTED_EDGE('',*,*,#8930,.F.);
#11671=ORIENTED_EDGE('',*,*,#8931,.T.);
#11672=ORIENTED_EDGE('',*,*,#8927,.T.);
#11673=ORIENTED_EDGE('',*,*,#8932,.F.);
#11674=ORIENTED_EDGE('',*,*,#8933,.F.);
#11675=ORIENTED_EDGE('',*,*,#8934,.T.);
#11676=ORIENTED_EDGE('',*,*,#8935,.T.);
#11677=ORIENTED_EDGE('',*,*,#8936,.T.);
#11678=ORIENTED_EDGE('',*,*,#8937,.F.);
#11679=ORIENTED_EDGE('',*,*,#8938,.T.);
#11680=ORIENTED_EDGE('',*,*,#8933,.T.);
#11681=ORIENTED_EDGE('',*,*,#8939,.T.);
#11682=ORIENTED_EDGE('',*,*,#8940,.F.);
#11683=ORIENTED_EDGE('',*,*,#8941,.T.);
#11684=ORIENTED_EDGE('',*,*,#8937,.T.);
#11685=ORIENTED_EDGE('',*,*,#8942,.T.);
#11686=ORIENTED_EDGE('',*,*,#8943,.F.);
#11687=ORIENTED_EDGE('',*,*,#8944,.T.);
#11688=ORIENTED_EDGE('',*,*,#8940,.T.);
#11689=ORIENTED_EDGE('',*,*,#8945,.T.);
#11690=ORIENTED_EDGE('',*,*,#8946,.F.);
#11691=ORIENTED_EDGE('',*,*,#8947,.T.);
#11692=ORIENTED_EDGE('',*,*,#8943,.T.);
#11693=ORIENTED_EDGE('',*,*,#8948,.T.);
#11694=ORIENTED_EDGE('',*,*,#8949,.F.);
#11695=ORIENTED_EDGE('',*,*,#8950,.T.);
#11696=ORIENTED_EDGE('',*,*,#8946,.T.);
#11697=ORIENTED_EDGE('',*,*,#8951,.T.);
#11698=ORIENTED_EDGE('',*,*,#8952,.F.);
#11699=ORIENTED_EDGE('',*,*,#8953,.T.);
#11700=ORIENTED_EDGE('',*,*,#8949,.T.);
#11701=ORIENTED_EDGE('',*,*,#8954,.T.);
#11702=ORIENTED_EDGE('',*,*,#8955,.F.);
#11703=ORIENTED_EDGE('',*,*,#8956,.T.);
#11704=ORIENTED_EDGE('',*,*,#8952,.T.);
#11705=ORIENTED_EDGE('',*,*,#8957,.T.);
#11706=ORIENTED_EDGE('',*,*,#8958,.F.);
#11707=ORIENTED_EDGE('',*,*,#8959,.T.);
#11708=ORIENTED_EDGE('',*,*,#8955,.T.);
#11709=ORIENTED_EDGE('',*,*,#8960,.T.);
#11710=ORIENTED_EDGE('',*,*,#8961,.F.);
#11711=ORIENTED_EDGE('',*,*,#8962,.T.);
#11712=ORIENTED_EDGE('',*,*,#8958,.T.);
#11713=ORIENTED_EDGE('',*,*,#8963,.T.);
#11714=ORIENTED_EDGE('',*,*,#8964,.F.);
#11715=ORIENTED_EDGE('',*,*,#8965,.F.);
#11716=ORIENTED_EDGE('',*,*,#8966,.T.);
#11717=ORIENTED_EDGE('',*,*,#8961,.T.);
#11718=ORIENTED_EDGE('',*,*,#8967,.T.);
#11719=ORIENTED_EDGE('',*,*,#8968,.F.);
#11720=ORIENTED_EDGE('',*,*,#8969,.T.);
#11721=ORIENTED_EDGE('',*,*,#8970,.F.);
#11722=ORIENTED_EDGE('',*,*,#8971,.F.);
#11723=ORIENTED_EDGE('',*,*,#8972,.F.);
#11724=ORIENTED_EDGE('',*,*,#8973,.T.);
#11725=ORIENTED_EDGE('',*,*,#8968,.T.);
#11726=ORIENTED_EDGE('',*,*,#8974,.F.);
#11727=ORIENTED_EDGE('',*,*,#8975,.F.);
#11728=ORIENTED_EDGE('',*,*,#8976,.T.);
#11729=ORIENTED_EDGE('',*,*,#8972,.T.);
#11730=ORIENTED_EDGE('',*,*,#8977,.F.);
#11731=ORIENTED_EDGE('',*,*,#8978,.F.);
#11732=ORIENTED_EDGE('',*,*,#8979,.T.);
#11733=ORIENTED_EDGE('',*,*,#8975,.T.);
#11734=ORIENTED_EDGE('',*,*,#8980,.F.);
#11735=ORIENTED_EDGE('',*,*,#8981,.F.);
#11736=ORIENTED_EDGE('',*,*,#8982,.T.);
#11737=ORIENTED_EDGE('',*,*,#8978,.T.);
#11738=ORIENTED_EDGE('',*,*,#8983,.F.);
#11739=ORIENTED_EDGE('',*,*,#8984,.F.);
#11740=ORIENTED_EDGE('',*,*,#8985,.T.);
#11741=ORIENTED_EDGE('',*,*,#8981,.T.);
#11742=ORIENTED_EDGE('',*,*,#8986,.F.);
#11743=ORIENTED_EDGE('',*,*,#8987,.F.);
#11744=ORIENTED_EDGE('',*,*,#8988,.T.);
#11745=ORIENTED_EDGE('',*,*,#8984,.T.);
#11746=ORIENTED_EDGE('',*,*,#8989,.F.);
#11747=ORIENTED_EDGE('',*,*,#8990,.F.);
#11748=ORIENTED_EDGE('',*,*,#8991,.T.);
#11749=ORIENTED_EDGE('',*,*,#8987,.T.);
#11750=ORIENTED_EDGE('',*,*,#8992,.F.);
#11751=ORIENTED_EDGE('',*,*,#8993,.F.);
#11752=ORIENTED_EDGE('',*,*,#8994,.T.);
#11753=ORIENTED_EDGE('',*,*,#8990,.T.);
#11754=ORIENTED_EDGE('',*,*,#8995,.F.);
#11755=ORIENTED_EDGE('',*,*,#8996,.F.);
#11756=ORIENTED_EDGE('',*,*,#8997,.T.);
#11757=ORIENTED_EDGE('',*,*,#8993,.T.);
#11758=ORIENTED_EDGE('',*,*,#8998,.F.);
#11759=ORIENTED_EDGE('',*,*,#8999,.T.);
#11760=ORIENTED_EDGE('',*,*,#9000,.T.);
#11761=ORIENTED_EDGE('',*,*,#9001,.T.);
#11762=ORIENTED_EDGE('',*,*,#9002,.T.);
#11763=ORIENTED_EDGE('',*,*,#9000,.F.);
#11764=ORIENTED_EDGE('',*,*,#9003,.F.);
#11765=ORIENTED_EDGE('',*,*,#9004,.F.);
#11766=ORIENTED_EDGE('',*,*,#9005,.T.);
#11767=ORIENTED_EDGE('',*,*,#9001,.F.);
#11768=ORIENTED_EDGE('',*,*,#9002,.F.);
#11769=ORIENTED_EDGE('',*,*,#9005,.F.);
#11770=ORIENTED_EDGE('',*,*,#9006,.F.);
#11771=ORIENTED_EDGE('',*,*,#8999,.F.);
#11772=ORIENTED_EDGE('',*,*,#9003,.T.);
#11773=ORIENTED_EDGE('',*,*,#9004,.T.);
#11774=ORIENTED_EDGE('',*,*,#9007,.T.);
#11775=ORIENTED_EDGE('',*,*,#9008,.T.);
#11776=ORIENTED_EDGE('',*,*,#9007,.F.);
#11777=ORIENTED_EDGE('',*,*,#9009,.T.);
#11778=ORIENTED_EDGE('',*,*,#9008,.F.);
#11779=ORIENTED_EDGE('',*,*,#9010,.T.);
#11780=ORIENTED_EDGE('',*,*,#9011,.T.);
#11781=ORIENTED_EDGE('',*,*,#9012,.T.);
#11782=ORIENTED_EDGE('',*,*,#9013,.T.);
#11783=ORIENTED_EDGE('',*,*,#9011,.F.);
#11784=ORIENTED_EDGE('',*,*,#9012,.F.);
#11785=ORIENTED_EDGE('',*,*,#9013,.F.);
#11786=ORIENTED_EDGE('',*,*,#9014,.T.);
#11787=ORIENTED_EDGE('',*,*,#9015,.T.);
#11788=ORIENTED_EDGE('',*,*,#9014,.F.);
#11789=ORIENTED_EDGE('',*,*,#9010,.F.);
#11790=ORIENTED_EDGE('',*,*,#9016,.T.);
#11791=ORIENTED_EDGE('',*,*,#9017,.T.);
#11792=ORIENTED_EDGE('',*,*,#9018,.T.);
#11793=ORIENTED_EDGE('',*,*,#8935,.F.);
#11794=ORIENTED_EDGE('',*,*,#9019,.T.);
#11795=ORIENTED_EDGE('',*,*,#9020,.T.);
#11796=ORIENTED_EDGE('',*,*,#9021,.F.);
#11797=ORIENTED_EDGE('',*,*,#9022,.T.);
#11798=ORIENTED_EDGE('',*,*,#9023,.F.);
#11799=ORIENTED_EDGE('',*,*,#9020,.F.);
#11800=ORIENTED_EDGE('',*,*,#9024,.F.);
#11801=ORIENTED_EDGE('',*,*,#9025,.T.);
#11802=ORIENTED_EDGE('',*,*,#9019,.F.);
#11803=ORIENTED_EDGE('',*,*,#9025,.F.);
#11804=ORIENTED_EDGE('',*,*,#9024,.T.);
#11805=ORIENTED_EDGE('',*,*,#9026,.T.);
#11806=ORIENTED_EDGE('',*,*,#9027,.T.);
#11807=ORIENTED_EDGE('',*,*,#9026,.F.);
#11808=ORIENTED_EDGE('',*,*,#9027,.F.);
#11809=ORIENTED_EDGE('',*,*,#9028,.F.);
#11810=ORIENTED_EDGE('',*,*,#8970,.T.);
#11811=ORIENTED_EDGE('',*,*,#9029,.T.);
#11812=ORIENTED_EDGE('',*,*,#9030,.F.);
#11813=ORIENTED_EDGE('',*,*,#9031,.T.);
#11814=ORIENTED_EDGE('',*,*,#9031,.F.);
#11815=ORIENTED_EDGE('',*,*,#9032,.F.);
#11816=ORIENTED_EDGE('',*,*,#8967,.F.);
#11817=ORIENTED_EDGE('',*,*,#8963,.F.);
#11818=ORIENTED_EDGE('',*,*,#8960,.F.);
#11819=ORIENTED_EDGE('',*,*,#8957,.F.);
#11820=ORIENTED_EDGE('',*,*,#8954,.F.);
#11821=ORIENTED_EDGE('',*,*,#8951,.F.);
#11822=ORIENTED_EDGE('',*,*,#8948,.F.);
#11823=ORIENTED_EDGE('',*,*,#8945,.F.);
#11824=ORIENTED_EDGE('',*,*,#8942,.F.);
#11825=ORIENTED_EDGE('',*,*,#8939,.F.);
#11826=ORIENTED_EDGE('',*,*,#8936,.F.);
#11827=ORIENTED_EDGE('',*,*,#9018,.F.);
#11828=ORIENTED_EDGE('',*,*,#9033,.T.);
#11829=ORIENTED_EDGE('',*,*,#8998,.T.);
#11830=ORIENTED_EDGE('',*,*,#8995,.T.);
#11831=ORIENTED_EDGE('',*,*,#8992,.T.);
#11832=ORIENTED_EDGE('',*,*,#8989,.T.);
#11833=ORIENTED_EDGE('',*,*,#8986,.T.);
#11834=ORIENTED_EDGE('',*,*,#8983,.T.);
#11835=ORIENTED_EDGE('',*,*,#8980,.T.);
#11836=ORIENTED_EDGE('',*,*,#8977,.T.);
#11837=ORIENTED_EDGE('',*,*,#8974,.T.);
#11838=ORIENTED_EDGE('',*,*,#8971,.T.);
#11839=ORIENTED_EDGE('',*,*,#8996,.T.);
#11840=ORIENTED_EDGE('',*,*,#9033,.F.);
#11841=ORIENTED_EDGE('',*,*,#9017,.F.);
#11842=ORIENTED_EDGE('',*,*,#9034,.T.);
#11843=ORIENTED_EDGE('',*,*,#9029,.F.);
#11844=ORIENTED_EDGE('',*,*,#8969,.F.);
#11845=ORIENTED_EDGE('',*,*,#8973,.F.);
#11846=ORIENTED_EDGE('',*,*,#8976,.F.);
#11847=ORIENTED_EDGE('',*,*,#8979,.F.);
#11848=ORIENTED_EDGE('',*,*,#8982,.F.);
#11849=ORIENTED_EDGE('',*,*,#8985,.F.);
#11850=ORIENTED_EDGE('',*,*,#8988,.F.);
#11851=ORIENTED_EDGE('',*,*,#8991,.F.);
#11852=ORIENTED_EDGE('',*,*,#8994,.F.);
#11853=ORIENTED_EDGE('',*,*,#8997,.F.);
#11854=ORIENTED_EDGE('',*,*,#9034,.F.);
#11855=ORIENTED_EDGE('',*,*,#9016,.F.);
#11856=ORIENTED_EDGE('',*,*,#8934,.F.);
#11857=ORIENTED_EDGE('',*,*,#8938,.F.);
#11858=ORIENTED_EDGE('',*,*,#8941,.F.);
#11859=ORIENTED_EDGE('',*,*,#8944,.F.);
#11860=ORIENTED_EDGE('',*,*,#8947,.F.);
#11861=ORIENTED_EDGE('',*,*,#8950,.F.);
#11862=ORIENTED_EDGE('',*,*,#8953,.F.);
#11863=ORIENTED_EDGE('',*,*,#8956,.F.);
#11864=ORIENTED_EDGE('',*,*,#8959,.F.);
#11865=ORIENTED_EDGE('',*,*,#8962,.F.);
#11866=ORIENTED_EDGE('',*,*,#8966,.F.);
#11867=ORIENTED_EDGE('',*,*,#8964,.T.);
#11868=ORIENTED_EDGE('',*,*,#9032,.T.);
#11869=ORIENTED_EDGE('',*,*,#9035,.F.);
#11870=ORIENTED_EDGE('',*,*,#9036,.F.);
#11871=ORIENTED_EDGE('',*,*,#9037,.F.);
#11872=ORIENTED_EDGE('',*,*,#8886,.F.);
#11873=ORIENTED_EDGE('',*,*,#8883,.F.);
#11874=ORIENTED_EDGE('',*,*,#8880,.F.);
#11875=ORIENTED_EDGE('',*,*,#8877,.F.);
#11876=ORIENTED_EDGE('',*,*,#8874,.F.);
#11877=ORIENTED_EDGE('',*,*,#8871,.F.);
#11878=ORIENTED_EDGE('',*,*,#8868,.F.);
#11879=ORIENTED_EDGE('',*,*,#8865,.F.);
#11880=ORIENTED_EDGE('',*,*,#8862,.F.);
#11881=ORIENTED_EDGE('',*,*,#8859,.F.);
#11882=ORIENTED_EDGE('',*,*,#8856,.F.);
#11883=ORIENTED_EDGE('',*,*,#8853,.F.);
#11884=ORIENTED_EDGE('',*,*,#8850,.F.);
#11885=ORIENTED_EDGE('',*,*,#8847,.F.);
#11886=ORIENTED_EDGE('',*,*,#8844,.F.);
#11887=ORIENTED_EDGE('',*,*,#8841,.F.);
#11888=ORIENTED_EDGE('',*,*,#9038,.F.);
#11889=ORIENTED_EDGE('',*,*,#9039,.T.);
#11890=ORIENTED_EDGE('',*,*,#8932,.T.);
#11891=ORIENTED_EDGE('',*,*,#8929,.T.);
#11892=ORIENTED_EDGE('',*,*,#8926,.T.);
#11893=ORIENTED_EDGE('',*,*,#8923,.T.);
#11894=ORIENTED_EDGE('',*,*,#8920,.T.);
#11895=ORIENTED_EDGE('',*,*,#8917,.T.);
#11896=ORIENTED_EDGE('',*,*,#8914,.T.);
#11897=ORIENTED_EDGE('',*,*,#8911,.T.);
#11898=ORIENTED_EDGE('',*,*,#8908,.T.);
#11899=ORIENTED_EDGE('',*,*,#8905,.T.);
#11900=ORIENTED_EDGE('',*,*,#8902,.T.);
#11901=ORIENTED_EDGE('',*,*,#8899,.T.);
#11902=ORIENTED_EDGE('',*,*,#8896,.T.);
#11903=ORIENTED_EDGE('',*,*,#8893,.T.);
#11904=ORIENTED_EDGE('',*,*,#8890,.T.);
#11905=ORIENTED_EDGE('',*,*,#9040,.T.);
#11906=ORIENTED_EDGE('',*,*,#9041,.T.);
#11907=ORIENTED_EDGE('',*,*,#9042,.T.);
#11908=ORIENTED_EDGE('',*,*,#9043,.T.);
#11909=ORIENTED_EDGE('',*,*,#9038,.T.);
#11910=ORIENTED_EDGE('',*,*,#8930,.T.);
#11911=ORIENTED_EDGE('',*,*,#9039,.F.);
#11912=ORIENTED_EDGE('',*,*,#9043,.F.);
#11913=ORIENTED_EDGE('',*,*,#9044,.T.);
#11914=ORIENTED_EDGE('',*,*,#9045,.F.);
#11915=ORIENTED_EDGE('',*,*,#8888,.F.);
#11916=ORIENTED_EDGE('',*,*,#8892,.F.);
#11917=ORIENTED_EDGE('',*,*,#8895,.F.);
#11918=ORIENTED_EDGE('',*,*,#8898,.F.);
#11919=ORIENTED_EDGE('',*,*,#8901,.F.);
#11920=ORIENTED_EDGE('',*,*,#8904,.F.);
#11921=ORIENTED_EDGE('',*,*,#8907,.F.);
#11922=ORIENTED_EDGE('',*,*,#8910,.F.);
#11923=ORIENTED_EDGE('',*,*,#8913,.F.);
#11924=ORIENTED_EDGE('',*,*,#8916,.F.);
#11925=ORIENTED_EDGE('',*,*,#8919,.F.);
#11926=ORIENTED_EDGE('',*,*,#8922,.F.);
#11927=ORIENTED_EDGE('',*,*,#8925,.F.);
#11928=ORIENTED_EDGE('',*,*,#8928,.F.);
#11929=ORIENTED_EDGE('',*,*,#8931,.F.);
#11930=ORIENTED_EDGE('',*,*,#9044,.F.);
#11931=ORIENTED_EDGE('',*,*,#9042,.F.);
#11932=ORIENTED_EDGE('',*,*,#8839,.F.);
#11933=ORIENTED_EDGE('',*,*,#8843,.F.);
#11934=ORIENTED_EDGE('',*,*,#8846,.F.);
#11935=ORIENTED_EDGE('',*,*,#8849,.F.);
#11936=ORIENTED_EDGE('',*,*,#8852,.F.);
#11937=ORIENTED_EDGE('',*,*,#8855,.F.);
#11938=ORIENTED_EDGE('',*,*,#8858,.F.);
#11939=ORIENTED_EDGE('',*,*,#8861,.F.);
#11940=ORIENTED_EDGE('',*,*,#8864,.F.);
#11941=ORIENTED_EDGE('',*,*,#8867,.F.);
#11942=ORIENTED_EDGE('',*,*,#8870,.F.);
#11943=ORIENTED_EDGE('',*,*,#8873,.F.);
#11944=ORIENTED_EDGE('',*,*,#8876,.F.);
#11945=ORIENTED_EDGE('',*,*,#8879,.F.);
#11946=ORIENTED_EDGE('',*,*,#8882,.F.);
#11947=ORIENTED_EDGE('',*,*,#8885,.F.);
#11948=ORIENTED_EDGE('',*,*,#9046,.F.);
#11949=ORIENTED_EDGE('',*,*,#9047,.T.);
#11950=ORIENTED_EDGE('',*,*,#9048,.T.);
#11951=ORIENTED_EDGE('',*,*,#9049,.T.);
#11952=ORIENTED_EDGE('',*,*,#9050,.T.);
#11953=ORIENTED_EDGE('',*,*,#9047,.F.);
#11954=ORIENTED_EDGE('',*,*,#9051,.F.);
#11955=ORIENTED_EDGE('',*,*,#9052,.F.);
#11956=ORIENTED_EDGE('',*,*,#9053,.T.);
#11957=ORIENTED_EDGE('',*,*,#9054,.F.);
#11958=ORIENTED_EDGE('',*,*,#9055,.T.);
#11959=ORIENTED_EDGE('',*,*,#9021,.T.);
#11960=ORIENTED_EDGE('',*,*,#9023,.T.);
#11961=ORIENTED_EDGE('',*,*,#9056,.T.);
#11962=ORIENTED_EDGE('',*,*,#9057,.F.);
#11963=ORIENTED_EDGE('',*,*,#9058,.F.);
#11964=ORIENTED_EDGE('',*,*,#9050,.F.);
#11965=ORIENTED_EDGE('',*,*,#9059,.F.);
#11966=ORIENTED_EDGE('',*,*,#9060,.F.);
#11967=ORIENTED_EDGE('',*,*,#9051,.T.);
#11968=ORIENTED_EDGE('',*,*,#9052,.T.);
#11969=ORIENTED_EDGE('',*,*,#9060,.T.);
#11970=ORIENTED_EDGE('',*,*,#9061,.T.);
#11971=ORIENTED_EDGE('',*,*,#9062,.T.);
#11972=ORIENTED_EDGE('',*,*,#9063,.F.);
#11973=ORIENTED_EDGE('',*,*,#9064,.T.);
#11974=ORIENTED_EDGE('',*,*,#9057,.T.);
#11975=ORIENTED_EDGE('',*,*,#9065,.T.);
#11976=ORIENTED_EDGE('',*,*,#9054,.T.);
#11977=ORIENTED_EDGE('',*,*,#9066,.T.);
#11978=ORIENTED_EDGE('',*,*,#9067,.T.);
#11979=ORIENTED_EDGE('',*,*,#9068,.T.);
#11980=ORIENTED_EDGE('',*,*,#9069,.T.);
#11981=ORIENTED_EDGE('',*,*,#9070,.T.);
#11982=ORIENTED_EDGE('',*,*,#9071,.T.);
#11983=ORIENTED_EDGE('',*,*,#9070,.F.);
#11984=ORIENTED_EDGE('',*,*,#9072,.F.);
#11985=ORIENTED_EDGE('',*,*,#9069,.F.);
#11986=ORIENTED_EDGE('',*,*,#9071,.F.);
#11987=ORIENTED_EDGE('',*,*,#9073,.T.);
#11988=ORIENTED_EDGE('',*,*,#9074,.T.);
#11989=ORIENTED_EDGE('',*,*,#9073,.F.);
#11990=ORIENTED_EDGE('',*,*,#9028,.T.);
#11991=ORIENTED_EDGE('',*,*,#9075,.T.);
#11992=ORIENTED_EDGE('',*,*,#9076,.T.);
#11993=ORIENTED_EDGE('',*,*,#9075,.F.);
#11994=ORIENTED_EDGE('',*,*,#9076,.F.);
#11995=ORIENTED_EDGE('',*,*,#9077,.T.);
#11996=ORIENTED_EDGE('',*,*,#9078,.T.);
#11997=ORIENTED_EDGE('',*,*,#9077,.F.);
#11998=ORIENTED_EDGE('',*,*,#9072,.T.);
#11999=ORIENTED_EDGE('',*,*,#9079,.T.);
#12000=ORIENTED_EDGE('',*,*,#9080,.T.);
#12001=ORIENTED_EDGE('',*,*,#9079,.F.);
#12002=ORIENTED_EDGE('',*,*,#9080,.F.);
#12003=ORIENTED_EDGE('',*,*,#9081,.T.);
#12004=ORIENTED_EDGE('',*,*,#9082,.F.);
#12005=ORIENTED_EDGE('',*,*,#9083,.F.);
#12006=ORIENTED_EDGE('',*,*,#9081,.F.);
#12007=ORIENTED_EDGE('',*,*,#9022,.F.);
#12008=ORIENTED_EDGE('',*,*,#9055,.F.);
#12009=ORIENTED_EDGE('',*,*,#9068,.F.);
#12010=ORIENTED_EDGE('',*,*,#9084,.F.);
#12011=ORIENTED_EDGE('',*,*,#9065,.F.);
#12012=ORIENTED_EDGE('',*,*,#9056,.F.);
#12013=ORIENTED_EDGE('',*,*,#9074,.F.);
#12014=ORIENTED_EDGE('',*,*,#9078,.F.);
#12015=ORIENTED_EDGE('',*,*,#9085,.F.);
#12016=ORIENTED_EDGE('',*,*,#9086,.T.);
#12017=ORIENTED_EDGE('',*,*,#9087,.F.);
#12018=ORIENTED_EDGE('',*,*,#9086,.F.);
#12019=ORIENTED_EDGE('',*,*,#9015,.F.);
#12020=ORIENTED_EDGE('',*,*,#9082,.T.);
#12021=ORIENTED_EDGE('',*,*,#9088,.T.);
#12022=ORIENTED_EDGE('',*,*,#9089,.T.);
#12023=ORIENTED_EDGE('',*,*,#9088,.F.);
#12024=ORIENTED_EDGE('',*,*,#9083,.T.);
#12025=ORIENTED_EDGE('',*,*,#9084,.T.);
#12026=ORIENTED_EDGE('',*,*,#9067,.F.);
#12027=ORIENTED_EDGE('',*,*,#9090,.T.);
#12028=ORIENTED_EDGE('',*,*,#9061,.F.);
#12029=ORIENTED_EDGE('',*,*,#9059,.T.);
#12030=ORIENTED_EDGE('',*,*,#9049,.F.);
#12031=ORIENTED_EDGE('',*,*,#9091,.T.);
#12032=ORIENTED_EDGE('',*,*,#9063,.T.);
#12033=ORIENTED_EDGE('',*,*,#9062,.F.);
#12034=ORIENTED_EDGE('',*,*,#9090,.F.);
#12035=ORIENTED_EDGE('',*,*,#9066,.F.);
#12036=ORIENTED_EDGE('',*,*,#9053,.F.);
#12037=ORIENTED_EDGE('',*,*,#9085,.T.);
#12038=ORIENTED_EDGE('',*,*,#9048,.F.);
#12039=ORIENTED_EDGE('',*,*,#9058,.T.);
#12040=ORIENTED_EDGE('',*,*,#9064,.F.);
#12041=ORIENTED_EDGE('',*,*,#9091,.F.);
#12042=ORIENTED_EDGE('',*,*,#9087,.T.);
#12043=ORIENTED_EDGE('',*,*,#9006,.T.);
#12044=ORIENTED_EDGE('',*,*,#9092,.T.);
#12045=ORIENTED_EDGE('',*,*,#9093,.F.);
#12046=ORIENTED_EDGE('',*,*,#9092,.F.);
#12047=ORIENTED_EDGE('',*,*,#9094,.F.);
#12048=ORIENTED_EDGE('',*,*,#9093,.T.);
#12049=ORIENTED_EDGE('',*,*,#9040,.F.);
#12050=ORIENTED_EDGE('',*,*,#8840,.F.);
#12051=ORIENTED_EDGE('',*,*,#9041,.F.);
#12052=ORIENTED_EDGE('',*,*,#9095,.T.);
#12053=ORIENTED_EDGE('',*,*,#9094,.T.);
#12054=ORIENTED_EDGE('',*,*,#9095,.F.);
#12055=ORIENTED_EDGE('',*,*,#8884,.T.);
#12056=ORIENTED_EDGE('',*,*,#9037,.T.);
#12057=ORIENTED_EDGE('',*,*,#9096,.F.);
#12058=ORIENTED_EDGE('',*,*,#9046,.T.);
#12059=ORIENTED_EDGE('',*,*,#9097,.F.);
#12060=ORIENTED_EDGE('',*,*,#9096,.T.);
#12061=ORIENTED_EDGE('',*,*,#9036,.T.);
#12062=ORIENTED_EDGE('',*,*,#8889,.T.);
#12063=ORIENTED_EDGE('',*,*,#9045,.T.);
#12064=ORIENTED_EDGE('',*,*,#9089,.F.);
#12065=ORIENTED_EDGE('',*,*,#9098,.T.);
#12066=ORIENTED_EDGE('',*,*,#9097,.T.);
#12067=ORIENTED_EDGE('',*,*,#9098,.F.);
#12068=ORIENTED_EDGE('',*,*,#9009,.F.);
#12069=ORIENTED_EDGE('',*,*,#9099,.T.);
#12070=ORIENTED_EDGE('',*,*,#9035,.T.);
#12071=ORIENTED_EDGE('',*,*,#9030,.T.);
#12072=ORIENTED_EDGE('',*,*,#8965,.T.);
#12073=ORIENTED_EDGE('',*,*,#9099,.F.);
#12074=ORIENTED_EDGE('',*,*,#9100,.F.);
#12075=ORIENTED_EDGE('',*,*,#9101,.T.);
#12076=ORIENTED_EDGE('',*,*,#9102,.T.);
#12077=ORIENTED_EDGE('',*,*,#9101,.F.);
#12078=ORIENTED_EDGE('',*,*,#9102,.F.);
#12079=ORIENTED_EDGE('',*,*,#9103,.F.);
#12080=ORIENTED_EDGE('',*,*,#9100,.T.);
#12081=ORIENTED_EDGE('',*,*,#9104,.F.);
#12082=ORIENTED_EDGE('',*,*,#9105,.T.);
#12083=ORIENTED_EDGE('',*,*,#9103,.T.);
#12084=ORIENTED_EDGE('',*,*,#9105,.F.);
#12085=ORIENTED_EDGE('',*,*,#9106,.F.);
#12086=ORIENTED_EDGE('',*,*,#9107,.T.);
#12087=ORIENTED_EDGE('',*,*,#9104,.T.);
#12088=ORIENTED_EDGE('',*,*,#9107,.F.);
#12089=ORIENTED_EDGE('',*,*,#9108,.F.);
#12090=ORIENTED_EDGE('',*,*,#9106,.T.);
#12091=ORIENTED_EDGE('',*,*,#9109,.F.);
#12092=ORIENTED_EDGE('',*,*,#9110,.T.);
#12093=ORIENTED_EDGE('',*,*,#9108,.T.);
#12094=ORIENTED_EDGE('',*,*,#9110,.F.);
#12095=ORIENTED_EDGE('',*,*,#9111,.F.);
#12096=ORIENTED_EDGE('',*,*,#9112,.T.);
#12097=ORIENTED_EDGE('',*,*,#9109,.T.);
#12098=ORIENTED_EDGE('',*,*,#9112,.F.);
#12099=ORIENTED_EDGE('',*,*,#9111,.T.);
#12100=ORIENTED_EDGE('',*,*,#9113,.F.);
#12101=ORIENTED_EDGE('',*,*,#9114,.F.);
#12102=ORIENTED_EDGE('',*,*,#9115,.T.);
#12103=ORIENTED_EDGE('',*,*,#9113,.T.);
#12104=ORIENTED_EDGE('',*,*,#9115,.F.);
#12105=ORIENTED_EDGE('',*,*,#9116,.F.);
#12106=ORIENTED_EDGE('',*,*,#9114,.T.);
#12107=ORIENTED_EDGE('',*,*,#9117,.F.);
#12108=ORIENTED_EDGE('',*,*,#9118,.T.);
#12109=ORIENTED_EDGE('',*,*,#9116,.T.);
#12110=ORIENTED_EDGE('',*,*,#9118,.F.);
#12111=ORIENTED_EDGE('',*,*,#9117,.T.);
#12112=ORIENTED_EDGE('',*,*,#9119,.F.);
#12113=ORIENTED_EDGE('',*,*,#9120,.F.);
#12114=ORIENTED_EDGE('',*,*,#9121,.T.);
#12115=ORIENTED_EDGE('',*,*,#9119,.T.);
#12116=ORIENTED_EDGE('',*,*,#9121,.F.);
#12117=ORIENTED_EDGE('',*,*,#9122,.F.);
#12118=ORIENTED_EDGE('',*,*,#9120,.T.);
#12119=ORIENTED_EDGE('',*,*,#9123,.F.);
#12120=ORIENTED_EDGE('',*,*,#9124,.T.);
#12121=ORIENTED_EDGE('',*,*,#9122,.T.);
#12122=ORIENTED_EDGE('',*,*,#9124,.F.);
#12123=ORIENTED_EDGE('',*,*,#9125,.F.);
#12124=ORIENTED_EDGE('',*,*,#9126,.T.);
#12125=ORIENTED_EDGE('',*,*,#9123,.T.);
#12126=ORIENTED_EDGE('',*,*,#9126,.F.);
#12127=ORIENTED_EDGE('',*,*,#9125,.T.);
#12128=ORIENTED_EDGE('',*,*,#9127,.T.);
#12129=ORIENTED_EDGE('',*,*,#9128,.T.);
#12130=ORIENTED_EDGE('',*,*,#9129,.F.);
#12131=ORIENTED_EDGE('',*,*,#9128,.F.);
#12132=ORIENTED_EDGE('',*,*,#9129,.T.);
#12133=ORIENTED_EDGE('',*,*,#9127,.F.);
#12134=ORIENTED_EDGE('',*,*,#9130,.F.);
#12135=ORIENTED_EDGE('',*,*,#9131,.T.);
#12136=ORIENTED_EDGE('',*,*,#9130,.T.);
#12137=ORIENTED_EDGE('',*,*,#9131,.F.);
#12138=ORIENTED_EDGE('',*,*,#9132,.T.);
#12139=ORIENTED_EDGE('',*,*,#9133,.T.);
#12140=ORIENTED_EDGE('',*,*,#9134,.F.);
#12141=ORIENTED_EDGE('',*,*,#9133,.F.);
#12142=ORIENTED_EDGE('',*,*,#9135,.F.);
#12143=ORIENTED_EDGE('',*,*,#9134,.T.);
#12144=ORIENTED_EDGE('',*,*,#9136,.F.);
#12145=ORIENTED_EDGE('',*,*,#9137,.T.);
#12146=ORIENTED_EDGE('',*,*,#9135,.T.);
#12147=ORIENTED_EDGE('',*,*,#9137,.F.);
#12148=ORIENTED_EDGE('',*,*,#9136,.T.);
#12149=ORIENTED_EDGE('',*,*,#9132,.F.);
#12150=ORIENTED_EDGE('',*,*,#9138,.F.);
#12151=ORIENTED_EDGE('',*,*,#9139,.F.);
#12152=ORIENTED_EDGE('',*,*,#9140,.T.);
#12153=ORIENTED_EDGE('',*,*,#9138,.T.);
#12154=ORIENTED_EDGE('',*,*,#9140,.F.);
#12155=ORIENTED_EDGE('',*,*,#9141,.F.);
#12156=ORIENTED_EDGE('',*,*,#9142,.T.);
#12157=ORIENTED_EDGE('',*,*,#9139,.T.);
#12158=ORIENTED_EDGE('',*,*,#9142,.F.);
#12159=ORIENTED_EDGE('',*,*,#9143,.F.);
#12160=ORIENTED_EDGE('',*,*,#9144,.T.);
#12161=ORIENTED_EDGE('',*,*,#9141,.T.);
#12162=ORIENTED_EDGE('',*,*,#9144,.F.);
#12163=ORIENTED_EDGE('',*,*,#9143,.T.);
#12164=ORIENTED_EDGE('',*,*,#9145,.T.);
#12165=ORIENTED_EDGE('',*,*,#9146,.T.);
#12166=ORIENTED_EDGE('',*,*,#9147,.T.);
#12167=ORIENTED_EDGE('',*,*,#9148,.T.);
#12168=ORIENTED_EDGE('',*,*,#9145,.F.);
#12169=ORIENTED_EDGE('',*,*,#9149,.T.);
#12170=ORIENTED_EDGE('',*,*,#9150,.F.);
#12171=ORIENTED_EDGE('',*,*,#9151,.T.);
#12172=ORIENTED_EDGE('',*,*,#9152,.T.);
#12173=ORIENTED_EDGE('',*,*,#9153,.T.);
#12174=ORIENTED_EDGE('',*,*,#9148,.F.);
#12175=ORIENTED_EDGE('',*,*,#9154,.F.);
#12176=ORIENTED_EDGE('',*,*,#9155,.F.);
#12177=ORIENTED_EDGE('',*,*,#9149,.F.);
#12178=ORIENTED_EDGE('',*,*,#9156,.T.);
#12179=ORIENTED_EDGE('',*,*,#9157,.T.);
#12180=ORIENTED_EDGE('',*,*,#9158,.T.);
#12181=ORIENTED_EDGE('',*,*,#9159,.T.);
#12182=ORIENTED_EDGE('',*,*,#9159,.F.);
#12183=ORIENTED_EDGE('',*,*,#9160,.F.);
#12184=ORIENTED_EDGE('',*,*,#9161,.F.);
#12185=ORIENTED_EDGE('',*,*,#9162,.F.);
#12186=ORIENTED_EDGE('',*,*,#9158,.F.);
#12187=ORIENTED_EDGE('',*,*,#9163,.T.);
#12188=ORIENTED_EDGE('',*,*,#9164,.T.);
#12189=ORIENTED_EDGE('',*,*,#9165,.T.);
#12190=ORIENTED_EDGE('',*,*,#9166,.F.);
#12191=ORIENTED_EDGE('',*,*,#9160,.T.);
#12192=ORIENTED_EDGE('',*,*,#9167,.T.);
#12193=ORIENTED_EDGE('',*,*,#9168,.T.);
#12194=ORIENTED_EDGE('',*,*,#9169,.T.);
#12195=ORIENTED_EDGE('',*,*,#9170,.T.);
#12196=ORIENTED_EDGE('',*,*,#9171,.T.);
#12197=ORIENTED_EDGE('',*,*,#9172,.T.);
#12198=ORIENTED_EDGE('',*,*,#9168,.F.);
#12199=ORIENTED_EDGE('',*,*,#9173,.F.);
#12200=ORIENTED_EDGE('',*,*,#9174,.F.);
#12201=ORIENTED_EDGE('',*,*,#9175,.F.);
#12202=ORIENTED_EDGE('',*,*,#9167,.F.);
#12203=ORIENTED_EDGE('',*,*,#9176,.F.);
#12204=ORIENTED_EDGE('',*,*,#9177,.T.);
#12205=ORIENTED_EDGE('',*,*,#9178,.T.);
#12206=ORIENTED_EDGE('',*,*,#9179,.F.);
#12207=ORIENTED_EDGE('',*,*,#9173,.T.);
#12208=ORIENTED_EDGE('',*,*,#9172,.F.);
#12209=ORIENTED_EDGE('',*,*,#9180,.T.);
#12210=ORIENTED_EDGE('',*,*,#9181,.F.);
#12211=ORIENTED_EDGE('',*,*,#9182,.T.);
#12212=ORIENTED_EDGE('',*,*,#9176,.T.);
#12213=ORIENTED_EDGE('',*,*,#9183,.T.);
#12214=ORIENTED_EDGE('',*,*,#9184,.T.);
#12215=ORIENTED_EDGE('',*,*,#9185,.T.);
#12216=ORIENTED_EDGE('',*,*,#9186,.T.);
#12217=ORIENTED_EDGE('',*,*,#9187,.T.);
#12218=ORIENTED_EDGE('',*,*,#9188,.T.);
#12219=ORIENTED_EDGE('',*,*,#9187,.F.);
#12220=ORIENTED_EDGE('',*,*,#9189,.T.);
#12221=ORIENTED_EDGE('',*,*,#9190,.T.);
#12222=ORIENTED_EDGE('',*,*,#9170,.F.);
#12223=ORIENTED_EDGE('',*,*,#9191,.T.);
#12224=ORIENTED_EDGE('',*,*,#9192,.T.);
#12225=ORIENTED_EDGE('',*,*,#9190,.F.);
#12226=ORIENTED_EDGE('',*,*,#9193,.T.);
#12227=ORIENTED_EDGE('',*,*,#9184,.F.);
#12228=ORIENTED_EDGE('',*,*,#9194,.T.);
#12229=ORIENTED_EDGE('',*,*,#9195,.T.);
#12230=ORIENTED_EDGE('',*,*,#9196,.F.);
#12231=ORIENTED_EDGE('',*,*,#9197,.T.);
#12232=ORIENTED_EDGE('',*,*,#9198,.F.);
#12233=ORIENTED_EDGE('',*,*,#9183,.F.);
#12234=ORIENTED_EDGE('',*,*,#9188,.F.);
#12235=ORIENTED_EDGE('',*,*,#9192,.F.);
#12236=ORIENTED_EDGE('',*,*,#9199,.F.);
#12237=ORIENTED_EDGE('',*,*,#9200,.F.);
#12238=ORIENTED_EDGE('',*,*,#9201,.F.);
#12239=ORIENTED_EDGE('',*,*,#9202,.F.);
#12240=ORIENTED_EDGE('',*,*,#9194,.F.);
#12241=ORIENTED_EDGE('',*,*,#9169,.F.);
#12242=ORIENTED_EDGE('',*,*,#9175,.T.);
#12243=ORIENTED_EDGE('',*,*,#9203,.F.);
#12244=ORIENTED_EDGE('',*,*,#9204,.T.);
#12245=ORIENTED_EDGE('',*,*,#9199,.T.);
#12246=ORIENTED_EDGE('',*,*,#9191,.F.);
#12247=ORIENTED_EDGE('',*,*,#9205,.T.);
#12248=ORIENTED_EDGE('',*,*,#9206,.T.);
#12249=ORIENTED_EDGE('',*,*,#9207,.T.);
#12250=ORIENTED_EDGE('',*,*,#9208,.T.);
#12251=ORIENTED_EDGE('',*,*,#9205,.F.);
#12252=ORIENTED_EDGE('',*,*,#9209,.T.);
#12253=ORIENTED_EDGE('',*,*,#9210,.F.);
#12254=ORIENTED_EDGE('',*,*,#9211,.T.);
#12255=ORIENTED_EDGE('',*,*,#9212,.T.);
#12256=ORIENTED_EDGE('',*,*,#9213,.T.);
#12257=ORIENTED_EDGE('',*,*,#9208,.F.);
#12258=ORIENTED_EDGE('',*,*,#9214,.F.);
#12259=ORIENTED_EDGE('',*,*,#9215,.F.);
#12260=ORIENTED_EDGE('',*,*,#9209,.F.);
#12261=ORIENTED_EDGE('',*,*,#9216,.T.);
#12262=ORIENTED_EDGE('',*,*,#9217,.T.);
#12263=ORIENTED_EDGE('',*,*,#9150,.T.);
#12264=ORIENTED_EDGE('',*,*,#9155,.T.);
#12265=ORIENTED_EDGE('',*,*,#9179,.T.);
#12266=ORIENTED_EDGE('',*,*,#9218,.T.);
#12267=ORIENTED_EDGE('',*,*,#9203,.T.);
#12268=ORIENTED_EDGE('',*,*,#9174,.T.);
#12269=ORIENTED_EDGE('',*,*,#9218,.F.);
#12270=ORIENTED_EDGE('',*,*,#9178,.F.);
#12271=ORIENTED_EDGE('',*,*,#9211,.F.);
#12272=ORIENTED_EDGE('',*,*,#9219,.F.);
#12273=ORIENTED_EDGE('',*,*,#9220,.F.);
#12274=ORIENTED_EDGE('',*,*,#9204,.F.);
#12275=ORIENTED_EDGE('',*,*,#9221,.T.);
#12276=ORIENTED_EDGE('',*,*,#9219,.T.);
#12277=ORIENTED_EDGE('',*,*,#9210,.T.);
#12278=ORIENTED_EDGE('',*,*,#9215,.T.);
#12279=ORIENTED_EDGE('',*,*,#9222,.T.);
#12280=ORIENTED_EDGE('',*,*,#9223,.T.);
#12281=ORIENTED_EDGE('',*,*,#9224,.T.);
#12282=ORIENTED_EDGE('',*,*,#9225,.T.);
#12283=ORIENTED_EDGE('',*,*,#9226,.T.);
#12284=ORIENTED_EDGE('',*,*,#9227,.T.);
#12285=ORIENTED_EDGE('',*,*,#9181,.T.);
#12286=ORIENTED_EDGE('',*,*,#9228,.T.);
#12287=ORIENTED_EDGE('',*,*,#9226,.F.);
#12288=ORIENTED_EDGE('',*,*,#9182,.F.);
#12289=ORIENTED_EDGE('',*,*,#9227,.F.);
#12290=ORIENTED_EDGE('',*,*,#9225,.F.);
#12291=ORIENTED_EDGE('',*,*,#9229,.F.);
#12292=ORIENTED_EDGE('',*,*,#9164,.F.);
#12293=ORIENTED_EDGE('',*,*,#9152,.F.);
#12294=ORIENTED_EDGE('',*,*,#9212,.F.);
#12295=ORIENTED_EDGE('',*,*,#9177,.F.);
#12296=ORIENTED_EDGE('',*,*,#9230,.T.);
#12297=ORIENTED_EDGE('',*,*,#9231,.T.);
#12298=ORIENTED_EDGE('',*,*,#9232,.T.);
#12299=ORIENTED_EDGE('',*,*,#9233,.T.);
#12300=ORIENTED_EDGE('',*,*,#9234,.T.);
#12301=ORIENTED_EDGE('',*,*,#9235,.T.);
#12302=ORIENTED_EDGE('',*,*,#9236,.T.);
#12303=ORIENTED_EDGE('',*,*,#9237,.T.);
#12304=ORIENTED_EDGE('',*,*,#9238,.T.);
#12305=ORIENTED_EDGE('',*,*,#9239,.T.);
#12306=ORIENTED_EDGE('',*,*,#9240,.T.);
#12307=ORIENTED_EDGE('',*,*,#9241,.T.);
#12308=ORIENTED_EDGE('',*,*,#9242,.T.);
#12309=ORIENTED_EDGE('',*,*,#9243,.T.);
#12310=ORIENTED_EDGE('',*,*,#9244,.T.);
#12311=ORIENTED_EDGE('',*,*,#9245,.T.);
#12312=ORIENTED_EDGE('',*,*,#9246,.T.);
#12313=ORIENTED_EDGE('',*,*,#9247,.T.);
#12314=ORIENTED_EDGE('',*,*,#9248,.T.);
#12315=ORIENTED_EDGE('',*,*,#9249,.T.);
#12316=ORIENTED_EDGE('',*,*,#9250,.T.);
#12317=ORIENTED_EDGE('',*,*,#9251,.T.);
#12318=ORIENTED_EDGE('',*,*,#9252,.T.);
#12319=ORIENTED_EDGE('',*,*,#9253,.T.);
#12320=ORIENTED_EDGE('',*,*,#9254,.T.);
#12321=ORIENTED_EDGE('',*,*,#9255,.T.);
#12322=ORIENTED_EDGE('',*,*,#9256,.T.);
#12323=ORIENTED_EDGE('',*,*,#9257,.T.);
#12324=ORIENTED_EDGE('',*,*,#9258,.T.);
#12325=ORIENTED_EDGE('',*,*,#9259,.T.);
#12326=ORIENTED_EDGE('',*,*,#9260,.T.);
#12327=ORIENTED_EDGE('',*,*,#9261,.T.);
#12328=ORIENTED_EDGE('',*,*,#9262,.T.);
#12329=ORIENTED_EDGE('',*,*,#9263,.T.);
#12330=ORIENTED_EDGE('',*,*,#9264,.T.);
#12331=ORIENTED_EDGE('',*,*,#9265,.T.);
#12332=ORIENTED_EDGE('',*,*,#9266,.T.);
#12333=ORIENTED_EDGE('',*,*,#9267,.T.);
#12334=ORIENTED_EDGE('',*,*,#9268,.T.);
#12335=ORIENTED_EDGE('',*,*,#9269,.T.);
#12336=ORIENTED_EDGE('',*,*,#9270,.T.);
#12337=ORIENTED_EDGE('',*,*,#9271,.T.);
#12338=ORIENTED_EDGE('',*,*,#9272,.T.);
#12339=ORIENTED_EDGE('',*,*,#9273,.T.);
#12340=ORIENTED_EDGE('',*,*,#9274,.T.);
#12341=ORIENTED_EDGE('',*,*,#9275,.T.);
#12342=ORIENTED_EDGE('',*,*,#9276,.T.);
#12343=ORIENTED_EDGE('',*,*,#9277,.T.);
#12344=ORIENTED_EDGE('',*,*,#9278,.T.);
#12345=ORIENTED_EDGE('',*,*,#9279,.T.);
#12346=ORIENTED_EDGE('',*,*,#9280,.T.);
#12347=ORIENTED_EDGE('',*,*,#9281,.T.);
#12348=ORIENTED_EDGE('',*,*,#9282,.T.);
#12349=ORIENTED_EDGE('',*,*,#9283,.T.);
#12350=ORIENTED_EDGE('',*,*,#9284,.T.);
#12351=ORIENTED_EDGE('',*,*,#9285,.T.);
#12352=ORIENTED_EDGE('',*,*,#9286,.T.);
#12353=ORIENTED_EDGE('',*,*,#9287,.T.);
#12354=ORIENTED_EDGE('',*,*,#9288,.T.);
#12355=ORIENTED_EDGE('',*,*,#9289,.T.);
#12356=ORIENTED_EDGE('',*,*,#9290,.T.);
#12357=ORIENTED_EDGE('',*,*,#9291,.T.);
#12358=ORIENTED_EDGE('',*,*,#9292,.T.);
#12359=ORIENTED_EDGE('',*,*,#9293,.T.);
#12360=ORIENTED_EDGE('',*,*,#9294,.T.);
#12361=ORIENTED_EDGE('',*,*,#9295,.T.);
#12362=ORIENTED_EDGE('',*,*,#9296,.T.);
#12363=ORIENTED_EDGE('',*,*,#9297,.T.);
#12364=ORIENTED_EDGE('',*,*,#9298,.T.);
#12365=ORIENTED_EDGE('',*,*,#9299,.T.);
#12366=ORIENTED_EDGE('',*,*,#9300,.T.);
#12367=ORIENTED_EDGE('',*,*,#9301,.T.);
#12368=ORIENTED_EDGE('',*,*,#9302,.T.);
#12369=ORIENTED_EDGE('',*,*,#9303,.T.);
#12370=ORIENTED_EDGE('',*,*,#9304,.T.);
#12371=ORIENTED_EDGE('',*,*,#9305,.T.);
#12372=ORIENTED_EDGE('',*,*,#9306,.T.);
#12373=ORIENTED_EDGE('',*,*,#9224,.F.);
#12374=ORIENTED_EDGE('',*,*,#9307,.F.);
#12375=ORIENTED_EDGE('',*,*,#9308,.T.);
#12376=ORIENTED_EDGE('',*,*,#9309,.F.);
#12377=ORIENTED_EDGE('',*,*,#9310,.T.);
#12378=ORIENTED_EDGE('',*,*,#9229,.T.);
#12379=ORIENTED_EDGE('',*,*,#9185,.F.);
#12380=ORIENTED_EDGE('',*,*,#9198,.T.);
#12381=ORIENTED_EDGE('',*,*,#9311,.T.);
#12382=ORIENTED_EDGE('',*,*,#9307,.T.);
#12383=ORIENTED_EDGE('',*,*,#9223,.F.);
#12384=ORIENTED_EDGE('',*,*,#9312,.T.);
#12385=ORIENTED_EDGE('',*,*,#9311,.F.);
#12386=ORIENTED_EDGE('',*,*,#9197,.F.);
#12387=ORIENTED_EDGE('',*,*,#9313,.F.);
#12388=ORIENTED_EDGE('',*,*,#9308,.F.);
#12389=ORIENTED_EDGE('',*,*,#9166,.T.);
#12390=ORIENTED_EDGE('',*,*,#9314,.T.);
#12391=ORIENTED_EDGE('',*,*,#9315,.T.);
#12392=ORIENTED_EDGE('',*,*,#9161,.T.);
#12393=ORIENTED_EDGE('',*,*,#9156,.F.);
#12394=ORIENTED_EDGE('',*,*,#9162,.T.);
#12395=ORIENTED_EDGE('',*,*,#9315,.F.);
#12396=ORIENTED_EDGE('',*,*,#9316,.T.);
#12397=ORIENTED_EDGE('',*,*,#9202,.T.);
#12398=ORIENTED_EDGE('',*,*,#9317,.T.);
#12399=ORIENTED_EDGE('',*,*,#9314,.F.);
#12400=ORIENTED_EDGE('',*,*,#9165,.F.);
#12401=ORIENTED_EDGE('',*,*,#9310,.F.);
#12402=ORIENTED_EDGE('',*,*,#9318,.F.);
#12403=ORIENTED_EDGE('',*,*,#9195,.F.);
#12404=ORIENTED_EDGE('',*,*,#9316,.F.);
#12405=ORIENTED_EDGE('',*,*,#9196,.T.);
#12406=ORIENTED_EDGE('',*,*,#9318,.T.);
#12407=ORIENTED_EDGE('',*,*,#9309,.T.);
#12408=ORIENTED_EDGE('',*,*,#9313,.T.);
#12409=ORIENTED_EDGE('',*,*,#9230,.F.);
#12410=ORIENTED_EDGE('',*,*,#9319,.T.);
#12411=ORIENTED_EDGE('',*,*,#9320,.T.);
#12412=ORIENTED_EDGE('',*,*,#9321,.F.);
#12413=ORIENTED_EDGE('',*,*,#9248,.F.);
#12414=ORIENTED_EDGE('',*,*,#9322,.T.);
#12415=ORIENTED_EDGE('',*,*,#9323,.T.);
#12416=ORIENTED_EDGE('',*,*,#9319,.F.);
#12417=ORIENTED_EDGE('',*,*,#9247,.F.);
#12418=ORIENTED_EDGE('',*,*,#9324,.T.);
#12419=ORIENTED_EDGE('',*,*,#9325,.T.);
#12420=ORIENTED_EDGE('',*,*,#9322,.F.);
#12421=ORIENTED_EDGE('',*,*,#9246,.F.);
#12422=ORIENTED_EDGE('',*,*,#9326,.T.);
#12423=ORIENTED_EDGE('',*,*,#9327,.T.);
#12424=ORIENTED_EDGE('',*,*,#9324,.F.);
#12425=ORIENTED_EDGE('',*,*,#9245,.F.);
#12426=ORIENTED_EDGE('',*,*,#9328,.T.);
#12427=ORIENTED_EDGE('',*,*,#9329,.T.);
#12428=ORIENTED_EDGE('',*,*,#9326,.F.);
#12429=ORIENTED_EDGE('',*,*,#9244,.F.);
#12430=ORIENTED_EDGE('',*,*,#9330,.T.);
#12431=ORIENTED_EDGE('',*,*,#9331,.T.);
#12432=ORIENTED_EDGE('',*,*,#9328,.F.);
#12433=ORIENTED_EDGE('',*,*,#9243,.F.);
#12434=ORIENTED_EDGE('',*,*,#9332,.T.);
#12435=ORIENTED_EDGE('',*,*,#9333,.T.);
#12436=ORIENTED_EDGE('',*,*,#9330,.F.);
#12437=ORIENTED_EDGE('',*,*,#9242,.F.);
#12438=ORIENTED_EDGE('',*,*,#9334,.T.);
#12439=ORIENTED_EDGE('',*,*,#9335,.T.);
#12440=ORIENTED_EDGE('',*,*,#9332,.F.);
#12441=ORIENTED_EDGE('',*,*,#9241,.F.);
#12442=ORIENTED_EDGE('',*,*,#9336,.T.);
#12443=ORIENTED_EDGE('',*,*,#9337,.T.);
#12444=ORIENTED_EDGE('',*,*,#9334,.F.);
#12445=ORIENTED_EDGE('',*,*,#9240,.F.);
#12446=ORIENTED_EDGE('',*,*,#9338,.T.);
#12447=ORIENTED_EDGE('',*,*,#9339,.T.);
#12448=ORIENTED_EDGE('',*,*,#9336,.F.);
#12449=ORIENTED_EDGE('',*,*,#9239,.F.);
#12450=ORIENTED_EDGE('',*,*,#9340,.T.);
#12451=ORIENTED_EDGE('',*,*,#9341,.T.);
#12452=ORIENTED_EDGE('',*,*,#9338,.F.);
#12453=ORIENTED_EDGE('',*,*,#9238,.F.);
#12454=ORIENTED_EDGE('',*,*,#9342,.T.);
#12455=ORIENTED_EDGE('',*,*,#9343,.T.);
#12456=ORIENTED_EDGE('',*,*,#9340,.F.);
#12457=ORIENTED_EDGE('',*,*,#9237,.F.);
#12458=ORIENTED_EDGE('',*,*,#9344,.T.);
#12459=ORIENTED_EDGE('',*,*,#9345,.T.);
#12460=ORIENTED_EDGE('',*,*,#9342,.F.);
#12461=ORIENTED_EDGE('',*,*,#9236,.F.);
#12462=ORIENTED_EDGE('',*,*,#9346,.T.);
#12463=ORIENTED_EDGE('',*,*,#9347,.T.);
#12464=ORIENTED_EDGE('',*,*,#9344,.F.);
#12465=ORIENTED_EDGE('',*,*,#9235,.F.);
#12466=ORIENTED_EDGE('',*,*,#9348,.T.);
#12467=ORIENTED_EDGE('',*,*,#9349,.T.);
#12468=ORIENTED_EDGE('',*,*,#9346,.F.);
#12469=ORIENTED_EDGE('',*,*,#9234,.F.);
#12470=ORIENTED_EDGE('',*,*,#9350,.T.);
#12471=ORIENTED_EDGE('',*,*,#9351,.T.);
#12472=ORIENTED_EDGE('',*,*,#9348,.F.);
#12473=ORIENTED_EDGE('',*,*,#9233,.F.);
#12474=ORIENTED_EDGE('',*,*,#9352,.T.);
#12475=ORIENTED_EDGE('',*,*,#9353,.T.);
#12476=ORIENTED_EDGE('',*,*,#9350,.F.);
#12477=ORIENTED_EDGE('',*,*,#9232,.F.);
#12478=ORIENTED_EDGE('',*,*,#9354,.T.);
#12479=ORIENTED_EDGE('',*,*,#9355,.T.);
#12480=ORIENTED_EDGE('',*,*,#9352,.F.);
#12481=ORIENTED_EDGE('',*,*,#9231,.F.);
#12482=ORIENTED_EDGE('',*,*,#9321,.T.);
#12483=ORIENTED_EDGE('',*,*,#9356,.T.);
#12484=ORIENTED_EDGE('',*,*,#9354,.F.);
#12485=ORIENTED_EDGE('',*,*,#9356,.F.);
#12486=ORIENTED_EDGE('',*,*,#9320,.F.);
#12487=ORIENTED_EDGE('',*,*,#9323,.F.);
#12488=ORIENTED_EDGE('',*,*,#9325,.F.);
#12489=ORIENTED_EDGE('',*,*,#9327,.F.);
#12490=ORIENTED_EDGE('',*,*,#9329,.F.);
#12491=ORIENTED_EDGE('',*,*,#9331,.F.);
#12492=ORIENTED_EDGE('',*,*,#9333,.F.);
#12493=ORIENTED_EDGE('',*,*,#9335,.F.);
#12494=ORIENTED_EDGE('',*,*,#9337,.F.);
#12495=ORIENTED_EDGE('',*,*,#9339,.F.);
#12496=ORIENTED_EDGE('',*,*,#9341,.F.);
#12497=ORIENTED_EDGE('',*,*,#9343,.F.);
#12498=ORIENTED_EDGE('',*,*,#9345,.F.);
#12499=ORIENTED_EDGE('',*,*,#9347,.F.);
#12500=ORIENTED_EDGE('',*,*,#9349,.F.);
#12501=ORIENTED_EDGE('',*,*,#9351,.F.);
#12502=ORIENTED_EDGE('',*,*,#9353,.F.);
#12503=ORIENTED_EDGE('',*,*,#9355,.F.);
#12504=ORIENTED_EDGE('',*,*,#9249,.F.);
#12505=ORIENTED_EDGE('',*,*,#9357,.T.);
#12506=ORIENTED_EDGE('',*,*,#9358,.T.);
#12507=ORIENTED_EDGE('',*,*,#9359,.F.);
#12508=ORIENTED_EDGE('',*,*,#9256,.F.);
#12509=ORIENTED_EDGE('',*,*,#9360,.T.);
#12510=ORIENTED_EDGE('',*,*,#9361,.T.);
#12511=ORIENTED_EDGE('',*,*,#9357,.F.);
#12512=ORIENTED_EDGE('',*,*,#9255,.F.);
#12513=ORIENTED_EDGE('',*,*,#9362,.T.);
#12514=ORIENTED_EDGE('',*,*,#9363,.T.);
#12515=ORIENTED_EDGE('',*,*,#9360,.F.);
#12516=ORIENTED_EDGE('',*,*,#9254,.F.);
#12517=ORIENTED_EDGE('',*,*,#9364,.T.);
#12518=ORIENTED_EDGE('',*,*,#9365,.T.);
#12519=ORIENTED_EDGE('',*,*,#9362,.F.);
#12520=ORIENTED_EDGE('',*,*,#9253,.F.);
#12521=ORIENTED_EDGE('',*,*,#9366,.T.);
#12522=ORIENTED_EDGE('',*,*,#9367,.T.);
#12523=ORIENTED_EDGE('',*,*,#9364,.F.);
#12524=ORIENTED_EDGE('',*,*,#9252,.F.);
#12525=ORIENTED_EDGE('',*,*,#9368,.T.);
#12526=ORIENTED_EDGE('',*,*,#9369,.T.);
#12527=ORIENTED_EDGE('',*,*,#9366,.F.);
#12528=ORIENTED_EDGE('',*,*,#9251,.F.);
#12529=ORIENTED_EDGE('',*,*,#9370,.T.);
#12530=ORIENTED_EDGE('',*,*,#9371,.T.);
#12531=ORIENTED_EDGE('',*,*,#9368,.F.);
#12532=ORIENTED_EDGE('',*,*,#9250,.F.);
#12533=ORIENTED_EDGE('',*,*,#9359,.T.);
#12534=ORIENTED_EDGE('',*,*,#9372,.T.);
#12535=ORIENTED_EDGE('',*,*,#9370,.F.);
#12536=ORIENTED_EDGE('',*,*,#9372,.F.);
#12537=ORIENTED_EDGE('',*,*,#9358,.F.);
#12538=ORIENTED_EDGE('',*,*,#9361,.F.);
#12539=ORIENTED_EDGE('',*,*,#9363,.F.);
#12540=ORIENTED_EDGE('',*,*,#9365,.F.);
#12541=ORIENTED_EDGE('',*,*,#9367,.F.);
#12542=ORIENTED_EDGE('',*,*,#9369,.F.);
#12543=ORIENTED_EDGE('',*,*,#9371,.F.);
#12544=ORIENTED_EDGE('',*,*,#9257,.F.);
#12545=ORIENTED_EDGE('',*,*,#9373,.T.);
#12546=ORIENTED_EDGE('',*,*,#9374,.T.);
#12547=ORIENTED_EDGE('',*,*,#9375,.F.);
#12548=ORIENTED_EDGE('',*,*,#9268,.F.);
#12549=ORIENTED_EDGE('',*,*,#9376,.T.);
#12550=ORIENTED_EDGE('',*,*,#9377,.T.);
#12551=ORIENTED_EDGE('',*,*,#9373,.F.);
#12552=ORIENTED_EDGE('',*,*,#9267,.F.);
#12553=ORIENTED_EDGE('',*,*,#9378,.T.);
#12554=ORIENTED_EDGE('',*,*,#9379,.T.);
#12555=ORIENTED_EDGE('',*,*,#9376,.F.);
#12556=ORIENTED_EDGE('',*,*,#9266,.F.);
#12557=ORIENTED_EDGE('',*,*,#9380,.T.);
#12558=ORIENTED_EDGE('',*,*,#9381,.T.);
#12559=ORIENTED_EDGE('',*,*,#9378,.F.);
#12560=ORIENTED_EDGE('',*,*,#9265,.F.);
#12561=ORIENTED_EDGE('',*,*,#9382,.T.);
#12562=ORIENTED_EDGE('',*,*,#9383,.T.);
#12563=ORIENTED_EDGE('',*,*,#9380,.F.);
#12564=ORIENTED_EDGE('',*,*,#9264,.F.);
#12565=ORIENTED_EDGE('',*,*,#9384,.T.);
#12566=ORIENTED_EDGE('',*,*,#9385,.T.);
#12567=ORIENTED_EDGE('',*,*,#9382,.F.);
#12568=ORIENTED_EDGE('',*,*,#9263,.F.);
#12569=ORIENTED_EDGE('',*,*,#9386,.T.);
#12570=ORIENTED_EDGE('',*,*,#9387,.T.);
#12571=ORIENTED_EDGE('',*,*,#9384,.F.);
#12572=ORIENTED_EDGE('',*,*,#9262,.F.);
#12573=ORIENTED_EDGE('',*,*,#9388,.T.);
#12574=ORIENTED_EDGE('',*,*,#9389,.T.);
#12575=ORIENTED_EDGE('',*,*,#9386,.F.);
#12576=ORIENTED_EDGE('',*,*,#9261,.F.);
#12577=ORIENTED_EDGE('',*,*,#9390,.T.);
#12578=ORIENTED_EDGE('',*,*,#9391,.T.);
#12579=ORIENTED_EDGE('',*,*,#9388,.F.);
#12580=ORIENTED_EDGE('',*,*,#9260,.F.);
#12581=ORIENTED_EDGE('',*,*,#9392,.T.);
#12582=ORIENTED_EDGE('',*,*,#9393,.T.);
#12583=ORIENTED_EDGE('',*,*,#9390,.F.);
#12584=ORIENTED_EDGE('',*,*,#9259,.F.);
#12585=ORIENTED_EDGE('',*,*,#9394,.T.);
#12586=ORIENTED_EDGE('',*,*,#9395,.T.);
#12587=ORIENTED_EDGE('',*,*,#9392,.F.);
#12588=ORIENTED_EDGE('',*,*,#9258,.F.);
#12589=ORIENTED_EDGE('',*,*,#9375,.T.);
#12590=ORIENTED_EDGE('',*,*,#9396,.T.);
#12591=ORIENTED_EDGE('',*,*,#9394,.F.);
#12592=ORIENTED_EDGE('',*,*,#9396,.F.);
#12593=ORIENTED_EDGE('',*,*,#9374,.F.);
#12594=ORIENTED_EDGE('',*,*,#9377,.F.);
#12595=ORIENTED_EDGE('',*,*,#9379,.F.);
#12596=ORIENTED_EDGE('',*,*,#9381,.F.);
#12597=ORIENTED_EDGE('',*,*,#9383,.F.);
#12598=ORIENTED_EDGE('',*,*,#9385,.F.);
#12599=ORIENTED_EDGE('',*,*,#9387,.F.);
#12600=ORIENTED_EDGE('',*,*,#9389,.F.);
#12601=ORIENTED_EDGE('',*,*,#9391,.F.);
#12602=ORIENTED_EDGE('',*,*,#9393,.F.);
#12603=ORIENTED_EDGE('',*,*,#9395,.F.);
#12604=ORIENTED_EDGE('',*,*,#9269,.F.);
#12605=ORIENTED_EDGE('',*,*,#9397,.T.);
#12606=ORIENTED_EDGE('',*,*,#9398,.T.);
#12607=ORIENTED_EDGE('',*,*,#9399,.F.);
#12608=ORIENTED_EDGE('',*,*,#9277,.F.);
#12609=ORIENTED_EDGE('',*,*,#9400,.T.);
#12610=ORIENTED_EDGE('',*,*,#9401,.T.);
#12611=ORIENTED_EDGE('',*,*,#9397,.F.);
#12612=ORIENTED_EDGE('',*,*,#9276,.F.);
#12613=ORIENTED_EDGE('',*,*,#9402,.T.);
#12614=ORIENTED_EDGE('',*,*,#9403,.T.);
#12615=ORIENTED_EDGE('',*,*,#9400,.F.);
#12616=ORIENTED_EDGE('',*,*,#9275,.F.);
#12617=ORIENTED_EDGE('',*,*,#9404,.T.);
#12618=ORIENTED_EDGE('',*,*,#9405,.T.);
#12619=ORIENTED_EDGE('',*,*,#9402,.F.);
#12620=ORIENTED_EDGE('',*,*,#9274,.F.);
#12621=ORIENTED_EDGE('',*,*,#9406,.T.);
#12622=ORIENTED_EDGE('',*,*,#9407,.T.);
#12623=ORIENTED_EDGE('',*,*,#9404,.F.);
#12624=ORIENTED_EDGE('',*,*,#9273,.F.);
#12625=ORIENTED_EDGE('',*,*,#9408,.T.);
#12626=ORIENTED_EDGE('',*,*,#9409,.T.);
#12627=ORIENTED_EDGE('',*,*,#9406,.F.);
#12628=ORIENTED_EDGE('',*,*,#9272,.F.);
#12629=ORIENTED_EDGE('',*,*,#9410,.T.);
#12630=ORIENTED_EDGE('',*,*,#9411,.T.);
#12631=ORIENTED_EDGE('',*,*,#9408,.F.);
#12632=ORIENTED_EDGE('',*,*,#9271,.F.);
#12633=ORIENTED_EDGE('',*,*,#9412,.T.);
#12634=ORIENTED_EDGE('',*,*,#9413,.T.);
#12635=ORIENTED_EDGE('',*,*,#9410,.F.);
#12636=ORIENTED_EDGE('',*,*,#9270,.F.);
#12637=ORIENTED_EDGE('',*,*,#9399,.T.);
#12638=ORIENTED_EDGE('',*,*,#9414,.T.);
#12639=ORIENTED_EDGE('',*,*,#9412,.F.);
#12640=ORIENTED_EDGE('',*,*,#9414,.F.);
#12641=ORIENTED_EDGE('',*,*,#9398,.F.);
#12642=ORIENTED_EDGE('',*,*,#9401,.F.);
#12643=ORIENTED_EDGE('',*,*,#9403,.F.);
#12644=ORIENTED_EDGE('',*,*,#9405,.F.);
#12645=ORIENTED_EDGE('',*,*,#9407,.F.);
#12646=ORIENTED_EDGE('',*,*,#9409,.F.);
#12647=ORIENTED_EDGE('',*,*,#9411,.F.);
#12648=ORIENTED_EDGE('',*,*,#9413,.F.);
#12649=ORIENTED_EDGE('',*,*,#9278,.F.);
#12650=ORIENTED_EDGE('',*,*,#9415,.T.);
#12651=ORIENTED_EDGE('',*,*,#9416,.T.);
#12652=ORIENTED_EDGE('',*,*,#9417,.F.);
#12653=ORIENTED_EDGE('',*,*,#9306,.F.);
#12654=ORIENTED_EDGE('',*,*,#9418,.T.);
#12655=ORIENTED_EDGE('',*,*,#9419,.T.);
#12656=ORIENTED_EDGE('',*,*,#9415,.F.);
#12657=ORIENTED_EDGE('',*,*,#9305,.F.);
#12658=ORIENTED_EDGE('',*,*,#9420,.T.);
#12659=ORIENTED_EDGE('',*,*,#9421,.T.);
#12660=ORIENTED_EDGE('',*,*,#9418,.F.);
#12661=ORIENTED_EDGE('',*,*,#9304,.F.);
#12662=ORIENTED_EDGE('',*,*,#9422,.T.);
#12663=ORIENTED_EDGE('',*,*,#9423,.T.);
#12664=ORIENTED_EDGE('',*,*,#9420,.F.);
#12665=ORIENTED_EDGE('',*,*,#9303,.F.);
#12666=ORIENTED_EDGE('',*,*,#9424,.T.);
#12667=ORIENTED_EDGE('',*,*,#9425,.T.);
#12668=ORIENTED_EDGE('',*,*,#9422,.F.);
#12669=ORIENTED_EDGE('',*,*,#9302,.F.);
#12670=ORIENTED_EDGE('',*,*,#9426,.T.);
#12671=ORIENTED_EDGE('',*,*,#9427,.T.);
#12672=ORIENTED_EDGE('',*,*,#9424,.F.);
#12673=ORIENTED_EDGE('',*,*,#9301,.F.);
#12674=ORIENTED_EDGE('',*,*,#9428,.T.);
#12675=ORIENTED_EDGE('',*,*,#9429,.T.);
#12676=ORIENTED_EDGE('',*,*,#9426,.F.);
#12677=ORIENTED_EDGE('',*,*,#9300,.F.);
#12678=ORIENTED_EDGE('',*,*,#9430,.T.);
#12679=ORIENTED_EDGE('',*,*,#9431,.T.);
#12680=ORIENTED_EDGE('',*,*,#9428,.F.);
#12681=ORIENTED_EDGE('',*,*,#9299,.F.);
#12682=ORIENTED_EDGE('',*,*,#9432,.T.);
#12683=ORIENTED_EDGE('',*,*,#9433,.T.);
#12684=ORIENTED_EDGE('',*,*,#9430,.F.);
#12685=ORIENTED_EDGE('',*,*,#9298,.F.);
#12686=ORIENTED_EDGE('',*,*,#9434,.T.);
#12687=ORIENTED_EDGE('',*,*,#9435,.T.);
#12688=ORIENTED_EDGE('',*,*,#9432,.F.);
#12689=ORIENTED_EDGE('',*,*,#9297,.F.);
#12690=ORIENTED_EDGE('',*,*,#9436,.T.);
#12691=ORIENTED_EDGE('',*,*,#9437,.T.);
#12692=ORIENTED_EDGE('',*,*,#9434,.F.);
#12693=ORIENTED_EDGE('',*,*,#9296,.F.);
#12694=ORIENTED_EDGE('',*,*,#9438,.T.);
#12695=ORIENTED_EDGE('',*,*,#9439,.T.);
#12696=ORIENTED_EDGE('',*,*,#9436,.F.);
#12697=ORIENTED_EDGE('',*,*,#9295,.F.);
#12698=ORIENTED_EDGE('',*,*,#9440,.T.);
#12699=ORIENTED_EDGE('',*,*,#9441,.T.);
#12700=ORIENTED_EDGE('',*,*,#9438,.F.);
#12701=ORIENTED_EDGE('',*,*,#9294,.F.);
#12702=ORIENTED_EDGE('',*,*,#9442,.T.);
#12703=ORIENTED_EDGE('',*,*,#9443,.T.);
#12704=ORIENTED_EDGE('',*,*,#9440,.F.);
#12705=ORIENTED_EDGE('',*,*,#9293,.F.);
#12706=ORIENTED_EDGE('',*,*,#9444,.T.);
#12707=ORIENTED_EDGE('',*,*,#9445,.T.);
#12708=ORIENTED_EDGE('',*,*,#9442,.F.);
#12709=ORIENTED_EDGE('',*,*,#9292,.F.);
#12710=ORIENTED_EDGE('',*,*,#9446,.T.);
#12711=ORIENTED_EDGE('',*,*,#9447,.T.);
#12712=ORIENTED_EDGE('',*,*,#9444,.F.);
#12713=ORIENTED_EDGE('',*,*,#9291,.F.);
#12714=ORIENTED_EDGE('',*,*,#9448,.T.);
#12715=ORIENTED_EDGE('',*,*,#9449,.T.);
#12716=ORIENTED_EDGE('',*,*,#9446,.F.);
#12717=ORIENTED_EDGE('',*,*,#9290,.F.);
#12718=ORIENTED_EDGE('',*,*,#9450,.T.);
#12719=ORIENTED_EDGE('',*,*,#9451,.T.);
#12720=ORIENTED_EDGE('',*,*,#9448,.F.);
#12721=ORIENTED_EDGE('',*,*,#9289,.F.);
#12722=ORIENTED_EDGE('',*,*,#9452,.T.);
#12723=ORIENTED_EDGE('',*,*,#9453,.T.);
#12724=ORIENTED_EDGE('',*,*,#9450,.F.);
#12725=ORIENTED_EDGE('',*,*,#9288,.F.);
#12726=ORIENTED_EDGE('',*,*,#9454,.T.);
#12727=ORIENTED_EDGE('',*,*,#9455,.T.);
#12728=ORIENTED_EDGE('',*,*,#9452,.F.);
#12729=ORIENTED_EDGE('',*,*,#9287,.F.);
#12730=ORIENTED_EDGE('',*,*,#9456,.T.);
#12731=ORIENTED_EDGE('',*,*,#9457,.T.);
#12732=ORIENTED_EDGE('',*,*,#9454,.F.);
#12733=ORIENTED_EDGE('',*,*,#9286,.F.);
#12734=ORIENTED_EDGE('',*,*,#9458,.T.);
#12735=ORIENTED_EDGE('',*,*,#9459,.T.);
#12736=ORIENTED_EDGE('',*,*,#9456,.F.);
#12737=ORIENTED_EDGE('',*,*,#9285,.F.);
#12738=ORIENTED_EDGE('',*,*,#9460,.T.);
#12739=ORIENTED_EDGE('',*,*,#9461,.T.);
#12740=ORIENTED_EDGE('',*,*,#9458,.F.);
#12741=ORIENTED_EDGE('',*,*,#9284,.F.);
#12742=ORIENTED_EDGE('',*,*,#9462,.T.);
#12743=ORIENTED_EDGE('',*,*,#9463,.T.);
#12744=ORIENTED_EDGE('',*,*,#9460,.F.);
#12745=ORIENTED_EDGE('',*,*,#9283,.F.);
#12746=ORIENTED_EDGE('',*,*,#9464,.T.);
#12747=ORIENTED_EDGE('',*,*,#9465,.T.);
#12748=ORIENTED_EDGE('',*,*,#9462,.F.);
#12749=ORIENTED_EDGE('',*,*,#9282,.F.);
#12750=ORIENTED_EDGE('',*,*,#9466,.T.);
#12751=ORIENTED_EDGE('',*,*,#9467,.T.);
#12752=ORIENTED_EDGE('',*,*,#9464,.F.);
#12753=ORIENTED_EDGE('',*,*,#9281,.F.);
#12754=ORIENTED_EDGE('',*,*,#9468,.T.);
#12755=ORIENTED_EDGE('',*,*,#9469,.T.);
#12756=ORIENTED_EDGE('',*,*,#9466,.F.);
#12757=ORIENTED_EDGE('',*,*,#9280,.F.);
#12758=ORIENTED_EDGE('',*,*,#9470,.T.);
#12759=ORIENTED_EDGE('',*,*,#9471,.T.);
#12760=ORIENTED_EDGE('',*,*,#9468,.F.);
#12761=ORIENTED_EDGE('',*,*,#9279,.F.);
#12762=ORIENTED_EDGE('',*,*,#9417,.T.);
#12763=ORIENTED_EDGE('',*,*,#9472,.T.);
#12764=ORIENTED_EDGE('',*,*,#9470,.F.);
#12765=ORIENTED_EDGE('',*,*,#9472,.F.);
#12766=ORIENTED_EDGE('',*,*,#9416,.F.);
#12767=ORIENTED_EDGE('',*,*,#9419,.F.);
#12768=ORIENTED_EDGE('',*,*,#9421,.F.);
#12769=ORIENTED_EDGE('',*,*,#9423,.F.);
#12770=ORIENTED_EDGE('',*,*,#9425,.F.);
#12771=ORIENTED_EDGE('',*,*,#9427,.F.);
#12772=ORIENTED_EDGE('',*,*,#9429,.F.);
#12773=ORIENTED_EDGE('',*,*,#9431,.F.);
#12774=ORIENTED_EDGE('',*,*,#9433,.F.);
#12775=ORIENTED_EDGE('',*,*,#9435,.F.);
#12776=ORIENTED_EDGE('',*,*,#9437,.F.);
#12777=ORIENTED_EDGE('',*,*,#9439,.F.);
#12778=ORIENTED_EDGE('',*,*,#9441,.F.);
#12779=ORIENTED_EDGE('',*,*,#9443,.F.);
#12780=ORIENTED_EDGE('',*,*,#9445,.F.);
#12781=ORIENTED_EDGE('',*,*,#9447,.F.);
#12782=ORIENTED_EDGE('',*,*,#9449,.F.);
#12783=ORIENTED_EDGE('',*,*,#9451,.F.);
#12784=ORIENTED_EDGE('',*,*,#9453,.F.);
#12785=ORIENTED_EDGE('',*,*,#9455,.F.);
#12786=ORIENTED_EDGE('',*,*,#9457,.F.);
#12787=ORIENTED_EDGE('',*,*,#9459,.F.);
#12788=ORIENTED_EDGE('',*,*,#9461,.F.);
#12789=ORIENTED_EDGE('',*,*,#9463,.F.);
#12790=ORIENTED_EDGE('',*,*,#9465,.F.);
#12791=ORIENTED_EDGE('',*,*,#9467,.F.);
#12792=ORIENTED_EDGE('',*,*,#9469,.F.);
#12793=ORIENTED_EDGE('',*,*,#9471,.F.);
#12794=ORIENTED_EDGE('',*,*,#9206,.F.);
#12795=ORIENTED_EDGE('',*,*,#9213,.F.);
#12796=ORIENTED_EDGE('',*,*,#9151,.F.);
#12797=ORIENTED_EDGE('',*,*,#9217,.F.);
#12798=ORIENTED_EDGE('',*,*,#9473,.F.);
#12799=ORIENTED_EDGE('',*,*,#9474,.F.);
#12800=ORIENTED_EDGE('',*,*,#9147,.F.);
#12801=ORIENTED_EDGE('',*,*,#9475,.T.);
#12802=ORIENTED_EDGE('',*,*,#9201,.T.);
#12803=ORIENTED_EDGE('',*,*,#9473,.T.);
#12804=ORIENTED_EDGE('',*,*,#9216,.F.);
#12805=ORIENTED_EDGE('',*,*,#9154,.T.);
#12806=ORIENTED_EDGE('',*,*,#9207,.F.);
#12807=ORIENTED_EDGE('',*,*,#9474,.T.);
#12808=ORIENTED_EDGE('',*,*,#9200,.T.);
#12809=ORIENTED_EDGE('',*,*,#9220,.T.);
#12810=ORIENTED_EDGE('',*,*,#9221,.F.);
#12811=ORIENTED_EDGE('',*,*,#9214,.T.);
#12812=ORIENTED_EDGE('',*,*,#9171,.F.);
#12813=ORIENTED_EDGE('',*,*,#9193,.F.);
#12814=ORIENTED_EDGE('',*,*,#9476,.F.);
#12815=ORIENTED_EDGE('',*,*,#9180,.F.);
#12816=ORIENTED_EDGE('',*,*,#9146,.F.);
#12817=ORIENTED_EDGE('',*,*,#9153,.F.);
#12818=ORIENTED_EDGE('',*,*,#9163,.F.);
#12819=ORIENTED_EDGE('',*,*,#9157,.F.);
#12820=ORIENTED_EDGE('',*,*,#9317,.F.);
#12821=ORIENTED_EDGE('',*,*,#9475,.F.);
#12822=ORIENTED_EDGE('',*,*,#9186,.F.);
#12823=ORIENTED_EDGE('',*,*,#9312,.F.);
#12824=ORIENTED_EDGE('',*,*,#9222,.F.);
#12825=ORIENTED_EDGE('',*,*,#9477,.T.);
#12826=ORIENTED_EDGE('',*,*,#9189,.F.);
#12827=ORIENTED_EDGE('',*,*,#9477,.F.);
#12828=ORIENTED_EDGE('',*,*,#9228,.F.);
#12829=ORIENTED_EDGE('',*,*,#9476,.T.);
#12830=ORIENTED_EDGE('',*,*,#9478,.F.);
#12831=ORIENTED_EDGE('',*,*,#9479,.F.);
#12832=ORIENTED_EDGE('',*,*,#9480,.T.);
#12833=ORIENTED_EDGE('',*,*,#9478,.T.);
#12834=ORIENTED_EDGE('',*,*,#9480,.F.);
#12835=ORIENTED_EDGE('',*,*,#9481,.F.);
#12836=ORIENTED_EDGE('',*,*,#9482,.T.);
#12837=ORIENTED_EDGE('',*,*,#9479,.T.);
#12838=ORIENTED_EDGE('',*,*,#9482,.F.);
#12839=ORIENTED_EDGE('',*,*,#9481,.T.);
#12840=ORIENTED_EDGE('',*,*,#9483,.F.);
#12841=ORIENTED_EDGE('',*,*,#9484,.F.);
#12842=ORIENTED_EDGE('',*,*,#9485,.T.);
#12843=ORIENTED_EDGE('',*,*,#9483,.T.);
#12844=ORIENTED_EDGE('',*,*,#9485,.F.);
#12845=ORIENTED_EDGE('',*,*,#9486,.F.);
#12846=ORIENTED_EDGE('',*,*,#9484,.T.);
#12847=ORIENTED_EDGE('',*,*,#9487,.F.);
#12848=ORIENTED_EDGE('',*,*,#9488,.T.);
#12849=ORIENTED_EDGE('',*,*,#9486,.T.);
#12850=ORIENTED_EDGE('',*,*,#9488,.F.);
#12851=ORIENTED_EDGE('',*,*,#9487,.T.);
#12852=ORIENTED_EDGE('',*,*,#9489,.F.);
#12853=ORIENTED_EDGE('',*,*,#9490,.F.);
#12854=ORIENTED_EDGE('',*,*,#9491,.T.);
#12855=ORIENTED_EDGE('',*,*,#9489,.T.);
#12856=ORIENTED_EDGE('',*,*,#9491,.F.);
#12857=ORIENTED_EDGE('',*,*,#9492,.F.);
#12858=ORIENTED_EDGE('',*,*,#9490,.T.);
#12859=ORIENTED_EDGE('',*,*,#9493,.F.);
#12860=ORIENTED_EDGE('',*,*,#9494,.T.);
#12861=ORIENTED_EDGE('',*,*,#9492,.T.);
#12862=ORIENTED_EDGE('',*,*,#9494,.F.);
#12863=ORIENTED_EDGE('',*,*,#9495,.F.);
#12864=ORIENTED_EDGE('',*,*,#9496,.T.);
#12865=ORIENTED_EDGE('',*,*,#9493,.T.);
#12866=ORIENTED_EDGE('',*,*,#9496,.F.);
#12867=ORIENTED_EDGE('',*,*,#9495,.T.);
#12868=ORIENTED_EDGE('',*,*,#9497,.F.);
#12869=ORIENTED_EDGE('',*,*,#9498,.T.);
#12870=ORIENTED_EDGE('',*,*,#9499,.T.);
#12871=ORIENTED_EDGE('',*,*,#9500,.T.);
#12872=ORIENTED_EDGE('',*,*,#9501,.F.);
#12873=ORIENTED_EDGE('',*,*,#9502,.T.);
#12874=ORIENTED_EDGE('',*,*,#9497,.T.);
#12875=ORIENTED_EDGE('',*,*,#9503,.T.);
#12876=ORIENTED_EDGE('',*,*,#9504,.F.);
#12877=ORIENTED_EDGE('',*,*,#9505,.T.);
#12878=ORIENTED_EDGE('',*,*,#9501,.T.);
#12879=ORIENTED_EDGE('',*,*,#9506,.T.);
#12880=ORIENTED_EDGE('',*,*,#9507,.F.);
#12881=ORIENTED_EDGE('',*,*,#9508,.T.);
#12882=ORIENTED_EDGE('',*,*,#9504,.T.);
#12883=ORIENTED_EDGE('',*,*,#9509,.T.);
#12884=ORIENTED_EDGE('',*,*,#9510,.F.);
#12885=ORIENTED_EDGE('',*,*,#9511,.T.);
#12886=ORIENTED_EDGE('',*,*,#9507,.T.);
#12887=ORIENTED_EDGE('',*,*,#9512,.T.);
#12888=ORIENTED_EDGE('',*,*,#9513,.F.);
#12889=ORIENTED_EDGE('',*,*,#9514,.T.);
#12890=ORIENTED_EDGE('',*,*,#9510,.T.);
#12891=ORIENTED_EDGE('',*,*,#9515,.T.);
#12892=ORIENTED_EDGE('',*,*,#9516,.F.);
#12893=ORIENTED_EDGE('',*,*,#9517,.T.);
#12894=ORIENTED_EDGE('',*,*,#9513,.T.);
#12895=ORIENTED_EDGE('',*,*,#9518,.T.);
#12896=ORIENTED_EDGE('',*,*,#9519,.F.);
#12897=ORIENTED_EDGE('',*,*,#9520,.T.);
#12898=ORIENTED_EDGE('',*,*,#9516,.T.);
#12899=ORIENTED_EDGE('',*,*,#9521,.T.);
#12900=ORIENTED_EDGE('',*,*,#9522,.F.);
#12901=ORIENTED_EDGE('',*,*,#9523,.T.);
#12902=ORIENTED_EDGE('',*,*,#9519,.T.);
#12903=ORIENTED_EDGE('',*,*,#9524,.T.);
#12904=ORIENTED_EDGE('',*,*,#9525,.F.);
#12905=ORIENTED_EDGE('',*,*,#9526,.T.);
#12906=ORIENTED_EDGE('',*,*,#9522,.T.);
#12907=ORIENTED_EDGE('',*,*,#9527,.T.);
#12908=ORIENTED_EDGE('',*,*,#9528,.F.);
#12909=ORIENTED_EDGE('',*,*,#9529,.T.);
#12910=ORIENTED_EDGE('',*,*,#9525,.T.);
#12911=ORIENTED_EDGE('',*,*,#9530,.T.);
#12912=ORIENTED_EDGE('',*,*,#9531,.F.);
#12913=ORIENTED_EDGE('',*,*,#9532,.T.);
#12914=ORIENTED_EDGE('',*,*,#9528,.T.);
#12915=ORIENTED_EDGE('',*,*,#9533,.T.);
#12916=ORIENTED_EDGE('',*,*,#9534,.F.);
#12917=ORIENTED_EDGE('',*,*,#9535,.T.);
#12918=ORIENTED_EDGE('',*,*,#9536,.F.);
#12919=ORIENTED_EDGE('',*,*,#9537,.F.);
#12920=ORIENTED_EDGE('',*,*,#9538,.F.);
#12921=ORIENTED_EDGE('',*,*,#9539,.T.);
#12922=ORIENTED_EDGE('',*,*,#9534,.T.);
#12923=ORIENTED_EDGE('',*,*,#9540,.F.);
#12924=ORIENTED_EDGE('',*,*,#9541,.F.);
#12925=ORIENTED_EDGE('',*,*,#9542,.T.);
#12926=ORIENTED_EDGE('',*,*,#9538,.T.);
#12927=ORIENTED_EDGE('',*,*,#9543,.F.);
#12928=ORIENTED_EDGE('',*,*,#9544,.F.);
#12929=ORIENTED_EDGE('',*,*,#9545,.T.);
#12930=ORIENTED_EDGE('',*,*,#9541,.T.);
#12931=ORIENTED_EDGE('',*,*,#9546,.F.);
#12932=ORIENTED_EDGE('',*,*,#9547,.F.);
#12933=ORIENTED_EDGE('',*,*,#9548,.T.);
#12934=ORIENTED_EDGE('',*,*,#9544,.T.);
#12935=ORIENTED_EDGE('',*,*,#9549,.F.);
#12936=ORIENTED_EDGE('',*,*,#9550,.F.);
#12937=ORIENTED_EDGE('',*,*,#9551,.T.);
#12938=ORIENTED_EDGE('',*,*,#9547,.T.);
#12939=ORIENTED_EDGE('',*,*,#9552,.F.);
#12940=ORIENTED_EDGE('',*,*,#9553,.F.);
#12941=ORIENTED_EDGE('',*,*,#9554,.T.);
#12942=ORIENTED_EDGE('',*,*,#9550,.T.);
#12943=ORIENTED_EDGE('',*,*,#9555,.F.);
#12944=ORIENTED_EDGE('',*,*,#9556,.F.);
#12945=ORIENTED_EDGE('',*,*,#9557,.T.);
#12946=ORIENTED_EDGE('',*,*,#9553,.T.);
#12947=ORIENTED_EDGE('',*,*,#9558,.F.);
#12948=ORIENTED_EDGE('',*,*,#9559,.F.);
#12949=ORIENTED_EDGE('',*,*,#9560,.T.);
#12950=ORIENTED_EDGE('',*,*,#9556,.T.);
#12951=ORIENTED_EDGE('',*,*,#9561,.F.);
#12952=ORIENTED_EDGE('',*,*,#9562,.F.);
#12953=ORIENTED_EDGE('',*,*,#9563,.T.);
#12954=ORIENTED_EDGE('',*,*,#9559,.T.);
#12955=ORIENTED_EDGE('',*,*,#9564,.F.);
#12956=ORIENTED_EDGE('',*,*,#9565,.F.);
#12957=ORIENTED_EDGE('',*,*,#9566,.T.);
#12958=ORIENTED_EDGE('',*,*,#9562,.T.);
#12959=ORIENTED_EDGE('',*,*,#9567,.F.);
#12960=ORIENTED_EDGE('',*,*,#9568,.T.);
#12961=ORIENTED_EDGE('',*,*,#9569,.T.);
#12962=ORIENTED_EDGE('',*,*,#9570,.T.);
#12963=ORIENTED_EDGE('',*,*,#9571,.T.);
#12964=ORIENTED_EDGE('',*,*,#9569,.F.);
#12965=ORIENTED_EDGE('',*,*,#9570,.F.);
#12966=ORIENTED_EDGE('',*,*,#9571,.F.);
#12967=ORIENTED_EDGE('',*,*,#9572,.T.);
#12968=ORIENTED_EDGE('',*,*,#9573,.F.);
#12969=ORIENTED_EDGE('',*,*,#9574,.F.);
#12970=ORIENTED_EDGE('',*,*,#9572,.F.);
#12971=ORIENTED_EDGE('',*,*,#9568,.F.);
#12972=ORIENTED_EDGE('',*,*,#9575,.T.);
#12973=ORIENTED_EDGE('',*,*,#9576,.T.);
#12974=ORIENTED_EDGE('',*,*,#9577,.T.);
#12975=ORIENTED_EDGE('',*,*,#9499,.F.);
#12976=ORIENTED_EDGE('',*,*,#9573,.T.);
#12977=ORIENTED_EDGE('',*,*,#9574,.T.);
#12978=ORIENTED_EDGE('',*,*,#9578,.T.);
#12979=ORIENTED_EDGE('',*,*,#9579,.T.);
#12980=ORIENTED_EDGE('',*,*,#9580,.T.);
#12981=ORIENTED_EDGE('',*,*,#9578,.F.);
#12982=ORIENTED_EDGE('',*,*,#9579,.F.);
#12983=ORIENTED_EDGE('',*,*,#9580,.F.);
#12984=ORIENTED_EDGE('',*,*,#9581,.T.);
#12985=ORIENTED_EDGE('',*,*,#9582,.T.);
#12986=ORIENTED_EDGE('',*,*,#9581,.F.);
#12987=ORIENTED_EDGE('',*,*,#9536,.T.);
#12988=ORIENTED_EDGE('',*,*,#9583,.T.);
#12989=ORIENTED_EDGE('',*,*,#9584,.F.);
#12990=ORIENTED_EDGE('',*,*,#9585,.F.);
#12991=ORIENTED_EDGE('',*,*,#9586,.T.);
#12992=ORIENTED_EDGE('',*,*,#9586,.F.);
#12993=ORIENTED_EDGE('',*,*,#9587,.F.);
#12994=ORIENTED_EDGE('',*,*,#9533,.F.);
#12995=ORIENTED_EDGE('',*,*,#9530,.F.);
#12996=ORIENTED_EDGE('',*,*,#9527,.F.);
#12997=ORIENTED_EDGE('',*,*,#9524,.F.);
#12998=ORIENTED_EDGE('',*,*,#9521,.F.);
#12999=ORIENTED_EDGE('',*,*,#9518,.F.);
#13000=ORIENTED_EDGE('',*,*,#9515,.F.);
#13001=ORIENTED_EDGE('',*,*,#9512,.F.);
#13002=ORIENTED_EDGE('',*,*,#9509,.F.);
#13003=ORIENTED_EDGE('',*,*,#9506,.F.);
#13004=ORIENTED_EDGE('',*,*,#9503,.F.);
#13005=ORIENTED_EDGE('',*,*,#9500,.F.);
#13006=ORIENTED_EDGE('',*,*,#9577,.F.);
#13007=ORIENTED_EDGE('',*,*,#9588,.T.);
#13008=ORIENTED_EDGE('',*,*,#9567,.T.);
#13009=ORIENTED_EDGE('',*,*,#9564,.T.);
#13010=ORIENTED_EDGE('',*,*,#9561,.T.);
#13011=ORIENTED_EDGE('',*,*,#9558,.T.);
#13012=ORIENTED_EDGE('',*,*,#9555,.T.);
#13013=ORIENTED_EDGE('',*,*,#9552,.T.);
#13014=ORIENTED_EDGE('',*,*,#9549,.T.);
#13015=ORIENTED_EDGE('',*,*,#9546,.T.);
#13016=ORIENTED_EDGE('',*,*,#9543,.T.);
#13017=ORIENTED_EDGE('',*,*,#9540,.T.);
#13018=ORIENTED_EDGE('',*,*,#9537,.T.);
#13019=ORIENTED_EDGE('',*,*,#9565,.T.);
#13020=ORIENTED_EDGE('',*,*,#9588,.F.);
#13021=ORIENTED_EDGE('',*,*,#9576,.F.);
#13022=ORIENTED_EDGE('',*,*,#9589,.T.);
#13023=ORIENTED_EDGE('',*,*,#9583,.F.);
#13024=ORIENTED_EDGE('',*,*,#9535,.F.);
#13025=ORIENTED_EDGE('',*,*,#9539,.F.);
#13026=ORIENTED_EDGE('',*,*,#9542,.F.);
#13027=ORIENTED_EDGE('',*,*,#9545,.F.);
#13028=ORIENTED_EDGE('',*,*,#9548,.F.);
#13029=ORIENTED_EDGE('',*,*,#9551,.F.);
#13030=ORIENTED_EDGE('',*,*,#9554,.F.);
#13031=ORIENTED_EDGE('',*,*,#9557,.F.);
#13032=ORIENTED_EDGE('',*,*,#9560,.F.);
#13033=ORIENTED_EDGE('',*,*,#9563,.F.);
#13034=ORIENTED_EDGE('',*,*,#9566,.F.);
#13035=ORIENTED_EDGE('',*,*,#9589,.F.);
#13036=ORIENTED_EDGE('',*,*,#9575,.F.);
#13037=ORIENTED_EDGE('',*,*,#9498,.F.);
#13038=ORIENTED_EDGE('',*,*,#9502,.F.);
#13039=ORIENTED_EDGE('',*,*,#9505,.F.);
#13040=ORIENTED_EDGE('',*,*,#9508,.F.);
#13041=ORIENTED_EDGE('',*,*,#9511,.F.);
#13042=ORIENTED_EDGE('',*,*,#9514,.F.);
#13043=ORIENTED_EDGE('',*,*,#9517,.F.);
#13044=ORIENTED_EDGE('',*,*,#9520,.F.);
#13045=ORIENTED_EDGE('',*,*,#9523,.F.);
#13046=ORIENTED_EDGE('',*,*,#9526,.F.);
#13047=ORIENTED_EDGE('',*,*,#9529,.F.);
#13048=ORIENTED_EDGE('',*,*,#9532,.F.);
#13049=ORIENTED_EDGE('',*,*,#9590,.F.);
#13050=ORIENTED_EDGE('',*,*,#9531,.T.);
#13051=ORIENTED_EDGE('',*,*,#9587,.T.);
#13052=ORIENTED_EDGE('',*,*,#9591,.F.);
#13053=ORIENTED_EDGE('',*,*,#9590,.T.);
#13054=ORIENTED_EDGE('',*,*,#9592,.T.);
#13055=ORIENTED_EDGE('',*,*,#9593,.T.);
#13056=ORIENTED_EDGE('',*,*,#9594,.F.);
#13057=ORIENTED_EDGE('',*,*,#9593,.F.);
#13058=ORIENTED_EDGE('',*,*,#9595,.F.);
#13059=ORIENTED_EDGE('',*,*,#9594,.T.);
#13060=ORIENTED_EDGE('',*,*,#9582,.F.);
#13061=ORIENTED_EDGE('',*,*,#9596,.T.);
#13062=ORIENTED_EDGE('',*,*,#9595,.T.);
#13063=ORIENTED_EDGE('',*,*,#9596,.F.);
#13064=ORIENTED_EDGE('',*,*,#9597,.F.);
#13065=ORIENTED_EDGE('',*,*,#9598,.T.);
#13066=ORIENTED_EDGE('',*,*,#9584,.T.);
#13067=ORIENTED_EDGE('',*,*,#9591,.T.);
#13068=ORIENTED_EDGE('',*,*,#9585,.T.);
#13069=ORIENTED_EDGE('',*,*,#9598,.F.);
#13070=ORIENTED_EDGE('',*,*,#9597,.T.);
#13071=ORIENTED_EDGE('',*,*,#9599,.F.);
#13072=ORIENTED_EDGE('',*,*,#9599,.T.);
#13073=ORIENTED_EDGE('',*,*,#9600,.T.);
#13074=ORIENTED_EDGE('',*,*,#9601,.F.);
#13075=ORIENTED_EDGE('',*,*,#9600,.F.);
#13076=ORIENTED_EDGE('',*,*,#9602,.F.);
#13077=ORIENTED_EDGE('',*,*,#9601,.T.);
#13078=ORIENTED_EDGE('',*,*,#9602,.T.);
#13079=ORIENTED_EDGE('',*,*,#9603,.T.);
#13080=ORIENTED_EDGE('',*,*,#9604,.F.);
#13081=ORIENTED_EDGE('',*,*,#9603,.F.);
#13082=ORIENTED_EDGE('',*,*,#9604,.T.);
#13083=ORIENTED_EDGE('',*,*,#9592,.F.);
#13084=ORIENTED_EDGE('',*,*,#9605,.F.);
#13085=ORIENTED_EDGE('',*,*,#9606,.T.);
#13086=ORIENTED_EDGE('',*,*,#9607,.T.);
#13087=ORIENTED_EDGE('',*,*,#9608,.T.);
#13088=ORIENTED_EDGE('',*,*,#9609,.F.);
#13089=ORIENTED_EDGE('',*,*,#9610,.T.);
#13090=ORIENTED_EDGE('',*,*,#9605,.T.);
#13091=ORIENTED_EDGE('',*,*,#9611,.T.);
#13092=ORIENTED_EDGE('',*,*,#9612,.F.);
#13093=ORIENTED_EDGE('',*,*,#9613,.T.);
#13094=ORIENTED_EDGE('',*,*,#9609,.T.);
#13095=ORIENTED_EDGE('',*,*,#9614,.T.);
#13096=ORIENTED_EDGE('',*,*,#9615,.F.);
#13097=ORIENTED_EDGE('',*,*,#9616,.T.);
#13098=ORIENTED_EDGE('',*,*,#9612,.T.);
#13099=ORIENTED_EDGE('',*,*,#9617,.T.);
#13100=ORIENTED_EDGE('',*,*,#9618,.F.);
#13101=ORIENTED_EDGE('',*,*,#9619,.T.);
#13102=ORIENTED_EDGE('',*,*,#9615,.T.);
#13103=ORIENTED_EDGE('',*,*,#9620,.T.);
#13104=ORIENTED_EDGE('',*,*,#9621,.F.);
#13105=ORIENTED_EDGE('',*,*,#9622,.T.);
#13106=ORIENTED_EDGE('',*,*,#9618,.T.);
#13107=ORIENTED_EDGE('',*,*,#9623,.T.);
#13108=ORIENTED_EDGE('',*,*,#9624,.F.);
#13109=ORIENTED_EDGE('',*,*,#9625,.T.);
#13110=ORIENTED_EDGE('',*,*,#9621,.T.);
#13111=ORIENTED_EDGE('',*,*,#9626,.T.);
#13112=ORIENTED_EDGE('',*,*,#9627,.F.);
#13113=ORIENTED_EDGE('',*,*,#9628,.T.);
#13114=ORIENTED_EDGE('',*,*,#9624,.T.);
#13115=ORIENTED_EDGE('',*,*,#9629,.T.);
#13116=ORIENTED_EDGE('',*,*,#9630,.F.);
#13117=ORIENTED_EDGE('',*,*,#9631,.T.);
#13118=ORIENTED_EDGE('',*,*,#9627,.T.);
#13119=ORIENTED_EDGE('',*,*,#9632,.T.);
#13120=ORIENTED_EDGE('',*,*,#9633,.F.);
#13121=ORIENTED_EDGE('',*,*,#9634,.T.);
#13122=ORIENTED_EDGE('',*,*,#9630,.T.);
#13123=ORIENTED_EDGE('',*,*,#9635,.T.);
#13124=ORIENTED_EDGE('',*,*,#9636,.F.);
#13125=ORIENTED_EDGE('',*,*,#9637,.T.);
#13126=ORIENTED_EDGE('',*,*,#9633,.T.);
#13127=ORIENTED_EDGE('',*,*,#9638,.T.);
#13128=ORIENTED_EDGE('',*,*,#9639,.F.);
#13129=ORIENTED_EDGE('',*,*,#9640,.T.);
#13130=ORIENTED_EDGE('',*,*,#9636,.T.);
#13131=ORIENTED_EDGE('',*,*,#9641,.T.);
#13132=ORIENTED_EDGE('',*,*,#9642,.F.);
#13133=ORIENTED_EDGE('',*,*,#9643,.T.);
#13134=ORIENTED_EDGE('',*,*,#9639,.T.);
#13135=ORIENTED_EDGE('',*,*,#9644,.T.);
#13136=ORIENTED_EDGE('',*,*,#9645,.F.);
#13137=ORIENTED_EDGE('',*,*,#9646,.T.);
#13138=ORIENTED_EDGE('',*,*,#9647,.F.);
#13139=ORIENTED_EDGE('',*,*,#9648,.F.);
#13140=ORIENTED_EDGE('',*,*,#9649,.T.);
#13141=ORIENTED_EDGE('',*,*,#9645,.T.);
#13142=ORIENTED_EDGE('',*,*,#9650,.F.);
#13143=ORIENTED_EDGE('',*,*,#9651,.F.);
#13144=ORIENTED_EDGE('',*,*,#9652,.F.);
#13145=ORIENTED_EDGE('',*,*,#9653,.T.);
#13146=ORIENTED_EDGE('',*,*,#9648,.T.);
#13147=ORIENTED_EDGE('',*,*,#9654,.F.);
#13148=ORIENTED_EDGE('',*,*,#9655,.F.);
#13149=ORIENTED_EDGE('',*,*,#9656,.T.);
#13150=ORIENTED_EDGE('',*,*,#9652,.T.);
#13151=ORIENTED_EDGE('',*,*,#9657,.F.);
#13152=ORIENTED_EDGE('',*,*,#9658,.F.);
#13153=ORIENTED_EDGE('',*,*,#9659,.T.);
#13154=ORIENTED_EDGE('',*,*,#9655,.T.);
#13155=ORIENTED_EDGE('',*,*,#9660,.F.);
#13156=ORIENTED_EDGE('',*,*,#9661,.F.);
#13157=ORIENTED_EDGE('',*,*,#9662,.T.);
#13158=ORIENTED_EDGE('',*,*,#9658,.T.);
#13159=ORIENTED_EDGE('',*,*,#9663,.F.);
#13160=ORIENTED_EDGE('',*,*,#9664,.F.);
#13161=ORIENTED_EDGE('',*,*,#9665,.T.);
#13162=ORIENTED_EDGE('',*,*,#9661,.T.);
#13163=ORIENTED_EDGE('',*,*,#9666,.F.);
#13164=ORIENTED_EDGE('',*,*,#9667,.F.);
#13165=ORIENTED_EDGE('',*,*,#9668,.T.);
#13166=ORIENTED_EDGE('',*,*,#9664,.T.);
#13167=ORIENTED_EDGE('',*,*,#9669,.F.);
#13168=ORIENTED_EDGE('',*,*,#9670,.F.);
#13169=ORIENTED_EDGE('',*,*,#9671,.T.);
#13170=ORIENTED_EDGE('',*,*,#9667,.T.);
#13171=ORIENTED_EDGE('',*,*,#9672,.F.);
#13172=ORIENTED_EDGE('',*,*,#9673,.F.);
#13173=ORIENTED_EDGE('',*,*,#9674,.T.);
#13174=ORIENTED_EDGE('',*,*,#9670,.T.);
#13175=ORIENTED_EDGE('',*,*,#9675,.F.);
#13176=ORIENTED_EDGE('',*,*,#9676,.F.);
#13177=ORIENTED_EDGE('',*,*,#9677,.T.);
#13178=ORIENTED_EDGE('',*,*,#9673,.T.);
#13179=ORIENTED_EDGE('',*,*,#9678,.F.);
#13180=ORIENTED_EDGE('',*,*,#9679,.F.);
#13181=ORIENTED_EDGE('',*,*,#9680,.T.);
#13182=ORIENTED_EDGE('',*,*,#9676,.T.);
#13183=ORIENTED_EDGE('',*,*,#9681,.F.);
#13184=ORIENTED_EDGE('',*,*,#9682,.F.);
#13185=ORIENTED_EDGE('',*,*,#9683,.T.);
#13186=ORIENTED_EDGE('',*,*,#9679,.T.);
#13187=ORIENTED_EDGE('',*,*,#9684,.F.);
#13188=ORIENTED_EDGE('',*,*,#9685,.T.);
#13189=ORIENTED_EDGE('',*,*,#9686,.T.);
#13190=ORIENTED_EDGE('',*,*,#9687,.T.);
#13191=ORIENTED_EDGE('',*,*,#9688,.T.);
#13192=ORIENTED_EDGE('',*,*,#9689,.T.);
#13193=ORIENTED_EDGE('',*,*,#9690,.T.);
#13194=ORIENTED_EDGE('',*,*,#9686,.F.);
#13195=ORIENTED_EDGE('',*,*,#9691,.T.);
#13196=ORIENTED_EDGE('',*,*,#9692,.T.);
#13197=ORIENTED_EDGE('',*,*,#9693,.T.);
#13198=ORIENTED_EDGE('',*,*,#9694,.T.);
#13199=ORIENTED_EDGE('',*,*,#9695,.T.);
#13200=ORIENTED_EDGE('',*,*,#9696,.T.);
#13201=ORIENTED_EDGE('',*,*,#9697,.T.);
#13202=ORIENTED_EDGE('',*,*,#9688,.F.);
#13203=ORIENTED_EDGE('',*,*,#9698,.F.);
#13204=ORIENTED_EDGE('',*,*,#9690,.F.);
#13205=ORIENTED_EDGE('',*,*,#9699,.T.);
#13206=ORIENTED_EDGE('',*,*,#9700,.T.);
#13207=ORIENTED_EDGE('',*,*,#9701,.T.);
#13208=ORIENTED_EDGE('',*,*,#9702,.T.);
#13209=ORIENTED_EDGE('',*,*,#9703,.T.);
#13210=ORIENTED_EDGE('',*,*,#9704,.T.);
#13211=ORIENTED_EDGE('',*,*,#9705,.T.);
#13212=ORIENTED_EDGE('',*,*,#9695,.F.);
#13213=ORIENTED_EDGE('',*,*,#9706,.F.);
#13214=ORIENTED_EDGE('',*,*,#9707,.T.);
#13215=ORIENTED_EDGE('',*,*,#9708,.T.);
#13216=ORIENTED_EDGE('',*,*,#9709,.T.);
#13217=ORIENTED_EDGE('',*,*,#9710,.T.);
#13218=ORIENTED_EDGE('',*,*,#9711,.T.);
#13219=ORIENTED_EDGE('',*,*,#9712,.T.);
#13220=ORIENTED_EDGE('',*,*,#9711,.F.);
#13221=ORIENTED_EDGE('',*,*,#9713,.T.);
#13222=ORIENTED_EDGE('',*,*,#9714,.T.);
#13223=ORIENTED_EDGE('',*,*,#9715,.T.);
#13224=ORIENTED_EDGE('',*,*,#9707,.F.);
#13225=ORIENTED_EDGE('',*,*,#9716,.F.);
#13226=ORIENTED_EDGE('',*,*,#9697,.F.);
#13227=ORIENTED_EDGE('',*,*,#9717,.T.);
#13228=ORIENTED_EDGE('',*,*,#9718,.T.);
#13229=ORIENTED_EDGE('',*,*,#9719,.T.);
#13230=ORIENTED_EDGE('',*,*,#9720,.T.);
#13231=ORIENTED_EDGE('',*,*,#9721,.T.);
#13232=ORIENTED_EDGE('',*,*,#9722,.T.);
#13233=ORIENTED_EDGE('',*,*,#9723,.T.);
#13234=ORIENTED_EDGE('',*,*,#9724,.T.);
#13235=ORIENTED_EDGE('',*,*,#9725,.T.);
#13236=ORIENTED_EDGE('',*,*,#9726,.T.);
#13237=ORIENTED_EDGE('',*,*,#9727,.T.);
#13238=ORIENTED_EDGE('',*,*,#9728,.T.);
#13239=ORIENTED_EDGE('',*,*,#9729,.T.);
#13240=ORIENTED_EDGE('',*,*,#9730,.T.);
#13241=ORIENTED_EDGE('',*,*,#9731,.T.);
#13242=ORIENTED_EDGE('',*,*,#9732,.T.);
#13243=ORIENTED_EDGE('',*,*,#9733,.T.);
#13244=ORIENTED_EDGE('',*,*,#9734,.T.);
#13245=ORIENTED_EDGE('',*,*,#9735,.T.);
#13246=ORIENTED_EDGE('',*,*,#9736,.T.);
#13247=ORIENTED_EDGE('',*,*,#9737,.T.);
#13248=ORIENTED_EDGE('',*,*,#9738,.T.);
#13249=ORIENTED_EDGE('',*,*,#9739,.T.);
#13250=ORIENTED_EDGE('',*,*,#9740,.T.);
#13251=ORIENTED_EDGE('',*,*,#9741,.T.);
#13252=ORIENTED_EDGE('',*,*,#9742,.T.);
#13253=ORIENTED_EDGE('',*,*,#9743,.T.);
#13254=ORIENTED_EDGE('',*,*,#9744,.T.);
#13255=ORIENTED_EDGE('',*,*,#9745,.T.);
#13256=ORIENTED_EDGE('',*,*,#9746,.T.);
#13257=ORIENTED_EDGE('',*,*,#9747,.T.);
#13258=ORIENTED_EDGE('',*,*,#9748,.T.);
#13259=ORIENTED_EDGE('',*,*,#9749,.T.);
#13260=ORIENTED_EDGE('',*,*,#9750,.T.);
#13261=ORIENTED_EDGE('',*,*,#9751,.T.);
#13262=ORIENTED_EDGE('',*,*,#9752,.T.);
#13263=ORIENTED_EDGE('',*,*,#9753,.T.);
#13264=ORIENTED_EDGE('',*,*,#9754,.T.);
#13265=ORIENTED_EDGE('',*,*,#9755,.T.);
#13266=ORIENTED_EDGE('',*,*,#9756,.T.);
#13267=ORIENTED_EDGE('',*,*,#9757,.T.);
#13268=ORIENTED_EDGE('',*,*,#9758,.T.);
#13269=ORIENTED_EDGE('',*,*,#9759,.T.);
#13270=ORIENTED_EDGE('',*,*,#9760,.T.);
#13271=ORIENTED_EDGE('',*,*,#9761,.T.);
#13272=ORIENTED_EDGE('',*,*,#9762,.T.);
#13273=ORIENTED_EDGE('',*,*,#9763,.T.);
#13274=ORIENTED_EDGE('',*,*,#9764,.T.);
#13275=ORIENTED_EDGE('',*,*,#9765,.T.);
#13276=ORIENTED_EDGE('',*,*,#9766,.T.);
#13277=ORIENTED_EDGE('',*,*,#9767,.T.);
#13278=ORIENTED_EDGE('',*,*,#9768,.T.);
#13279=ORIENTED_EDGE('',*,*,#9769,.T.);
#13280=ORIENTED_EDGE('',*,*,#9770,.T.);
#13281=ORIENTED_EDGE('',*,*,#9771,.T.);
#13282=ORIENTED_EDGE('',*,*,#9772,.T.);
#13283=ORIENTED_EDGE('',*,*,#9773,.T.);
#13284=ORIENTED_EDGE('',*,*,#9774,.T.);
#13285=ORIENTED_EDGE('',*,*,#9775,.T.);
#13286=ORIENTED_EDGE('',*,*,#9776,.T.);
#13287=ORIENTED_EDGE('',*,*,#9777,.T.);
#13288=ORIENTED_EDGE('',*,*,#9778,.T.);
#13289=ORIENTED_EDGE('',*,*,#9779,.T.);
#13290=ORIENTED_EDGE('',*,*,#9780,.T.);
#13291=ORIENTED_EDGE('',*,*,#9781,.T.);
#13292=ORIENTED_EDGE('',*,*,#9782,.T.);
#13293=ORIENTED_EDGE('',*,*,#9783,.T.);
#13294=ORIENTED_EDGE('',*,*,#9784,.T.);
#13295=ORIENTED_EDGE('',*,*,#9785,.T.);
#13296=ORIENTED_EDGE('',*,*,#9786,.T.);
#13297=ORIENTED_EDGE('',*,*,#9787,.T.);
#13298=ORIENTED_EDGE('',*,*,#9788,.T.);
#13299=ORIENTED_EDGE('',*,*,#9789,.T.);
#13300=ORIENTED_EDGE('',*,*,#9790,.T.);
#13301=ORIENTED_EDGE('',*,*,#9791,.T.);
#13302=ORIENTED_EDGE('',*,*,#9792,.T.);
#13303=ORIENTED_EDGE('',*,*,#9793,.T.);
#13304=ORIENTED_EDGE('',*,*,#9794,.T.);
#13305=ORIENTED_EDGE('',*,*,#9795,.T.);
#13306=ORIENTED_EDGE('',*,*,#9796,.T.);
#13307=ORIENTED_EDGE('',*,*,#9797,.T.);
#13308=ORIENTED_EDGE('',*,*,#9798,.T.);
#13309=ORIENTED_EDGE('',*,*,#9799,.T.);
#13310=ORIENTED_EDGE('',*,*,#9800,.T.);
#13311=ORIENTED_EDGE('',*,*,#9801,.T.);
#13312=ORIENTED_EDGE('',*,*,#9802,.T.);
#13313=ORIENTED_EDGE('',*,*,#9803,.T.);
#13314=ORIENTED_EDGE('',*,*,#9804,.T.);
#13315=ORIENTED_EDGE('',*,*,#9805,.T.);
#13316=ORIENTED_EDGE('',*,*,#9806,.T.);
#13317=ORIENTED_EDGE('',*,*,#9807,.T.);
#13318=ORIENTED_EDGE('',*,*,#9694,.F.);
#13319=ORIENTED_EDGE('',*,*,#9808,.F.);
#13320=ORIENTED_EDGE('',*,*,#9692,.F.);
#13321=ORIENTED_EDGE('',*,*,#9716,.T.);
#13322=ORIENTED_EDGE('',*,*,#9706,.T.);
#13323=ORIENTED_EDGE('',*,*,#9693,.F.);
#13324=ORIENTED_EDGE('',*,*,#9808,.T.);
#13325=ORIENTED_EDGE('',*,*,#9809,.F.);
#13326=ORIENTED_EDGE('',*,*,#9810,.F.);
#13327=ORIENTED_EDGE('',*,*,#9644,.F.);
#13328=ORIENTED_EDGE('',*,*,#9641,.F.);
#13329=ORIENTED_EDGE('',*,*,#9638,.F.);
#13330=ORIENTED_EDGE('',*,*,#9635,.F.);
#13331=ORIENTED_EDGE('',*,*,#9632,.F.);
#13332=ORIENTED_EDGE('',*,*,#9629,.F.);
#13333=ORIENTED_EDGE('',*,*,#9626,.F.);
#13334=ORIENTED_EDGE('',*,*,#9623,.F.);
#13335=ORIENTED_EDGE('',*,*,#9620,.F.);
#13336=ORIENTED_EDGE('',*,*,#9617,.F.);
#13337=ORIENTED_EDGE('',*,*,#9614,.F.);
#13338=ORIENTED_EDGE('',*,*,#9611,.F.);
#13339=ORIENTED_EDGE('',*,*,#9608,.F.);
#13340=ORIENTED_EDGE('',*,*,#9811,.F.);
#13341=ORIENTED_EDGE('',*,*,#9812,.T.);
#13342=ORIENTED_EDGE('',*,*,#9684,.T.);
#13343=ORIENTED_EDGE('',*,*,#9681,.T.);
#13344=ORIENTED_EDGE('',*,*,#9678,.T.);
#13345=ORIENTED_EDGE('',*,*,#9675,.T.);
#13346=ORIENTED_EDGE('',*,*,#9672,.T.);
#13347=ORIENTED_EDGE('',*,*,#9669,.T.);
#13348=ORIENTED_EDGE('',*,*,#9666,.T.);
#13349=ORIENTED_EDGE('',*,*,#9663,.T.);
#13350=ORIENTED_EDGE('',*,*,#9660,.T.);
#13351=ORIENTED_EDGE('',*,*,#9657,.T.);
#13352=ORIENTED_EDGE('',*,*,#9654,.T.);
#13353=ORIENTED_EDGE('',*,*,#9651,.T.);
#13354=ORIENTED_EDGE('',*,*,#9813,.T.);
#13355=ORIENTED_EDGE('',*,*,#9814,.T.);
#13356=ORIENTED_EDGE('',*,*,#9815,.T.);
#13357=ORIENTED_EDGE('',*,*,#9816,.T.);
#13358=ORIENTED_EDGE('',*,*,#9811,.T.);
#13359=ORIENTED_EDGE('',*,*,#9682,.T.);
#13360=ORIENTED_EDGE('',*,*,#9812,.F.);
#13361=ORIENTED_EDGE('',*,*,#9816,.F.);
#13362=ORIENTED_EDGE('',*,*,#9817,.T.);
#13363=ORIENTED_EDGE('',*,*,#9818,.F.);
#13364=ORIENTED_EDGE('',*,*,#9646,.F.);
#13365=ORIENTED_EDGE('',*,*,#9649,.F.);
#13366=ORIENTED_EDGE('',*,*,#9653,.F.);
#13367=ORIENTED_EDGE('',*,*,#9656,.F.);
#13368=ORIENTED_EDGE('',*,*,#9659,.F.);
#13369=ORIENTED_EDGE('',*,*,#9662,.F.);
#13370=ORIENTED_EDGE('',*,*,#9665,.F.);
#13371=ORIENTED_EDGE('',*,*,#9668,.F.);
#13372=ORIENTED_EDGE('',*,*,#9671,.F.);
#13373=ORIENTED_EDGE('',*,*,#9674,.F.);
#13374=ORIENTED_EDGE('',*,*,#9677,.F.);
#13375=ORIENTED_EDGE('',*,*,#9680,.F.);
#13376=ORIENTED_EDGE('',*,*,#9683,.F.);
#13377=ORIENTED_EDGE('',*,*,#9817,.F.);
#13378=ORIENTED_EDGE('',*,*,#9815,.F.);
#13379=ORIENTED_EDGE('',*,*,#9606,.F.);
#13380=ORIENTED_EDGE('',*,*,#9610,.F.);
#13381=ORIENTED_EDGE('',*,*,#9613,.F.);
#13382=ORIENTED_EDGE('',*,*,#9616,.F.);
#13383=ORIENTED_EDGE('',*,*,#9619,.F.);
#13384=ORIENTED_EDGE('',*,*,#9622,.F.);
#13385=ORIENTED_EDGE('',*,*,#9625,.F.);
#13386=ORIENTED_EDGE('',*,*,#9628,.F.);
#13387=ORIENTED_EDGE('',*,*,#9631,.F.);
#13388=ORIENTED_EDGE('',*,*,#9634,.F.);
#13389=ORIENTED_EDGE('',*,*,#9637,.F.);
#13390=ORIENTED_EDGE('',*,*,#9640,.F.);
#13391=ORIENTED_EDGE('',*,*,#9643,.F.);
#13392=ORIENTED_EDGE('',*,*,#9819,.F.);
#13393=ORIENTED_EDGE('',*,*,#9696,.F.);
#13394=ORIENTED_EDGE('',*,*,#9705,.F.);
#13395=ORIENTED_EDGE('',*,*,#9820,.T.);
#13396=ORIENTED_EDGE('',*,*,#9717,.F.);
#13397=ORIENTED_EDGE('',*,*,#9700,.F.);
#13398=ORIENTED_EDGE('',*,*,#9821,.F.);
#13399=ORIENTED_EDGE('',*,*,#9722,.F.);
#13400=ORIENTED_EDGE('',*,*,#9822,.F.);
#13401=ORIENTED_EDGE('',*,*,#9823,.F.);
#13402=ORIENTED_EDGE('',*,*,#9718,.F.);
#13403=ORIENTED_EDGE('',*,*,#9820,.F.);
#13404=ORIENTED_EDGE('',*,*,#9704,.F.);
#13405=ORIENTED_EDGE('',*,*,#9824,.F.);
#13406=ORIENTED_EDGE('',*,*,#9825,.F.);
#13407=ORIENTED_EDGE('',*,*,#9689,.F.);
#13408=ORIENTED_EDGE('',*,*,#9723,.F.);
#13409=ORIENTED_EDGE('',*,*,#9821,.T.);
#13410=ORIENTED_EDGE('',*,*,#9699,.F.);
#13411=ORIENTED_EDGE('',*,*,#9824,.T.);
#13412=ORIENTED_EDGE('',*,*,#9703,.F.);
#13413=ORIENTED_EDGE('',*,*,#9826,.F.);
#13414=ORIENTED_EDGE('',*,*,#9827,.T.);
#13415=ORIENTED_EDGE('',*,*,#9806,.F.);
#13416=ORIENTED_EDGE('',*,*,#9828,.T.);
#13417=ORIENTED_EDGE('',*,*,#9829,.F.);
#13418=ORIENTED_EDGE('',*,*,#9830,.F.);
#13419=ORIENTED_EDGE('',*,*,#9807,.F.);
#13420=ORIENTED_EDGE('',*,*,#9830,.T.);
#13421=ORIENTED_EDGE('',*,*,#9831,.T.);
#13422=ORIENTED_EDGE('',*,*,#9804,.F.);
#13423=ORIENTED_EDGE('',*,*,#9831,.F.);
#13424=ORIENTED_EDGE('',*,*,#9829,.T.);
#13425=ORIENTED_EDGE('',*,*,#9832,.T.);
#13426=ORIENTED_EDGE('',*,*,#9805,.F.);
#13427=ORIENTED_EDGE('',*,*,#9832,.F.);
#13428=ORIENTED_EDGE('',*,*,#9828,.F.);
#13429=ORIENTED_EDGE('',*,*,#9802,.F.);
#13430=ORIENTED_EDGE('',*,*,#9833,.T.);
#13431=ORIENTED_EDGE('',*,*,#9834,.F.);
#13432=ORIENTED_EDGE('',*,*,#9835,.F.);
#13433=ORIENTED_EDGE('',*,*,#9803,.F.);
#13434=ORIENTED_EDGE('',*,*,#9835,.T.);
#13435=ORIENTED_EDGE('',*,*,#9836,.T.);
#13436=ORIENTED_EDGE('',*,*,#9800,.F.);
#13437=ORIENTED_EDGE('',*,*,#9836,.F.);
#13438=ORIENTED_EDGE('',*,*,#9834,.T.);
#13439=ORIENTED_EDGE('',*,*,#9837,.T.);
#13440=ORIENTED_EDGE('',*,*,#9801,.F.);
#13441=ORIENTED_EDGE('',*,*,#9837,.F.);
#13442=ORIENTED_EDGE('',*,*,#9833,.F.);
#13443=ORIENTED_EDGE('',*,*,#9798,.F.);
#13444=ORIENTED_EDGE('',*,*,#9838,.T.);
#13445=ORIENTED_EDGE('',*,*,#9839,.F.);
#13446=ORIENTED_EDGE('',*,*,#9840,.F.);
#13447=ORIENTED_EDGE('',*,*,#9799,.F.);
#13448=ORIENTED_EDGE('',*,*,#9840,.T.);
#13449=ORIENTED_EDGE('',*,*,#9841,.T.);
#13450=ORIENTED_EDGE('',*,*,#9796,.F.);
#13451=ORIENTED_EDGE('',*,*,#9841,.F.);
#13452=ORIENTED_EDGE('',*,*,#9839,.T.);
#13453=ORIENTED_EDGE('',*,*,#9842,.T.);
#13454=ORIENTED_EDGE('',*,*,#9797,.F.);
#13455=ORIENTED_EDGE('',*,*,#9842,.F.);
#13456=ORIENTED_EDGE('',*,*,#9838,.F.);
#13457=ORIENTED_EDGE('',*,*,#9794,.F.);
#13458=ORIENTED_EDGE('',*,*,#9843,.T.);
#13459=ORIENTED_EDGE('',*,*,#9844,.F.);
#13460=ORIENTED_EDGE('',*,*,#9845,.F.);
#13461=ORIENTED_EDGE('',*,*,#9795,.F.);
#13462=ORIENTED_EDGE('',*,*,#9845,.T.);
#13463=ORIENTED_EDGE('',*,*,#9846,.T.);
#13464=ORIENTED_EDGE('',*,*,#9792,.F.);
#13465=ORIENTED_EDGE('',*,*,#9846,.F.);
#13466=ORIENTED_EDGE('',*,*,#9844,.T.);
#13467=ORIENTED_EDGE('',*,*,#9847,.T.);
#13468=ORIENTED_EDGE('',*,*,#9793,.F.);
#13469=ORIENTED_EDGE('',*,*,#9847,.F.);
#13470=ORIENTED_EDGE('',*,*,#9843,.F.);
#13471=ORIENTED_EDGE('',*,*,#9790,.F.);
#13472=ORIENTED_EDGE('',*,*,#9848,.T.);
#13473=ORIENTED_EDGE('',*,*,#9849,.F.);
#13474=ORIENTED_EDGE('',*,*,#9850,.F.);
#13475=ORIENTED_EDGE('',*,*,#9791,.F.);
#13476=ORIENTED_EDGE('',*,*,#9850,.T.);
#13477=ORIENTED_EDGE('',*,*,#9851,.T.);
#13478=ORIENTED_EDGE('',*,*,#9788,.F.);
#13479=ORIENTED_EDGE('',*,*,#9851,.F.);
#13480=ORIENTED_EDGE('',*,*,#9849,.T.);
#13481=ORIENTED_EDGE('',*,*,#9852,.T.);
#13482=ORIENTED_EDGE('',*,*,#9789,.F.);
#13483=ORIENTED_EDGE('',*,*,#9852,.F.);
#13484=ORIENTED_EDGE('',*,*,#9848,.F.);
#13485=ORIENTED_EDGE('',*,*,#9825,.T.);
#13486=ORIENTED_EDGE('',*,*,#9827,.F.);
#13487=ORIENTED_EDGE('',*,*,#9853,.F.);
#13488=ORIENTED_EDGE('',*,*,#9701,.F.);
#13489=ORIENTED_EDGE('',*,*,#9702,.F.);
#13490=ORIENTED_EDGE('',*,*,#9853,.T.);
#13491=ORIENTED_EDGE('',*,*,#9826,.T.);
#13492=ORIENTED_EDGE('',*,*,#9786,.F.);
#13493=ORIENTED_EDGE('',*,*,#9854,.T.);
#13494=ORIENTED_EDGE('',*,*,#9855,.F.);
#13495=ORIENTED_EDGE('',*,*,#9856,.F.);
#13496=ORIENTED_EDGE('',*,*,#9787,.F.);
#13497=ORIENTED_EDGE('',*,*,#9856,.T.);
#13498=ORIENTED_EDGE('',*,*,#9857,.T.);
#13499=ORIENTED_EDGE('',*,*,#9784,.F.);
#13500=ORIENTED_EDGE('',*,*,#9857,.F.);
#13501=ORIENTED_EDGE('',*,*,#9855,.T.);
#13502=ORIENTED_EDGE('',*,*,#9858,.T.);
#13503=ORIENTED_EDGE('',*,*,#9785,.F.);
#13504=ORIENTED_EDGE('',*,*,#9858,.F.);
#13505=ORIENTED_EDGE('',*,*,#9854,.F.);
#13506=ORIENTED_EDGE('',*,*,#9782,.F.);
#13507=ORIENTED_EDGE('',*,*,#9859,.T.);
#13508=ORIENTED_EDGE('',*,*,#9860,.F.);
#13509=ORIENTED_EDGE('',*,*,#9861,.F.);
#13510=ORIENTED_EDGE('',*,*,#9783,.F.);
#13511=ORIENTED_EDGE('',*,*,#9861,.T.);
#13512=ORIENTED_EDGE('',*,*,#9862,.T.);
#13513=ORIENTED_EDGE('',*,*,#9780,.F.);
#13514=ORIENTED_EDGE('',*,*,#9862,.F.);
#13515=ORIENTED_EDGE('',*,*,#9860,.T.);
#13516=ORIENTED_EDGE('',*,*,#9863,.T.);
#13517=ORIENTED_EDGE('',*,*,#9781,.F.);
#13518=ORIENTED_EDGE('',*,*,#9863,.F.);
#13519=ORIENTED_EDGE('',*,*,#9859,.F.);
#13520=ORIENTED_EDGE('',*,*,#9778,.F.);
#13521=ORIENTED_EDGE('',*,*,#9864,.T.);
#13522=ORIENTED_EDGE('',*,*,#9865,.F.);
#13523=ORIENTED_EDGE('',*,*,#9866,.F.);
#13524=ORIENTED_EDGE('',*,*,#9779,.F.);
#13525=ORIENTED_EDGE('',*,*,#9866,.T.);
#13526=ORIENTED_EDGE('',*,*,#9867,.T.);
#13527=ORIENTED_EDGE('',*,*,#9776,.F.);
#13528=ORIENTED_EDGE('',*,*,#9867,.F.);
#13529=ORIENTED_EDGE('',*,*,#9865,.T.);
#13530=ORIENTED_EDGE('',*,*,#9868,.T.);
#13531=ORIENTED_EDGE('',*,*,#9777,.F.);
#13532=ORIENTED_EDGE('',*,*,#9868,.F.);
#13533=ORIENTED_EDGE('',*,*,#9864,.F.);
#13534=ORIENTED_EDGE('',*,*,#9774,.F.);
#13535=ORIENTED_EDGE('',*,*,#9869,.T.);
#13536=ORIENTED_EDGE('',*,*,#9870,.F.);
#13537=ORIENTED_EDGE('',*,*,#9871,.F.);
#13538=ORIENTED_EDGE('',*,*,#9775,.F.);
#13539=ORIENTED_EDGE('',*,*,#9871,.T.);
#13540=ORIENTED_EDGE('',*,*,#9872,.T.);
#13541=ORIENTED_EDGE('',*,*,#9772,.F.);
#13542=ORIENTED_EDGE('',*,*,#9872,.F.);
#13543=ORIENTED_EDGE('',*,*,#9870,.T.);
#13544=ORIENTED_EDGE('',*,*,#9873,.T.);
#13545=ORIENTED_EDGE('',*,*,#9773,.F.);
#13546=ORIENTED_EDGE('',*,*,#9873,.F.);
#13547=ORIENTED_EDGE('',*,*,#9869,.F.);
#13548=ORIENTED_EDGE('',*,*,#9770,.F.);
#13549=ORIENTED_EDGE('',*,*,#9874,.T.);
#13550=ORIENTED_EDGE('',*,*,#9875,.F.);
#13551=ORIENTED_EDGE('',*,*,#9876,.F.);
#13552=ORIENTED_EDGE('',*,*,#9771,.F.);
#13553=ORIENTED_EDGE('',*,*,#9876,.T.);
#13554=ORIENTED_EDGE('',*,*,#9877,.T.);
#13555=ORIENTED_EDGE('',*,*,#9768,.F.);
#13556=ORIENTED_EDGE('',*,*,#9877,.F.);
#13557=ORIENTED_EDGE('',*,*,#9875,.T.);
#13558=ORIENTED_EDGE('',*,*,#9878,.T.);
#13559=ORIENTED_EDGE('',*,*,#9769,.F.);
#13560=ORIENTED_EDGE('',*,*,#9878,.F.);
#13561=ORIENTED_EDGE('',*,*,#9874,.F.);
#13562=ORIENTED_EDGE('',*,*,#9709,.F.);
#13563=ORIENTED_EDGE('',*,*,#9879,.T.);
#13564=ORIENTED_EDGE('',*,*,#9880,.F.);
#13565=ORIENTED_EDGE('',*,*,#9881,.F.);
#13566=ORIENTED_EDGE('',*,*,#9710,.F.);
#13567=ORIENTED_EDGE('',*,*,#9881,.T.);
#13568=ORIENTED_EDGE('',*,*,#9882,.T.);
#13569=ORIENTED_EDGE('',*,*,#9713,.F.);
#13570=ORIENTED_EDGE('',*,*,#9714,.F.);
#13571=ORIENTED_EDGE('',*,*,#9882,.F.);
#13572=ORIENTED_EDGE('',*,*,#9880,.T.);
#13573=ORIENTED_EDGE('',*,*,#9883,.T.);
#13574=ORIENTED_EDGE('',*,*,#9715,.F.);
#13575=ORIENTED_EDGE('',*,*,#9883,.F.);
#13576=ORIENTED_EDGE('',*,*,#9879,.F.);
#13577=ORIENTED_EDGE('',*,*,#9708,.F.);
#13578=ORIENTED_EDGE('',*,*,#9766,.F.);
#13579=ORIENTED_EDGE('',*,*,#9884,.T.);
#13580=ORIENTED_EDGE('',*,*,#9885,.F.);
#13581=ORIENTED_EDGE('',*,*,#9886,.F.);
#13582=ORIENTED_EDGE('',*,*,#9767,.F.);
#13583=ORIENTED_EDGE('',*,*,#9886,.T.);
#13584=ORIENTED_EDGE('',*,*,#9887,.T.);
#13585=ORIENTED_EDGE('',*,*,#9764,.F.);
#13586=ORIENTED_EDGE('',*,*,#9887,.F.);
#13587=ORIENTED_EDGE('',*,*,#9885,.T.);
#13588=ORIENTED_EDGE('',*,*,#9888,.T.);
#13589=ORIENTED_EDGE('',*,*,#9765,.F.);
#13590=ORIENTED_EDGE('',*,*,#9888,.F.);
#13591=ORIENTED_EDGE('',*,*,#9884,.F.);
#13592=ORIENTED_EDGE('',*,*,#9762,.F.);
#13593=ORIENTED_EDGE('',*,*,#9889,.T.);
#13594=ORIENTED_EDGE('',*,*,#9890,.F.);
#13595=ORIENTED_EDGE('',*,*,#9891,.F.);
#13596=ORIENTED_EDGE('',*,*,#9763,.F.);
#13597=ORIENTED_EDGE('',*,*,#9891,.T.);
#13598=ORIENTED_EDGE('',*,*,#9892,.T.);
#13599=ORIENTED_EDGE('',*,*,#9760,.F.);
#13600=ORIENTED_EDGE('',*,*,#9892,.F.);
#13601=ORIENTED_EDGE('',*,*,#9890,.T.);
#13602=ORIENTED_EDGE('',*,*,#9893,.T.);
#13603=ORIENTED_EDGE('',*,*,#9761,.F.);
#13604=ORIENTED_EDGE('',*,*,#9893,.F.);
#13605=ORIENTED_EDGE('',*,*,#9889,.F.);
#13606=ORIENTED_EDGE('',*,*,#9758,.F.);
#13607=ORIENTED_EDGE('',*,*,#9894,.T.);
#13608=ORIENTED_EDGE('',*,*,#9895,.F.);
#13609=ORIENTED_EDGE('',*,*,#9896,.F.);
#13610=ORIENTED_EDGE('',*,*,#9759,.F.);
#13611=ORIENTED_EDGE('',*,*,#9896,.T.);
#13612=ORIENTED_EDGE('',*,*,#9897,.T.);
#13613=ORIENTED_EDGE('',*,*,#9756,.F.);
#13614=ORIENTED_EDGE('',*,*,#9897,.F.);
#13615=ORIENTED_EDGE('',*,*,#9895,.T.);
#13616=ORIENTED_EDGE('',*,*,#9898,.T.);
#13617=ORIENTED_EDGE('',*,*,#9757,.F.);
#13618=ORIENTED_EDGE('',*,*,#9898,.F.);
#13619=ORIENTED_EDGE('',*,*,#9894,.F.);
#13620=ORIENTED_EDGE('',*,*,#9754,.F.);
#13621=ORIENTED_EDGE('',*,*,#9899,.T.);
#13622=ORIENTED_EDGE('',*,*,#9900,.F.);
#13623=ORIENTED_EDGE('',*,*,#9901,.F.);
#13624=ORIENTED_EDGE('',*,*,#9755,.F.);
#13625=ORIENTED_EDGE('',*,*,#9901,.T.);
#13626=ORIENTED_EDGE('',*,*,#9902,.T.);
#13627=ORIENTED_EDGE('',*,*,#9752,.F.);
#13628=ORIENTED_EDGE('',*,*,#9902,.F.);
#13629=ORIENTED_EDGE('',*,*,#9900,.T.);
#13630=ORIENTED_EDGE('',*,*,#9903,.T.);
#13631=ORIENTED_EDGE('',*,*,#9753,.F.);
#13632=ORIENTED_EDGE('',*,*,#9903,.F.);
#13633=ORIENTED_EDGE('',*,*,#9899,.F.);
#13634=ORIENTED_EDGE('',*,*,#9750,.F.);
#13635=ORIENTED_EDGE('',*,*,#9904,.T.);
#13636=ORIENTED_EDGE('',*,*,#9905,.F.);
#13637=ORIENTED_EDGE('',*,*,#9906,.F.);
#13638=ORIENTED_EDGE('',*,*,#9751,.F.);
#13639=ORIENTED_EDGE('',*,*,#9906,.T.);
#13640=ORIENTED_EDGE('',*,*,#9907,.T.);
#13641=ORIENTED_EDGE('',*,*,#9748,.F.);
#13642=ORIENTED_EDGE('',*,*,#9907,.F.);
#13643=ORIENTED_EDGE('',*,*,#9905,.T.);
#13644=ORIENTED_EDGE('',*,*,#9908,.T.);
#13645=ORIENTED_EDGE('',*,*,#9749,.F.);
#13646=ORIENTED_EDGE('',*,*,#9908,.F.);
#13647=ORIENTED_EDGE('',*,*,#9904,.F.);
#13648=ORIENTED_EDGE('',*,*,#9823,.T.);
#13649=ORIENTED_EDGE('',*,*,#9909,.F.);
#13650=ORIENTED_EDGE('',*,*,#9910,.F.);
#13651=ORIENTED_EDGE('',*,*,#9719,.F.);
#13652=ORIENTED_EDGE('',*,*,#9720,.F.);
#13653=ORIENTED_EDGE('',*,*,#9910,.T.);
#13654=ORIENTED_EDGE('',*,*,#9911,.T.);
#13655=ORIENTED_EDGE('',*,*,#9822,.T.);
#13656=ORIENTED_EDGE('',*,*,#9721,.F.);
#13657=ORIENTED_EDGE('',*,*,#9911,.F.);
#13658=ORIENTED_EDGE('',*,*,#9909,.T.);
#13659=ORIENTED_EDGE('',*,*,#9746,.F.);
#13660=ORIENTED_EDGE('',*,*,#9912,.T.);
#13661=ORIENTED_EDGE('',*,*,#9913,.F.);
#13662=ORIENTED_EDGE('',*,*,#9914,.F.);
#13663=ORIENTED_EDGE('',*,*,#9747,.F.);
#13664=ORIENTED_EDGE('',*,*,#9914,.T.);
#13665=ORIENTED_EDGE('',*,*,#9915,.T.);
#13666=ORIENTED_EDGE('',*,*,#9744,.F.);
#13667=ORIENTED_EDGE('',*,*,#9915,.F.);
#13668=ORIENTED_EDGE('',*,*,#9913,.T.);
#13669=ORIENTED_EDGE('',*,*,#9916,.T.);
#13670=ORIENTED_EDGE('',*,*,#9745,.F.);
#13671=ORIENTED_EDGE('',*,*,#9916,.F.);
#13672=ORIENTED_EDGE('',*,*,#9912,.F.);
#13673=ORIENTED_EDGE('',*,*,#9742,.F.);
#13674=ORIENTED_EDGE('',*,*,#9917,.T.);
#13675=ORIENTED_EDGE('',*,*,#9918,.F.);
#13676=ORIENTED_EDGE('',*,*,#9919,.F.);
#13677=ORIENTED_EDGE('',*,*,#9743,.F.);
#13678=ORIENTED_EDGE('',*,*,#9919,.T.);
#13679=ORIENTED_EDGE('',*,*,#9920,.T.);
#13680=ORIENTED_EDGE('',*,*,#9740,.F.);
#13681=ORIENTED_EDGE('',*,*,#9920,.F.);
#13682=ORIENTED_EDGE('',*,*,#9918,.T.);
#13683=ORIENTED_EDGE('',*,*,#9921,.T.);
#13684=ORIENTED_EDGE('',*,*,#9741,.F.);
#13685=ORIENTED_EDGE('',*,*,#9921,.F.);
#13686=ORIENTED_EDGE('',*,*,#9917,.F.);
#13687=ORIENTED_EDGE('',*,*,#9738,.F.);
#13688=ORIENTED_EDGE('',*,*,#9922,.T.);
#13689=ORIENTED_EDGE('',*,*,#9923,.F.);
#13690=ORIENTED_EDGE('',*,*,#9924,.F.);
#13691=ORIENTED_EDGE('',*,*,#9739,.F.);
#13692=ORIENTED_EDGE('',*,*,#9924,.T.);
#13693=ORIENTED_EDGE('',*,*,#9925,.T.);
#13694=ORIENTED_EDGE('',*,*,#9736,.F.);
#13695=ORIENTED_EDGE('',*,*,#9925,.F.);
#13696=ORIENTED_EDGE('',*,*,#9923,.T.);
#13697=ORIENTED_EDGE('',*,*,#9926,.T.);
#13698=ORIENTED_EDGE('',*,*,#9737,.F.);
#13699=ORIENTED_EDGE('',*,*,#9926,.F.);
#13700=ORIENTED_EDGE('',*,*,#9922,.F.);
#13701=ORIENTED_EDGE('',*,*,#9734,.F.);
#13702=ORIENTED_EDGE('',*,*,#9927,.T.);
#13703=ORIENTED_EDGE('',*,*,#9928,.F.);
#13704=ORIENTED_EDGE('',*,*,#9929,.F.);
#13705=ORIENTED_EDGE('',*,*,#9735,.F.);
#13706=ORIENTED_EDGE('',*,*,#9929,.T.);
#13707=ORIENTED_EDGE('',*,*,#9930,.T.);
#13708=ORIENTED_EDGE('',*,*,#9732,.F.);
#13709=ORIENTED_EDGE('',*,*,#9930,.F.);
#13710=ORIENTED_EDGE('',*,*,#9928,.T.);
#13711=ORIENTED_EDGE('',*,*,#9931,.T.);
#13712=ORIENTED_EDGE('',*,*,#9733,.F.);
#13713=ORIENTED_EDGE('',*,*,#9931,.F.);
#13714=ORIENTED_EDGE('',*,*,#9927,.F.);
#13715=ORIENTED_EDGE('',*,*,#9730,.F.);
#13716=ORIENTED_EDGE('',*,*,#9932,.T.);
#13717=ORIENTED_EDGE('',*,*,#9933,.F.);
#13718=ORIENTED_EDGE('',*,*,#9934,.F.);
#13719=ORIENTED_EDGE('',*,*,#9731,.F.);
#13720=ORIENTED_EDGE('',*,*,#9934,.T.);
#13721=ORIENTED_EDGE('',*,*,#9935,.T.);
#13722=ORIENTED_EDGE('',*,*,#9728,.F.);
#13723=ORIENTED_EDGE('',*,*,#9935,.F.);
#13724=ORIENTED_EDGE('',*,*,#9933,.T.);
#13725=ORIENTED_EDGE('',*,*,#9936,.T.);
#13726=ORIENTED_EDGE('',*,*,#9729,.F.);
#13727=ORIENTED_EDGE('',*,*,#9936,.F.);
#13728=ORIENTED_EDGE('',*,*,#9932,.F.);
#13729=ORIENTED_EDGE('',*,*,#9726,.F.);
#13730=ORIENTED_EDGE('',*,*,#9937,.T.);
#13731=ORIENTED_EDGE('',*,*,#9938,.F.);
#13732=ORIENTED_EDGE('',*,*,#9939,.F.);
#13733=ORIENTED_EDGE('',*,*,#9727,.F.);
#13734=ORIENTED_EDGE('',*,*,#9939,.T.);
#13735=ORIENTED_EDGE('',*,*,#9940,.T.);
#13736=ORIENTED_EDGE('',*,*,#9724,.F.);
#13737=ORIENTED_EDGE('',*,*,#9940,.F.);
#13738=ORIENTED_EDGE('',*,*,#9938,.T.);
#13739=ORIENTED_EDGE('',*,*,#9941,.T.);
#13740=ORIENTED_EDGE('',*,*,#9725,.F.);
#13741=ORIENTED_EDGE('',*,*,#9941,.F.);
#13742=ORIENTED_EDGE('',*,*,#9937,.F.);
#13743=ORIENTED_EDGE('',*,*,#9942,.F.);
#13744=ORIENTED_EDGE('',*,*,#9813,.F.);
#13745=ORIENTED_EDGE('',*,*,#9607,.F.);
#13746=ORIENTED_EDGE('',*,*,#9814,.F.);
#13747=ORIENTED_EDGE('',*,*,#9943,.T.);
#13748=ORIENTED_EDGE('',*,*,#9942,.T.);
#13749=ORIENTED_EDGE('',*,*,#9943,.F.);
#13750=ORIENTED_EDGE('',*,*,#9642,.T.);
#13751=ORIENTED_EDGE('',*,*,#9810,.T.);
#13752=ORIENTED_EDGE('',*,*,#9944,.F.);
#13753=ORIENTED_EDGE('',*,*,#9819,.T.);
#13754=ORIENTED_EDGE('',*,*,#9945,.F.);
#13755=ORIENTED_EDGE('',*,*,#9944,.T.);
#13756=ORIENTED_EDGE('',*,*,#9809,.T.);
#13757=ORIENTED_EDGE('',*,*,#9650,.T.);
#13758=ORIENTED_EDGE('',*,*,#9647,.T.);
#13759=ORIENTED_EDGE('',*,*,#9818,.T.);
#13760=ORIENTED_EDGE('',*,*,#9712,.F.);
#13761=ORIENTED_EDGE('',*,*,#9946,.T.);
#13762=ORIENTED_EDGE('',*,*,#9945,.T.);
#13763=ORIENTED_EDGE('',*,*,#9946,.F.);
#13764=ORIENTED_EDGE('',*,*,#9687,.F.);
#13765=ORIENTED_EDGE('',*,*,#9691,.F.);
#13766=ORIENTED_EDGE('',*,*,#9685,.F.);
#13767=ORIENTED_EDGE('',*,*,#9698,.T.);
#13768=ORIENTED_EDGE('',*,*,#9947,.T.);
#13769=ORIENTED_EDGE('',*,*,#9948,.T.);
#13770=ORIENTED_EDGE('',*,*,#9949,.T.);
#13771=ORIENTED_EDGE('',*,*,#9950,.T.);
#13772=ORIENTED_EDGE('',*,*,#9948,.F.);
#13773=ORIENTED_EDGE('',*,*,#9951,.T.);
#13774=ORIENTED_EDGE('',*,*,#9952,.T.);
#13775=ORIENTED_EDGE('',*,*,#9949,.F.);
#13776=ORIENTED_EDGE('',*,*,#9950,.F.);
#13777=ORIENTED_EDGE('',*,*,#9952,.F.);
#13778=ORIENTED_EDGE('',*,*,#9953,.F.);
#13779=ORIENTED_EDGE('',*,*,#9947,.F.);
#13780=ORIENTED_EDGE('',*,*,#9953,.T.);
#13781=ORIENTED_EDGE('',*,*,#9954,.T.);
#13782=ORIENTED_EDGE('',*,*,#9955,.F.);
#13783=ORIENTED_EDGE('',*,*,#9954,.F.);
#13784=ORIENTED_EDGE('',*,*,#9956,.F.);
#13785=ORIENTED_EDGE('',*,*,#9955,.T.);
#13786=ORIENTED_EDGE('',*,*,#9957,.F.);
#13787=ORIENTED_EDGE('',*,*,#9958,.T.);
#13788=ORIENTED_EDGE('',*,*,#9956,.T.);
#13789=ORIENTED_EDGE('',*,*,#9958,.F.);
#13790=ORIENTED_EDGE('',*,*,#9959,.F.);
#13791=ORIENTED_EDGE('',*,*,#9960,.T.);
#13792=ORIENTED_EDGE('',*,*,#9957,.T.);
#13793=ORIENTED_EDGE('',*,*,#9960,.F.);
#13794=ORIENTED_EDGE('',*,*,#9961,.F.);
#13795=ORIENTED_EDGE('',*,*,#9962,.T.);
#13796=ORIENTED_EDGE('',*,*,#9959,.T.);
#13797=ORIENTED_EDGE('',*,*,#9962,.F.);
#13798=ORIENTED_EDGE('',*,*,#9961,.T.);
#13799=ORIENTED_EDGE('',*,*,#9951,.F.);
#13800=ORIENTED_EDGE('',*,*,#9963,.T.);
#13801=ORIENTED_EDGE('',*,*,#9964,.T.);
#13802=ORIENTED_EDGE('',*,*,#9965,.T.);
#13803=ORIENTED_EDGE('',*,*,#9966,.T.);
#13804=ORIENTED_EDGE('',*,*,#9964,.F.);
#13805=ORIENTED_EDGE('',*,*,#9965,.F.);
#13806=ORIENTED_EDGE('',*,*,#9966,.F.);
#13807=ORIENTED_EDGE('',*,*,#9967,.T.);
#13808=ORIENTED_EDGE('',*,*,#9968,.F.);
#13809=ORIENTED_EDGE('',*,*,#9969,.F.);
#13810=ORIENTED_EDGE('',*,*,#9967,.F.);
#13811=ORIENTED_EDGE('',*,*,#9963,.F.);
#13812=ORIENTED_EDGE('',*,*,#9968,.T.);
#13813=ORIENTED_EDGE('',*,*,#9969,.T.);
#13814=ORIENTED_EDGE('',*,*,#9970,.T.);
#13815=ORIENTED_EDGE('',*,*,#9971,.T.);
#13816=ORIENTED_EDGE('',*,*,#9972,.T.);
#13817=ORIENTED_EDGE('',*,*,#9970,.F.);
#13818=ORIENTED_EDGE('',*,*,#9971,.F.);
#13819=ORIENTED_EDGE('',*,*,#9972,.F.);
#13820=ORIENTED_EDGE('',*,*,#9973,.T.);
#13821=ORIENTED_EDGE('',*,*,#9974,.F.);
#13822=ORIENTED_EDGE('',*,*,#9975,.F.);
#13823=ORIENTED_EDGE('',*,*,#9973,.F.);
#13824=ORIENTED_EDGE('',*,*,#9974,.T.);
#13825=ORIENTED_EDGE('',*,*,#9975,.T.);
#13826=ORIENTED_EDGE('',*,*,#9976,.T.);
#13827=ORIENTED_EDGE('',*,*,#9977,.T.);
#13828=ORIENTED_EDGE('',*,*,#9978,.T.);
#13829=ORIENTED_EDGE('',*,*,#9976,.F.);
#13830=ORIENTED_EDGE('',*,*,#9977,.F.);
#13831=ORIENTED_EDGE('',*,*,#9978,.F.);
#13832=ORIENTED_EDGE('',*,*,#9979,.T.);
#13833=ORIENTED_EDGE('',*,*,#9980,.T.);
#13834=ORIENTED_EDGE('',*,*,#9979,.F.);
#13835=ORIENTED_EDGE('',*,*,#9981,.T.);
#13836=ORIENTED_EDGE('',*,*,#9982,.T.);
#13837=ORIENTED_EDGE('',*,*,#9983,.F.);
#13838=ORIENTED_EDGE('',*,*,#9982,.F.);
#13839=ORIENTED_EDGE('',*,*,#9984,.F.);
#13840=ORIENTED_EDGE('',*,*,#9983,.T.);
#13841=ORIENTED_EDGE('',*,*,#9980,.F.);
#13842=ORIENTED_EDGE('',*,*,#9985,.T.);
#13843=ORIENTED_EDGE('',*,*,#9984,.T.);
#13844=ORIENTED_EDGE('',*,*,#9985,.F.);
#13845=ORIENTED_EDGE('',*,*,#9986,.F.);
#13846=ORIENTED_EDGE('',*,*,#9986,.T.);
#13847=ORIENTED_EDGE('',*,*,#9987,.T.);
#13848=ORIENTED_EDGE('',*,*,#9981,.F.);
#13849=ORIENTED_EDGE('',*,*,#9987,.F.);
#13850=ORIENTED_EDGE('',*,*,#9988,.F.);
#13851=ORIENTED_EDGE('',*,*,#9989,.T.);
#13852=ORIENTED_EDGE('',*,*,#9990,.T.);
#13853=ORIENTED_EDGE('',*,*,#9991,.T.);
#13854=ORIENTED_EDGE('',*,*,#9992,.F.);
#13855=ORIENTED_EDGE('',*,*,#9993,.T.);
#13856=ORIENTED_EDGE('',*,*,#9988,.T.);
#13857=ORIENTED_EDGE('',*,*,#9994,.T.);
#13858=ORIENTED_EDGE('',*,*,#9995,.F.);
#13859=ORIENTED_EDGE('',*,*,#9996,.T.);
#13860=ORIENTED_EDGE('',*,*,#9992,.T.);
#13861=ORIENTED_EDGE('',*,*,#9997,.T.);
#13862=ORIENTED_EDGE('',*,*,#9998,.F.);
#13863=ORIENTED_EDGE('',*,*,#9999,.T.);
#13864=ORIENTED_EDGE('',*,*,#9995,.T.);
#13865=ORIENTED_EDGE('',*,*,#10000,.T.);
#13866=ORIENTED_EDGE('',*,*,#10001,.F.);
#13867=ORIENTED_EDGE('',*,*,#10002,.T.);
#13868=ORIENTED_EDGE('',*,*,#9998,.T.);
#13869=ORIENTED_EDGE('',*,*,#10003,.T.);
#13870=ORIENTED_EDGE('',*,*,#10004,.F.);
#13871=ORIENTED_EDGE('',*,*,#10005,.T.);
#13872=ORIENTED_EDGE('',*,*,#10001,.T.);
#13873=ORIENTED_EDGE('',*,*,#10006,.T.);
#13874=ORIENTED_EDGE('',*,*,#10007,.F.);
#13875=ORIENTED_EDGE('',*,*,#10008,.T.);
#13876=ORIENTED_EDGE('',*,*,#10004,.T.);
#13877=ORIENTED_EDGE('',*,*,#10009,.T.);
#13878=ORIENTED_EDGE('',*,*,#10010,.F.);
#13879=ORIENTED_EDGE('',*,*,#10011,.T.);
#13880=ORIENTED_EDGE('',*,*,#10007,.T.);
#13881=ORIENTED_EDGE('',*,*,#10012,.T.);
#13882=ORIENTED_EDGE('',*,*,#10013,.F.);
#13883=ORIENTED_EDGE('',*,*,#10014,.T.);
#13884=ORIENTED_EDGE('',*,*,#10010,.T.);
#13885=ORIENTED_EDGE('',*,*,#10015,.T.);
#13886=ORIENTED_EDGE('',*,*,#10016,.F.);
#13887=ORIENTED_EDGE('',*,*,#10017,.T.);
#13888=ORIENTED_EDGE('',*,*,#10013,.T.);
#13889=ORIENTED_EDGE('',*,*,#10018,.T.);
#13890=ORIENTED_EDGE('',*,*,#10019,.F.);
#13891=ORIENTED_EDGE('',*,*,#10020,.T.);
#13892=ORIENTED_EDGE('',*,*,#10016,.T.);
#13893=ORIENTED_EDGE('',*,*,#10021,.T.);
#13894=ORIENTED_EDGE('',*,*,#10022,.F.);
#13895=ORIENTED_EDGE('',*,*,#10023,.T.);
#13896=ORIENTED_EDGE('',*,*,#10019,.T.);
#13897=ORIENTED_EDGE('',*,*,#10024,.T.);
#13898=ORIENTED_EDGE('',*,*,#10025,.F.);
#13899=ORIENTED_EDGE('',*,*,#10026,.T.);
#13900=ORIENTED_EDGE('',*,*,#10022,.T.);
#13901=ORIENTED_EDGE('',*,*,#10027,.T.);
#13902=ORIENTED_EDGE('',*,*,#10028,.F.);
#13903=ORIENTED_EDGE('',*,*,#10029,.T.);
#13904=ORIENTED_EDGE('',*,*,#10030,.F.);
#13905=ORIENTED_EDGE('',*,*,#10031,.F.);
#13906=ORIENTED_EDGE('',*,*,#10032,.F.);
#13907=ORIENTED_EDGE('',*,*,#10033,.T.);
#13908=ORIENTED_EDGE('',*,*,#10028,.T.);
#13909=ORIENTED_EDGE('',*,*,#10034,.F.);
#13910=ORIENTED_EDGE('',*,*,#10035,.F.);
#13911=ORIENTED_EDGE('',*,*,#10036,.T.);
#13912=ORIENTED_EDGE('',*,*,#10032,.T.);
#13913=ORIENTED_EDGE('',*,*,#10037,.F.);
#13914=ORIENTED_EDGE('',*,*,#10038,.F.);
#13915=ORIENTED_EDGE('',*,*,#10039,.T.);
#13916=ORIENTED_EDGE('',*,*,#10035,.T.);
#13917=ORIENTED_EDGE('',*,*,#10040,.F.);
#13918=ORIENTED_EDGE('',*,*,#10041,.F.);
#13919=ORIENTED_EDGE('',*,*,#10042,.T.);
#13920=ORIENTED_EDGE('',*,*,#10038,.T.);
#13921=ORIENTED_EDGE('',*,*,#10043,.F.);
#13922=ORIENTED_EDGE('',*,*,#10044,.F.);
#13923=ORIENTED_EDGE('',*,*,#10045,.T.);
#13924=ORIENTED_EDGE('',*,*,#10041,.T.);
#13925=ORIENTED_EDGE('',*,*,#10046,.F.);
#13926=ORIENTED_EDGE('',*,*,#10047,.F.);
#13927=ORIENTED_EDGE('',*,*,#10048,.T.);
#13928=ORIENTED_EDGE('',*,*,#10044,.T.);
#13929=ORIENTED_EDGE('',*,*,#10049,.F.);
#13930=ORIENTED_EDGE('',*,*,#10050,.F.);
#13931=ORIENTED_EDGE('',*,*,#10051,.T.);
#13932=ORIENTED_EDGE('',*,*,#10047,.T.);
#13933=ORIENTED_EDGE('',*,*,#10052,.F.);
#13934=ORIENTED_EDGE('',*,*,#10053,.F.);
#13935=ORIENTED_EDGE('',*,*,#10054,.T.);
#13936=ORIENTED_EDGE('',*,*,#10050,.T.);
#13937=ORIENTED_EDGE('',*,*,#10055,.F.);
#13938=ORIENTED_EDGE('',*,*,#10056,.F.);
#13939=ORIENTED_EDGE('',*,*,#10057,.T.);
#13940=ORIENTED_EDGE('',*,*,#10053,.T.);
#13941=ORIENTED_EDGE('',*,*,#10058,.F.);
#13942=ORIENTED_EDGE('',*,*,#10059,.F.);
#13943=ORIENTED_EDGE('',*,*,#10060,.T.);
#13944=ORIENTED_EDGE('',*,*,#10056,.T.);
#13945=ORIENTED_EDGE('',*,*,#10061,.F.);
#13946=ORIENTED_EDGE('',*,*,#10062,.F.);
#13947=ORIENTED_EDGE('',*,*,#10063,.T.);
#13948=ORIENTED_EDGE('',*,*,#10059,.T.);
#13949=ORIENTED_EDGE('',*,*,#10064,.F.);
#13950=ORIENTED_EDGE('',*,*,#10065,.F.);
#13951=ORIENTED_EDGE('',*,*,#10066,.F.);
#13952=ORIENTED_EDGE('',*,*,#10027,.F.);
#13953=ORIENTED_EDGE('',*,*,#10024,.F.);
#13954=ORIENTED_EDGE('',*,*,#10021,.F.);
#13955=ORIENTED_EDGE('',*,*,#10018,.F.);
#13956=ORIENTED_EDGE('',*,*,#10015,.F.);
#13957=ORIENTED_EDGE('',*,*,#10012,.F.);
#13958=ORIENTED_EDGE('',*,*,#10009,.F.);
#13959=ORIENTED_EDGE('',*,*,#10006,.F.);
#13960=ORIENTED_EDGE('',*,*,#10003,.F.);
#13961=ORIENTED_EDGE('',*,*,#10000,.F.);
#13962=ORIENTED_EDGE('',*,*,#9997,.F.);
#13963=ORIENTED_EDGE('',*,*,#9994,.F.);
#13964=ORIENTED_EDGE('',*,*,#9991,.F.);
#13965=ORIENTED_EDGE('',*,*,#10067,.F.);
#13966=ORIENTED_EDGE('',*,*,#10068,.T.);
#13967=ORIENTED_EDGE('',*,*,#10064,.T.);
#13968=ORIENTED_EDGE('',*,*,#10061,.T.);
#13969=ORIENTED_EDGE('',*,*,#10058,.T.);
#13970=ORIENTED_EDGE('',*,*,#10055,.T.);
#13971=ORIENTED_EDGE('',*,*,#10052,.T.);
#13972=ORIENTED_EDGE('',*,*,#10049,.T.);
#13973=ORIENTED_EDGE('',*,*,#10046,.T.);
#13974=ORIENTED_EDGE('',*,*,#10043,.T.);
#13975=ORIENTED_EDGE('',*,*,#10040,.T.);
#13976=ORIENTED_EDGE('',*,*,#10037,.T.);
#13977=ORIENTED_EDGE('',*,*,#10034,.T.);
#13978=ORIENTED_EDGE('',*,*,#10031,.T.);
#13979=ORIENTED_EDGE('',*,*,#10069,.T.);
#13980=ORIENTED_EDGE('',*,*,#10070,.T.);
#13981=ORIENTED_EDGE('',*,*,#10071,.T.);
#13982=ORIENTED_EDGE('',*,*,#10072,.T.);
#13983=ORIENTED_EDGE('',*,*,#10067,.T.);
#13984=ORIENTED_EDGE('',*,*,#10062,.T.);
#13985=ORIENTED_EDGE('',*,*,#10068,.F.);
#13986=ORIENTED_EDGE('',*,*,#10072,.F.);
#13987=ORIENTED_EDGE('',*,*,#10073,.T.);
#13988=ORIENTED_EDGE('',*,*,#10074,.F.);
#13989=ORIENTED_EDGE('',*,*,#10029,.F.);
#13990=ORIENTED_EDGE('',*,*,#10033,.F.);
#13991=ORIENTED_EDGE('',*,*,#10036,.F.);
#13992=ORIENTED_EDGE('',*,*,#10039,.F.);
#13993=ORIENTED_EDGE('',*,*,#10042,.F.);
#13994=ORIENTED_EDGE('',*,*,#10045,.F.);
#13995=ORIENTED_EDGE('',*,*,#10048,.F.);
#13996=ORIENTED_EDGE('',*,*,#10051,.F.);
#13997=ORIENTED_EDGE('',*,*,#10054,.F.);
#13998=ORIENTED_EDGE('',*,*,#10057,.F.);
#13999=ORIENTED_EDGE('',*,*,#10060,.F.);
#14000=ORIENTED_EDGE('',*,*,#10063,.F.);
#14001=ORIENTED_EDGE('',*,*,#10073,.F.);
#14002=ORIENTED_EDGE('',*,*,#10071,.F.);
#14003=ORIENTED_EDGE('',*,*,#9989,.F.);
#14004=ORIENTED_EDGE('',*,*,#9993,.F.);
#14005=ORIENTED_EDGE('',*,*,#9996,.F.);
#14006=ORIENTED_EDGE('',*,*,#9999,.F.);
#14007=ORIENTED_EDGE('',*,*,#10002,.F.);
#14008=ORIENTED_EDGE('',*,*,#10005,.F.);
#14009=ORIENTED_EDGE('',*,*,#10008,.F.);
#14010=ORIENTED_EDGE('',*,*,#10011,.F.);
#14011=ORIENTED_EDGE('',*,*,#10014,.F.);
#14012=ORIENTED_EDGE('',*,*,#10017,.F.);
#14013=ORIENTED_EDGE('',*,*,#10020,.F.);
#14014=ORIENTED_EDGE('',*,*,#10023,.F.);
#14015=ORIENTED_EDGE('',*,*,#10026,.F.);
#14016=ORIENTED_EDGE('',*,*,#10075,.F.);
#14017=ORIENTED_EDGE('',*,*,#10065,.T.);
#14018=ORIENTED_EDGE('',*,*,#10030,.T.);
#14019=ORIENTED_EDGE('',*,*,#10074,.T.);
#14020=ORIENTED_EDGE('',*,*,#10076,.T.);
#14021=ORIENTED_EDGE('',*,*,#10077,.F.);
#14022=ORIENTED_EDGE('',*,*,#10078,.F.);
#14023=ORIENTED_EDGE('',*,*,#10079,.T.);
#14024=ORIENTED_EDGE('',*,*,#10080,.T.);
#14025=ORIENTED_EDGE('',*,*,#10081,.F.);
#14026=ORIENTED_EDGE('',*,*,#10082,.F.);
#14027=ORIENTED_EDGE('',*,*,#10083,.T.);
#14028=ORIENTED_EDGE('',*,*,#10084,.T.);
#14029=ORIENTED_EDGE('',*,*,#10079,.F.);
#14030=ORIENTED_EDGE('',*,*,#10085,.F.);
#14031=ORIENTED_EDGE('',*,*,#10086,.T.);
#14032=ORIENTED_EDGE('',*,*,#10087,.T.);
#14033=ORIENTED_EDGE('',*,*,#10083,.F.);
#14034=ORIENTED_EDGE('',*,*,#10088,.F.);
#14035=ORIENTED_EDGE('',*,*,#10089,.T.);
#14036=ORIENTED_EDGE('',*,*,#10090,.T.);
#14037=ORIENTED_EDGE('',*,*,#10086,.F.);
#14038=ORIENTED_EDGE('',*,*,#10091,.F.);
#14039=ORIENTED_EDGE('',*,*,#10092,.T.);
#14040=ORIENTED_EDGE('',*,*,#10093,.T.);
#14041=ORIENTED_EDGE('',*,*,#10089,.F.);
#14042=ORIENTED_EDGE('',*,*,#10094,.F.);
#14043=ORIENTED_EDGE('',*,*,#10095,.T.);
#14044=ORIENTED_EDGE('',*,*,#10096,.T.);
#14045=ORIENTED_EDGE('',*,*,#10092,.F.);
#14046=ORIENTED_EDGE('',*,*,#10097,.F.);
#14047=ORIENTED_EDGE('',*,*,#10098,.T.);
#14048=ORIENTED_EDGE('',*,*,#10099,.T.);
#14049=ORIENTED_EDGE('',*,*,#10095,.F.);
#14050=ORIENTED_EDGE('',*,*,#10100,.F.);
#14051=ORIENTED_EDGE('',*,*,#10101,.T.);
#14052=ORIENTED_EDGE('',*,*,#10102,.T.);
#14053=ORIENTED_EDGE('',*,*,#10098,.F.);
#14054=ORIENTED_EDGE('',*,*,#10103,.F.);
#14055=ORIENTED_EDGE('',*,*,#10104,.T.);
#14056=ORIENTED_EDGE('',*,*,#10105,.T.);
#14057=ORIENTED_EDGE('',*,*,#10101,.F.);
#14058=ORIENTED_EDGE('',*,*,#10106,.F.);
#14059=ORIENTED_EDGE('',*,*,#10107,.T.);
#14060=ORIENTED_EDGE('',*,*,#10108,.T.);
#14061=ORIENTED_EDGE('',*,*,#10104,.F.);
#14062=ORIENTED_EDGE('',*,*,#10109,.F.);
#14063=ORIENTED_EDGE('',*,*,#10081,.T.);
#14064=ORIENTED_EDGE('',*,*,#10110,.T.);
#14065=ORIENTED_EDGE('',*,*,#10107,.F.);
#14066=ORIENTED_EDGE('',*,*,#10110,.F.);
#14067=ORIENTED_EDGE('',*,*,#10080,.F.);
#14068=ORIENTED_EDGE('',*,*,#10084,.F.);
#14069=ORIENTED_EDGE('',*,*,#10087,.F.);
#14070=ORIENTED_EDGE('',*,*,#10090,.F.);
#14071=ORIENTED_EDGE('',*,*,#10093,.F.);
#14072=ORIENTED_EDGE('',*,*,#10096,.F.);
#14073=ORIENTED_EDGE('',*,*,#10099,.F.);
#14074=ORIENTED_EDGE('',*,*,#10102,.F.);
#14075=ORIENTED_EDGE('',*,*,#10105,.F.);
#14076=ORIENTED_EDGE('',*,*,#10108,.F.);
#14077=ORIENTED_EDGE('',*,*,#10111,.F.);
#14078=ORIENTED_EDGE('',*,*,#10112,.T.);
#14079=ORIENTED_EDGE('',*,*,#10113,.T.);
#14080=ORIENTED_EDGE('',*,*,#10114,.F.);
#14081=ORIENTED_EDGE('',*,*,#10115,.F.);
#14082=ORIENTED_EDGE('',*,*,#10116,.T.);
#14083=ORIENTED_EDGE('',*,*,#10117,.T.);
#14084=ORIENTED_EDGE('',*,*,#10112,.F.);
#14085=ORIENTED_EDGE('',*,*,#10118,.F.);
#14086=ORIENTED_EDGE('',*,*,#10119,.T.);
#14087=ORIENTED_EDGE('',*,*,#10120,.T.);
#14088=ORIENTED_EDGE('',*,*,#10116,.F.);
#14089=ORIENTED_EDGE('',*,*,#10121,.F.);
#14090=ORIENTED_EDGE('',*,*,#10122,.T.);
#14091=ORIENTED_EDGE('',*,*,#10123,.T.);
#14092=ORIENTED_EDGE('',*,*,#10119,.F.);
#14093=ORIENTED_EDGE('',*,*,#10124,.F.);
#14094=ORIENTED_EDGE('',*,*,#10125,.T.);
#14095=ORIENTED_EDGE('',*,*,#10126,.T.);
#14096=ORIENTED_EDGE('',*,*,#10122,.F.);
#14097=ORIENTED_EDGE('',*,*,#10127,.F.);
#14098=ORIENTED_EDGE('',*,*,#10128,.T.);
#14099=ORIENTED_EDGE('',*,*,#10129,.T.);
#14100=ORIENTED_EDGE('',*,*,#10125,.F.);
#14101=ORIENTED_EDGE('',*,*,#10130,.F.);
#14102=ORIENTED_EDGE('',*,*,#10131,.T.);
#14103=ORIENTED_EDGE('',*,*,#10132,.T.);
#14104=ORIENTED_EDGE('',*,*,#10128,.F.);
#14105=ORIENTED_EDGE('',*,*,#10133,.F.);
#14106=ORIENTED_EDGE('',*,*,#10134,.T.);
#14107=ORIENTED_EDGE('',*,*,#10135,.T.);
#14108=ORIENTED_EDGE('',*,*,#10131,.F.);
#14109=ORIENTED_EDGE('',*,*,#10136,.F.);
#14110=ORIENTED_EDGE('',*,*,#10137,.T.);
#14111=ORIENTED_EDGE('',*,*,#10138,.T.);
#14112=ORIENTED_EDGE('',*,*,#10134,.F.);
#14113=ORIENTED_EDGE('',*,*,#10139,.F.);
#14114=ORIENTED_EDGE('',*,*,#10114,.T.);
#14115=ORIENTED_EDGE('',*,*,#10140,.T.);
#14116=ORIENTED_EDGE('',*,*,#10137,.F.);
#14117=ORIENTED_EDGE('',*,*,#10140,.F.);
#14118=ORIENTED_EDGE('',*,*,#10113,.F.);
#14119=ORIENTED_EDGE('',*,*,#10117,.F.);
#14120=ORIENTED_EDGE('',*,*,#10120,.F.);
#14121=ORIENTED_EDGE('',*,*,#10123,.F.);
#14122=ORIENTED_EDGE('',*,*,#10126,.F.);
#14123=ORIENTED_EDGE('',*,*,#10129,.F.);
#14124=ORIENTED_EDGE('',*,*,#10132,.F.);
#14125=ORIENTED_EDGE('',*,*,#10135,.F.);
#14126=ORIENTED_EDGE('',*,*,#10138,.F.);
#14127=ORIENTED_EDGE('',*,*,#10141,.F.);
#14128=ORIENTED_EDGE('',*,*,#10142,.T.);
#14129=ORIENTED_EDGE('',*,*,#10143,.T.);
#14130=ORIENTED_EDGE('',*,*,#10144,.F.);
#14131=ORIENTED_EDGE('',*,*,#10145,.F.);
#14132=ORIENTED_EDGE('',*,*,#10146,.T.);
#14133=ORIENTED_EDGE('',*,*,#10147,.T.);
#14134=ORIENTED_EDGE('',*,*,#10142,.F.);
#14135=ORIENTED_EDGE('',*,*,#10148,.F.);
#14136=ORIENTED_EDGE('',*,*,#10149,.T.);
#14137=ORIENTED_EDGE('',*,*,#10150,.T.);
#14138=ORIENTED_EDGE('',*,*,#10146,.F.);
#14139=ORIENTED_EDGE('',*,*,#10151,.F.);
#14140=ORIENTED_EDGE('',*,*,#10152,.T.);
#14141=ORIENTED_EDGE('',*,*,#10153,.T.);
#14142=ORIENTED_EDGE('',*,*,#10149,.F.);
#14143=ORIENTED_EDGE('',*,*,#10154,.F.);
#14144=ORIENTED_EDGE('',*,*,#10155,.T.);
#14145=ORIENTED_EDGE('',*,*,#10156,.T.);
#14146=ORIENTED_EDGE('',*,*,#10152,.F.);
#14147=ORIENTED_EDGE('',*,*,#10157,.F.);
#14148=ORIENTED_EDGE('',*,*,#10158,.T.);
#14149=ORIENTED_EDGE('',*,*,#10159,.T.);
#14150=ORIENTED_EDGE('',*,*,#10155,.F.);
#14151=ORIENTED_EDGE('',*,*,#10160,.F.);
#14152=ORIENTED_EDGE('',*,*,#10161,.T.);
#14153=ORIENTED_EDGE('',*,*,#10162,.T.);
#14154=ORIENTED_EDGE('',*,*,#10158,.F.);
#14155=ORIENTED_EDGE('',*,*,#10163,.F.);
#14156=ORIENTED_EDGE('',*,*,#10164,.T.);
#14157=ORIENTED_EDGE('',*,*,#10165,.T.);
#14158=ORIENTED_EDGE('',*,*,#10161,.F.);
#14159=ORIENTED_EDGE('',*,*,#10166,.F.);
#14160=ORIENTED_EDGE('',*,*,#10167,.T.);
#14161=ORIENTED_EDGE('',*,*,#10168,.T.);
#14162=ORIENTED_EDGE('',*,*,#10164,.F.);
#14163=ORIENTED_EDGE('',*,*,#10169,.F.);
#14164=ORIENTED_EDGE('',*,*,#10170,.T.);
#14165=ORIENTED_EDGE('',*,*,#10171,.T.);
#14166=ORIENTED_EDGE('',*,*,#10167,.F.);
#14167=ORIENTED_EDGE('',*,*,#10172,.F.);
#14168=ORIENTED_EDGE('',*,*,#10144,.T.);
#14169=ORIENTED_EDGE('',*,*,#10173,.T.);
#14170=ORIENTED_EDGE('',*,*,#10170,.F.);
#14171=ORIENTED_EDGE('',*,*,#10173,.F.);
#14172=ORIENTED_EDGE('',*,*,#10143,.F.);
#14173=ORIENTED_EDGE('',*,*,#10147,.F.);
#14174=ORIENTED_EDGE('',*,*,#10150,.F.);
#14175=ORIENTED_EDGE('',*,*,#10153,.F.);
#14176=ORIENTED_EDGE('',*,*,#10156,.F.);
#14177=ORIENTED_EDGE('',*,*,#10159,.F.);
#14178=ORIENTED_EDGE('',*,*,#10162,.F.);
#14179=ORIENTED_EDGE('',*,*,#10165,.F.);
#14180=ORIENTED_EDGE('',*,*,#10168,.F.);
#14181=ORIENTED_EDGE('',*,*,#10171,.F.);
#14182=ORIENTED_EDGE('',*,*,#10174,.F.);
#14183=ORIENTED_EDGE('',*,*,#10175,.T.);
#14184=ORIENTED_EDGE('',*,*,#10176,.T.);
#14185=ORIENTED_EDGE('',*,*,#10177,.F.);
#14186=ORIENTED_EDGE('',*,*,#10178,.F.);
#14187=ORIENTED_EDGE('',*,*,#10179,.T.);
#14188=ORIENTED_EDGE('',*,*,#10180,.T.);
#14189=ORIENTED_EDGE('',*,*,#10175,.F.);
#14190=ORIENTED_EDGE('',*,*,#10181,.F.);
#14191=ORIENTED_EDGE('',*,*,#10182,.T.);
#14192=ORIENTED_EDGE('',*,*,#10183,.T.);
#14193=ORIENTED_EDGE('',*,*,#10179,.F.);
#14194=ORIENTED_EDGE('',*,*,#10184,.F.);
#14195=ORIENTED_EDGE('',*,*,#10185,.T.);
#14196=ORIENTED_EDGE('',*,*,#10186,.T.);
#14197=ORIENTED_EDGE('',*,*,#10182,.F.);
#14198=ORIENTED_EDGE('',*,*,#10187,.F.);
#14199=ORIENTED_EDGE('',*,*,#10188,.T.);
#14200=ORIENTED_EDGE('',*,*,#10189,.T.);
#14201=ORIENTED_EDGE('',*,*,#10185,.F.);
#14202=ORIENTED_EDGE('',*,*,#10190,.F.);
#14203=ORIENTED_EDGE('',*,*,#10191,.T.);
#14204=ORIENTED_EDGE('',*,*,#10192,.T.);
#14205=ORIENTED_EDGE('',*,*,#10188,.F.);
#14206=ORIENTED_EDGE('',*,*,#10193,.F.);
#14207=ORIENTED_EDGE('',*,*,#10194,.T.);
#14208=ORIENTED_EDGE('',*,*,#10195,.T.);
#14209=ORIENTED_EDGE('',*,*,#10191,.F.);
#14210=ORIENTED_EDGE('',*,*,#10196,.F.);
#14211=ORIENTED_EDGE('',*,*,#10197,.T.);
#14212=ORIENTED_EDGE('',*,*,#10198,.T.);
#14213=ORIENTED_EDGE('',*,*,#10194,.F.);
#14214=ORIENTED_EDGE('',*,*,#10199,.F.);
#14215=ORIENTED_EDGE('',*,*,#10200,.T.);
#14216=ORIENTED_EDGE('',*,*,#10201,.T.);
#14217=ORIENTED_EDGE('',*,*,#10197,.F.);
#14218=ORIENTED_EDGE('',*,*,#10202,.F.);
#14219=ORIENTED_EDGE('',*,*,#10177,.T.);
#14220=ORIENTED_EDGE('',*,*,#10203,.T.);
#14221=ORIENTED_EDGE('',*,*,#10200,.F.);
#14222=ORIENTED_EDGE('',*,*,#10203,.F.);
#14223=ORIENTED_EDGE('',*,*,#10176,.F.);
#14224=ORIENTED_EDGE('',*,*,#10180,.F.);
#14225=ORIENTED_EDGE('',*,*,#10183,.F.);
#14226=ORIENTED_EDGE('',*,*,#10186,.F.);
#14227=ORIENTED_EDGE('',*,*,#10189,.F.);
#14228=ORIENTED_EDGE('',*,*,#10192,.F.);
#14229=ORIENTED_EDGE('',*,*,#10195,.F.);
#14230=ORIENTED_EDGE('',*,*,#10198,.F.);
#14231=ORIENTED_EDGE('',*,*,#10201,.F.);
#14232=ORIENTED_EDGE('',*,*,#10204,.F.);
#14233=ORIENTED_EDGE('',*,*,#10205,.T.);
#14234=ORIENTED_EDGE('',*,*,#10206,.T.);
#14235=ORIENTED_EDGE('',*,*,#10207,.F.);
#14236=ORIENTED_EDGE('',*,*,#10208,.F.);
#14237=ORIENTED_EDGE('',*,*,#10209,.T.);
#14238=ORIENTED_EDGE('',*,*,#10210,.T.);
#14239=ORIENTED_EDGE('',*,*,#10205,.F.);
#14240=ORIENTED_EDGE('',*,*,#10211,.F.);
#14241=ORIENTED_EDGE('',*,*,#10212,.T.);
#14242=ORIENTED_EDGE('',*,*,#10213,.T.);
#14243=ORIENTED_EDGE('',*,*,#10209,.F.);
#14244=ORIENTED_EDGE('',*,*,#10214,.F.);
#14245=ORIENTED_EDGE('',*,*,#10215,.T.);
#14246=ORIENTED_EDGE('',*,*,#10216,.T.);
#14247=ORIENTED_EDGE('',*,*,#10212,.F.);
#14248=ORIENTED_EDGE('',*,*,#10217,.F.);
#14249=ORIENTED_EDGE('',*,*,#10218,.T.);
#14250=ORIENTED_EDGE('',*,*,#10219,.T.);
#14251=ORIENTED_EDGE('',*,*,#10215,.F.);
#14252=ORIENTED_EDGE('',*,*,#10220,.F.);
#14253=ORIENTED_EDGE('',*,*,#10221,.T.);
#14254=ORIENTED_EDGE('',*,*,#10222,.T.);
#14255=ORIENTED_EDGE('',*,*,#10218,.F.);
#14256=ORIENTED_EDGE('',*,*,#10223,.F.);
#14257=ORIENTED_EDGE('',*,*,#10224,.T.);
#14258=ORIENTED_EDGE('',*,*,#10225,.T.);
#14259=ORIENTED_EDGE('',*,*,#10221,.F.);
#14260=ORIENTED_EDGE('',*,*,#10226,.F.);
#14261=ORIENTED_EDGE('',*,*,#10227,.T.);
#14262=ORIENTED_EDGE('',*,*,#10228,.T.);
#14263=ORIENTED_EDGE('',*,*,#10224,.F.);
#14264=ORIENTED_EDGE('',*,*,#10229,.F.);
#14265=ORIENTED_EDGE('',*,*,#10230,.T.);
#14266=ORIENTED_EDGE('',*,*,#10231,.T.);
#14267=ORIENTED_EDGE('',*,*,#10227,.F.);
#14268=ORIENTED_EDGE('',*,*,#10232,.F.);
#14269=ORIENTED_EDGE('',*,*,#10207,.T.);
#14270=ORIENTED_EDGE('',*,*,#10233,.T.);
#14271=ORIENTED_EDGE('',*,*,#10230,.F.);
#14272=ORIENTED_EDGE('',*,*,#10233,.F.);
#14273=ORIENTED_EDGE('',*,*,#10206,.F.);
#14274=ORIENTED_EDGE('',*,*,#10210,.F.);
#14275=ORIENTED_EDGE('',*,*,#10213,.F.);
#14276=ORIENTED_EDGE('',*,*,#10216,.F.);
#14277=ORIENTED_EDGE('',*,*,#10219,.F.);
#14278=ORIENTED_EDGE('',*,*,#10222,.F.);
#14279=ORIENTED_EDGE('',*,*,#10225,.F.);
#14280=ORIENTED_EDGE('',*,*,#10228,.F.);
#14281=ORIENTED_EDGE('',*,*,#10231,.F.);
#14282=ORIENTED_EDGE('',*,*,#10234,.T.);
#14283=ORIENTED_EDGE('',*,*,#10235,.F.);
#14284=ORIENTED_EDGE('',*,*,#10234,.F.);
#14285=ORIENTED_EDGE('',*,*,#10236,.T.);
#14286=ORIENTED_EDGE('',*,*,#10237,.F.);
#14287=ORIENTED_EDGE('',*,*,#10236,.F.);
#14288=ORIENTED_EDGE('',*,*,#10235,.T.);
#14289=ORIENTED_EDGE('',*,*,#10238,.T.);
#14290=ORIENTED_EDGE('',*,*,#10239,.F.);
#14291=ORIENTED_EDGE('',*,*,#10238,.F.);
#14292=ORIENTED_EDGE('',*,*,#10239,.T.);
#14293=ORIENTED_EDGE('',*,*,#10240,.F.);
#14294=ORIENTED_EDGE('',*,*,#10241,.T.);
#14295=ORIENTED_EDGE('',*,*,#10242,.F.);
#14296=ORIENTED_EDGE('',*,*,#10243,.F.);
#14297=ORIENTED_EDGE('',*,*,#10244,.F.);
#14298=ORIENTED_EDGE('',*,*,#10243,.T.);
#14299=ORIENTED_EDGE('',*,*,#10245,.T.);
#14300=ORIENTED_EDGE('',*,*,#10246,.F.);
#14301=ORIENTED_EDGE('',*,*,#10245,.F.);
#14302=ORIENTED_EDGE('',*,*,#10242,.T.);
#14303=ORIENTED_EDGE('',*,*,#10247,.T.);
#14304=ORIENTED_EDGE('',*,*,#10248,.F.);
#14305=ORIENTED_EDGE('',*,*,#10247,.F.);
#14306=ORIENTED_EDGE('',*,*,#10241,.F.);
#14307=ORIENTED_EDGE('',*,*,#10249,.F.);
#14308=ORIENTED_EDGE('',*,*,#10250,.T.);
#14309=ORIENTED_EDGE('',*,*,#10251,.F.);
#14310=ORIENTED_EDGE('',*,*,#10252,.F.);
#14311=ORIENTED_EDGE('',*,*,#10253,.F.);
#14312=ORIENTED_EDGE('',*,*,#10252,.T.);
#14313=ORIENTED_EDGE('',*,*,#10254,.T.);
#14314=ORIENTED_EDGE('',*,*,#10255,.F.);
#14315=ORIENTED_EDGE('',*,*,#10254,.F.);
#14316=ORIENTED_EDGE('',*,*,#10251,.T.);
#14317=ORIENTED_EDGE('',*,*,#10256,.T.);
#14318=ORIENTED_EDGE('',*,*,#10257,.F.);
#14319=ORIENTED_EDGE('',*,*,#10256,.F.);
#14320=ORIENTED_EDGE('',*,*,#10250,.F.);
#14321=ORIENTED_EDGE('',*,*,#10258,.F.);
#14322=ORIENTED_EDGE('',*,*,#10259,.T.);
#14323=ORIENTED_EDGE('',*,*,#10260,.F.);
#14324=ORIENTED_EDGE('',*,*,#10261,.F.);
#14325=ORIENTED_EDGE('',*,*,#10262,.F.);
#14326=ORIENTED_EDGE('',*,*,#10261,.T.);
#14327=ORIENTED_EDGE('',*,*,#10263,.T.);
#14328=ORIENTED_EDGE('',*,*,#10264,.F.);
#14329=ORIENTED_EDGE('',*,*,#10263,.F.);
#14330=ORIENTED_EDGE('',*,*,#10260,.T.);
#14331=ORIENTED_EDGE('',*,*,#10265,.T.);
#14332=ORIENTED_EDGE('',*,*,#10266,.F.);
#14333=ORIENTED_EDGE('',*,*,#10265,.F.);
#14334=ORIENTED_EDGE('',*,*,#10259,.F.);
#14335=ORIENTED_EDGE('',*,*,#10267,.F.);
#14336=ORIENTED_EDGE('',*,*,#10268,.T.);
#14337=ORIENTED_EDGE('',*,*,#10269,.F.);
#14338=ORIENTED_EDGE('',*,*,#10270,.F.);
#14339=ORIENTED_EDGE('',*,*,#10271,.F.);
#14340=ORIENTED_EDGE('',*,*,#10270,.T.);
#14341=ORIENTED_EDGE('',*,*,#10272,.T.);
#14342=ORIENTED_EDGE('',*,*,#10273,.F.);
#14343=ORIENTED_EDGE('',*,*,#10272,.F.);
#14344=ORIENTED_EDGE('',*,*,#10269,.T.);
#14345=ORIENTED_EDGE('',*,*,#10274,.T.);
#14346=ORIENTED_EDGE('',*,*,#10275,.F.);
#14347=ORIENTED_EDGE('',*,*,#10274,.F.);
#14348=ORIENTED_EDGE('',*,*,#10268,.F.);
#14349=ORIENTED_EDGE('',*,*,#10276,.F.);
#14350=ORIENTED_EDGE('',*,*,#10277,.T.);
#14351=ORIENTED_EDGE('',*,*,#10278,.F.);
#14352=ORIENTED_EDGE('',*,*,#10279,.F.);
#14353=ORIENTED_EDGE('',*,*,#10280,.F.);
#14354=ORIENTED_EDGE('',*,*,#10279,.T.);
#14355=ORIENTED_EDGE('',*,*,#10281,.T.);
#14356=ORIENTED_EDGE('',*,*,#10282,.F.);
#14357=ORIENTED_EDGE('',*,*,#10281,.F.);
#14358=ORIENTED_EDGE('',*,*,#10278,.T.);
#14359=ORIENTED_EDGE('',*,*,#10283,.T.);
#14360=ORIENTED_EDGE('',*,*,#10284,.F.);
#14361=ORIENTED_EDGE('',*,*,#10283,.F.);
#14362=ORIENTED_EDGE('',*,*,#10277,.F.);
#14363=ORIENTED_EDGE('',*,*,#10285,.F.);
#14364=ORIENTED_EDGE('',*,*,#10286,.T.);
#14365=ORIENTED_EDGE('',*,*,#10287,.F.);
#14366=ORIENTED_EDGE('',*,*,#10288,.F.);
#14367=ORIENTED_EDGE('',*,*,#10289,.F.);
#14368=ORIENTED_EDGE('',*,*,#10288,.T.);
#14369=ORIENTED_EDGE('',*,*,#10290,.T.);
#14370=ORIENTED_EDGE('',*,*,#10291,.F.);
#14371=ORIENTED_EDGE('',*,*,#10290,.F.);
#14372=ORIENTED_EDGE('',*,*,#10287,.T.);
#14373=ORIENTED_EDGE('',*,*,#10292,.T.);
#14374=ORIENTED_EDGE('',*,*,#10293,.F.);
#14375=ORIENTED_EDGE('',*,*,#10292,.F.);
#14376=ORIENTED_EDGE('',*,*,#10286,.F.);
#14377=ORIENTED_EDGE('',*,*,#10294,.F.);
#14378=ORIENTED_EDGE('',*,*,#10295,.T.);
#14379=ORIENTED_EDGE('',*,*,#10296,.F.);
#14380=ORIENTED_EDGE('',*,*,#10297,.F.);
#14381=ORIENTED_EDGE('',*,*,#10298,.F.);
#14382=ORIENTED_EDGE('',*,*,#10297,.T.);
#14383=ORIENTED_EDGE('',*,*,#10299,.T.);
#14384=ORIENTED_EDGE('',*,*,#10300,.F.);
#14385=ORIENTED_EDGE('',*,*,#10299,.F.);
#14386=ORIENTED_EDGE('',*,*,#10296,.T.);
#14387=ORIENTED_EDGE('',*,*,#10301,.T.);
#14388=ORIENTED_EDGE('',*,*,#10302,.F.);
#14389=ORIENTED_EDGE('',*,*,#10301,.F.);
#14390=ORIENTED_EDGE('',*,*,#10295,.F.);
#14391=ORIENTED_EDGE('',*,*,#10303,.F.);
#14392=ORIENTED_EDGE('',*,*,#10304,.T.);
#14393=ORIENTED_EDGE('',*,*,#10305,.F.);
#14394=ORIENTED_EDGE('',*,*,#10306,.F.);
#14395=ORIENTED_EDGE('',*,*,#10307,.F.);
#14396=ORIENTED_EDGE('',*,*,#10306,.T.);
#14397=ORIENTED_EDGE('',*,*,#10308,.T.);
#14398=ORIENTED_EDGE('',*,*,#10309,.F.);
#14399=ORIENTED_EDGE('',*,*,#10308,.F.);
#14400=ORIENTED_EDGE('',*,*,#10305,.T.);
#14401=ORIENTED_EDGE('',*,*,#10310,.T.);
#14402=ORIENTED_EDGE('',*,*,#10311,.F.);
#14403=ORIENTED_EDGE('',*,*,#10310,.F.);
#14404=ORIENTED_EDGE('',*,*,#10304,.F.);
#14405=ORIENTED_EDGE('',*,*,#10312,.F.);
#14406=ORIENTED_EDGE('',*,*,#10313,.T.);
#14407=ORIENTED_EDGE('',*,*,#10314,.F.);
#14408=ORIENTED_EDGE('',*,*,#10315,.F.);
#14409=ORIENTED_EDGE('',*,*,#10316,.F.);
#14410=ORIENTED_EDGE('',*,*,#10315,.T.);
#14411=ORIENTED_EDGE('',*,*,#10317,.T.);
#14412=ORIENTED_EDGE('',*,*,#10318,.F.);
#14413=ORIENTED_EDGE('',*,*,#10317,.F.);
#14414=ORIENTED_EDGE('',*,*,#10314,.T.);
#14415=ORIENTED_EDGE('',*,*,#10319,.T.);
#14416=ORIENTED_EDGE('',*,*,#10320,.F.);
#14417=ORIENTED_EDGE('',*,*,#10319,.F.);
#14418=ORIENTED_EDGE('',*,*,#10313,.F.);
#14419=ORIENTED_EDGE('',*,*,#10321,.F.);
#14420=ORIENTED_EDGE('',*,*,#10322,.T.);
#14421=ORIENTED_EDGE('',*,*,#10323,.F.);
#14422=ORIENTED_EDGE('',*,*,#10324,.F.);
#14423=ORIENTED_EDGE('',*,*,#10325,.F.);
#14424=ORIENTED_EDGE('',*,*,#10324,.T.);
#14425=ORIENTED_EDGE('',*,*,#10326,.T.);
#14426=ORIENTED_EDGE('',*,*,#10327,.F.);
#14427=ORIENTED_EDGE('',*,*,#10326,.F.);
#14428=ORIENTED_EDGE('',*,*,#10323,.T.);
#14429=ORIENTED_EDGE('',*,*,#10328,.T.);
#14430=ORIENTED_EDGE('',*,*,#10329,.F.);
#14431=ORIENTED_EDGE('',*,*,#10328,.F.);
#14432=ORIENTED_EDGE('',*,*,#10322,.F.);
#14433=ORIENTED_EDGE('',*,*,#10330,.F.);
#14434=ORIENTED_EDGE('',*,*,#10331,.T.);
#14435=ORIENTED_EDGE('',*,*,#10332,.F.);
#14436=ORIENTED_EDGE('',*,*,#10333,.F.);
#14437=ORIENTED_EDGE('',*,*,#10334,.F.);
#14438=ORIENTED_EDGE('',*,*,#10333,.T.);
#14439=ORIENTED_EDGE('',*,*,#10335,.T.);
#14440=ORIENTED_EDGE('',*,*,#10336,.F.);
#14441=ORIENTED_EDGE('',*,*,#10335,.F.);
#14442=ORIENTED_EDGE('',*,*,#10332,.T.);
#14443=ORIENTED_EDGE('',*,*,#10337,.T.);
#14444=ORIENTED_EDGE('',*,*,#10338,.F.);
#14445=ORIENTED_EDGE('',*,*,#10337,.F.);
#14446=ORIENTED_EDGE('',*,*,#10331,.F.);
#14447=ORIENTED_EDGE('',*,*,#10339,.F.);
#14448=ORIENTED_EDGE('',*,*,#10340,.T.);
#14449=ORIENTED_EDGE('',*,*,#10341,.F.);
#14450=ORIENTED_EDGE('',*,*,#10342,.F.);
#14451=ORIENTED_EDGE('',*,*,#10343,.F.);
#14452=ORIENTED_EDGE('',*,*,#10342,.T.);
#14453=ORIENTED_EDGE('',*,*,#10344,.T.);
#14454=ORIENTED_EDGE('',*,*,#10345,.F.);
#14455=ORIENTED_EDGE('',*,*,#10344,.F.);
#14456=ORIENTED_EDGE('',*,*,#10341,.T.);
#14457=ORIENTED_EDGE('',*,*,#10346,.T.);
#14458=ORIENTED_EDGE('',*,*,#10347,.F.);
#14459=ORIENTED_EDGE('',*,*,#10346,.F.);
#14460=ORIENTED_EDGE('',*,*,#10340,.F.);
#14461=ORIENTED_EDGE('',*,*,#10348,.F.);
#14462=ORIENTED_EDGE('',*,*,#10349,.T.);
#14463=ORIENTED_EDGE('',*,*,#10350,.F.);
#14464=ORIENTED_EDGE('',*,*,#10351,.F.);
#14465=ORIENTED_EDGE('',*,*,#10352,.F.);
#14466=ORIENTED_EDGE('',*,*,#10351,.T.);
#14467=ORIENTED_EDGE('',*,*,#10353,.T.);
#14468=ORIENTED_EDGE('',*,*,#10354,.F.);
#14469=ORIENTED_EDGE('',*,*,#10353,.F.);
#14470=ORIENTED_EDGE('',*,*,#10350,.T.);
#14471=ORIENTED_EDGE('',*,*,#10355,.T.);
#14472=ORIENTED_EDGE('',*,*,#10356,.F.);
#14473=ORIENTED_EDGE('',*,*,#10355,.F.);
#14474=ORIENTED_EDGE('',*,*,#10349,.F.);
#14475=ORIENTED_EDGE('',*,*,#10357,.F.);
#14476=ORIENTED_EDGE('',*,*,#10358,.T.);
#14477=ORIENTED_EDGE('',*,*,#10359,.F.);
#14478=ORIENTED_EDGE('',*,*,#10360,.F.);
#14479=ORIENTED_EDGE('',*,*,#10361,.F.);
#14480=ORIENTED_EDGE('',*,*,#10360,.T.);
#14481=ORIENTED_EDGE('',*,*,#10362,.T.);
#14482=ORIENTED_EDGE('',*,*,#10363,.F.);
#14483=ORIENTED_EDGE('',*,*,#10362,.F.);
#14484=ORIENTED_EDGE('',*,*,#10359,.T.);
#14485=ORIENTED_EDGE('',*,*,#10364,.T.);
#14486=ORIENTED_EDGE('',*,*,#10365,.F.);
#14487=ORIENTED_EDGE('',*,*,#10364,.F.);
#14488=ORIENTED_EDGE('',*,*,#10358,.F.);
#14489=ORIENTED_EDGE('',*,*,#10366,.F.);
#14490=ORIENTED_EDGE('',*,*,#10367,.T.);
#14491=ORIENTED_EDGE('',*,*,#10368,.F.);
#14492=ORIENTED_EDGE('',*,*,#10369,.F.);
#14493=ORIENTED_EDGE('',*,*,#10370,.F.);
#14494=ORIENTED_EDGE('',*,*,#10369,.T.);
#14495=ORIENTED_EDGE('',*,*,#10371,.T.);
#14496=ORIENTED_EDGE('',*,*,#10372,.F.);
#14497=ORIENTED_EDGE('',*,*,#10373,.F.);
#14498=ORIENTED_EDGE('',*,*,#10371,.F.);
#14499=ORIENTED_EDGE('',*,*,#10368,.T.);
#14500=ORIENTED_EDGE('',*,*,#10374,.T.);
#14501=ORIENTED_EDGE('',*,*,#10375,.F.);
#14502=ORIENTED_EDGE('',*,*,#10374,.F.);
#14503=ORIENTED_EDGE('',*,*,#10367,.F.);
#14504=ORIENTED_EDGE('',*,*,#10376,.F.);
#14505=ORIENTED_EDGE('',*,*,#10377,.F.);
#14506=ORIENTED_EDGE('',*,*,#10378,.T.);
#14507=ORIENTED_EDGE('',*,*,#10379,.F.);
#14508=ORIENTED_EDGE('',*,*,#10380,.F.);
#14509=ORIENTED_EDGE('',*,*,#10381,.F.);
#14510=ORIENTED_EDGE('',*,*,#10380,.T.);
#14511=ORIENTED_EDGE('',*,*,#10382,.T.);
#14512=ORIENTED_EDGE('',*,*,#10383,.F.);
#14513=ORIENTED_EDGE('',*,*,#10382,.F.);
#14514=ORIENTED_EDGE('',*,*,#10379,.T.);
#14515=ORIENTED_EDGE('',*,*,#10384,.T.);
#14516=ORIENTED_EDGE('',*,*,#10385,.F.);
#14517=ORIENTED_EDGE('',*,*,#10384,.F.);
#14518=ORIENTED_EDGE('',*,*,#10378,.F.);
#14519=ORIENTED_EDGE('',*,*,#10386,.F.);
#14520=ORIENTED_EDGE('',*,*,#10387,.T.);
#14521=ORIENTED_EDGE('',*,*,#10388,.F.);
#14522=ORIENTED_EDGE('',*,*,#10389,.F.);
#14523=ORIENTED_EDGE('',*,*,#10390,.F.);
#14524=ORIENTED_EDGE('',*,*,#10389,.T.);
#14525=ORIENTED_EDGE('',*,*,#10391,.T.);
#14526=ORIENTED_EDGE('',*,*,#10392,.F.);
#14527=ORIENTED_EDGE('',*,*,#10391,.F.);
#14528=ORIENTED_EDGE('',*,*,#10388,.T.);
#14529=ORIENTED_EDGE('',*,*,#10393,.T.);
#14530=ORIENTED_EDGE('',*,*,#10394,.F.);
#14531=ORIENTED_EDGE('',*,*,#10393,.F.);
#14532=ORIENTED_EDGE('',*,*,#10387,.F.);
#14533=ORIENTED_EDGE('',*,*,#10395,.F.);
#14534=ORIENTED_EDGE('',*,*,#10396,.T.);
#14535=ORIENTED_EDGE('',*,*,#10397,.F.);
#14536=ORIENTED_EDGE('',*,*,#10398,.F.);
#14537=ORIENTED_EDGE('',*,*,#10399,.F.);
#14538=ORIENTED_EDGE('',*,*,#10398,.T.);
#14539=ORIENTED_EDGE('',*,*,#10400,.T.);
#14540=ORIENTED_EDGE('',*,*,#10401,.F.);
#14541=ORIENTED_EDGE('',*,*,#10400,.F.);
#14542=ORIENTED_EDGE('',*,*,#10397,.T.);
#14543=ORIENTED_EDGE('',*,*,#10402,.T.);
#14544=ORIENTED_EDGE('',*,*,#10403,.F.);
#14545=ORIENTED_EDGE('',*,*,#10402,.F.);
#14546=ORIENTED_EDGE('',*,*,#10396,.F.);
#14547=ORIENTED_EDGE('',*,*,#10404,.F.);
#14548=ORIENTED_EDGE('',*,*,#10405,.T.);
#14549=ORIENTED_EDGE('',*,*,#10406,.F.);
#14550=ORIENTED_EDGE('',*,*,#10407,.F.);
#14551=ORIENTED_EDGE('',*,*,#10408,.F.);
#14552=ORIENTED_EDGE('',*,*,#10407,.T.);
#14553=ORIENTED_EDGE('',*,*,#10409,.T.);
#14554=ORIENTED_EDGE('',*,*,#10410,.F.);
#14555=ORIENTED_EDGE('',*,*,#10409,.F.);
#14556=ORIENTED_EDGE('',*,*,#10406,.T.);
#14557=ORIENTED_EDGE('',*,*,#10411,.T.);
#14558=ORIENTED_EDGE('',*,*,#10412,.F.);
#14559=ORIENTED_EDGE('',*,*,#10411,.F.);
#14560=ORIENTED_EDGE('',*,*,#10405,.F.);
#14561=ORIENTED_EDGE('',*,*,#10413,.F.);
#14562=ORIENTED_EDGE('',*,*,#10414,.T.);
#14563=ORIENTED_EDGE('',*,*,#10415,.F.);
#14564=ORIENTED_EDGE('',*,*,#10416,.F.);
#14565=ORIENTED_EDGE('',*,*,#10417,.F.);
#14566=ORIENTED_EDGE('',*,*,#10416,.T.);
#14567=ORIENTED_EDGE('',*,*,#10418,.T.);
#14568=ORIENTED_EDGE('',*,*,#10419,.F.);
#14569=ORIENTED_EDGE('',*,*,#10418,.F.);
#14570=ORIENTED_EDGE('',*,*,#10415,.T.);
#14571=ORIENTED_EDGE('',*,*,#10420,.T.);
#14572=ORIENTED_EDGE('',*,*,#10421,.F.);
#14573=ORIENTED_EDGE('',*,*,#10420,.F.);
#14574=ORIENTED_EDGE('',*,*,#10414,.F.);
#14575=ORIENTED_EDGE('',*,*,#10422,.F.);
#14576=ORIENTED_EDGE('',*,*,#10423,.T.);
#14577=ORIENTED_EDGE('',*,*,#10424,.F.);
#14578=ORIENTED_EDGE('',*,*,#10425,.F.);
#14579=ORIENTED_EDGE('',*,*,#10426,.F.);
#14580=ORIENTED_EDGE('',*,*,#10425,.T.);
#14581=ORIENTED_EDGE('',*,*,#10427,.T.);
#14582=ORIENTED_EDGE('',*,*,#10428,.F.);
#14583=ORIENTED_EDGE('',*,*,#10427,.F.);
#14584=ORIENTED_EDGE('',*,*,#10424,.T.);
#14585=ORIENTED_EDGE('',*,*,#10429,.T.);
#14586=ORIENTED_EDGE('',*,*,#10430,.F.);
#14587=ORIENTED_EDGE('',*,*,#10429,.F.);
#14588=ORIENTED_EDGE('',*,*,#10423,.F.);
#14589=ORIENTED_EDGE('',*,*,#10431,.F.);
#14590=ORIENTED_EDGE('',*,*,#10432,.T.);
#14591=ORIENTED_EDGE('',*,*,#10433,.F.);
#14592=ORIENTED_EDGE('',*,*,#10434,.F.);
#14593=ORIENTED_EDGE('',*,*,#10435,.F.);
#14594=ORIENTED_EDGE('',*,*,#10434,.T.);
#14595=ORIENTED_EDGE('',*,*,#10436,.T.);
#14596=ORIENTED_EDGE('',*,*,#10437,.F.);
#14597=ORIENTED_EDGE('',*,*,#10436,.F.);
#14598=ORIENTED_EDGE('',*,*,#10433,.T.);
#14599=ORIENTED_EDGE('',*,*,#10438,.T.);
#14600=ORIENTED_EDGE('',*,*,#10439,.F.);
#14601=ORIENTED_EDGE('',*,*,#10438,.F.);
#14602=ORIENTED_EDGE('',*,*,#10432,.F.);
#14603=ORIENTED_EDGE('',*,*,#10440,.F.);
#14604=ORIENTED_EDGE('',*,*,#10441,.T.);
#14605=ORIENTED_EDGE('',*,*,#10442,.F.);
#14606=ORIENTED_EDGE('',*,*,#10443,.F.);
#14607=ORIENTED_EDGE('',*,*,#10444,.F.);
#14608=ORIENTED_EDGE('',*,*,#10443,.T.);
#14609=ORIENTED_EDGE('',*,*,#10445,.T.);
#14610=ORIENTED_EDGE('',*,*,#10446,.F.);
#14611=ORIENTED_EDGE('',*,*,#10445,.F.);
#14612=ORIENTED_EDGE('',*,*,#10442,.T.);
#14613=ORIENTED_EDGE('',*,*,#10447,.T.);
#14614=ORIENTED_EDGE('',*,*,#10448,.F.);
#14615=ORIENTED_EDGE('',*,*,#10447,.F.);
#14616=ORIENTED_EDGE('',*,*,#10441,.F.);
#14617=ORIENTED_EDGE('',*,*,#10449,.F.);
#14618=ORIENTED_EDGE('',*,*,#10450,.T.);
#14619=ORIENTED_EDGE('',*,*,#10451,.F.);
#14620=ORIENTED_EDGE('',*,*,#10452,.F.);
#14621=ORIENTED_EDGE('',*,*,#10453,.F.);
#14622=ORIENTED_EDGE('',*,*,#10452,.T.);
#14623=ORIENTED_EDGE('',*,*,#10454,.T.);
#14624=ORIENTED_EDGE('',*,*,#10455,.F.);
#14625=ORIENTED_EDGE('',*,*,#10454,.F.);
#14626=ORIENTED_EDGE('',*,*,#10451,.T.);
#14627=ORIENTED_EDGE('',*,*,#10456,.T.);
#14628=ORIENTED_EDGE('',*,*,#10457,.F.);
#14629=ORIENTED_EDGE('',*,*,#10456,.F.);
#14630=ORIENTED_EDGE('',*,*,#10450,.F.);
#14631=ORIENTED_EDGE('',*,*,#10458,.F.);
#14632=ORIENTED_EDGE('',*,*,#10459,.T.);
#14633=ORIENTED_EDGE('',*,*,#10460,.F.);
#14634=ORIENTED_EDGE('',*,*,#10461,.F.);
#14635=ORIENTED_EDGE('',*,*,#10462,.F.);
#14636=ORIENTED_EDGE('',*,*,#10461,.T.);
#14637=ORIENTED_EDGE('',*,*,#10463,.T.);
#14638=ORIENTED_EDGE('',*,*,#10464,.F.);
#14639=ORIENTED_EDGE('',*,*,#10463,.F.);
#14640=ORIENTED_EDGE('',*,*,#10460,.T.);
#14641=ORIENTED_EDGE('',*,*,#10465,.T.);
#14642=ORIENTED_EDGE('',*,*,#10466,.F.);
#14643=ORIENTED_EDGE('',*,*,#10465,.F.);
#14644=ORIENTED_EDGE('',*,*,#10459,.F.);
#14645=ORIENTED_EDGE('',*,*,#10467,.F.);
#14646=ORIENTED_EDGE('',*,*,#10468,.T.);
#14647=ORIENTED_EDGE('',*,*,#10469,.F.);
#14648=ORIENTED_EDGE('',*,*,#10470,.F.);
#14649=ORIENTED_EDGE('',*,*,#10471,.F.);
#14650=ORIENTED_EDGE('',*,*,#10470,.T.);
#14651=ORIENTED_EDGE('',*,*,#10472,.T.);
#14652=ORIENTED_EDGE('',*,*,#10473,.F.);
#14653=ORIENTED_EDGE('',*,*,#10472,.F.);
#14654=ORIENTED_EDGE('',*,*,#10469,.T.);
#14655=ORIENTED_EDGE('',*,*,#10474,.T.);
#14656=ORIENTED_EDGE('',*,*,#10475,.F.);
#14657=ORIENTED_EDGE('',*,*,#10474,.F.);
#14658=ORIENTED_EDGE('',*,*,#10468,.F.);
#14659=ORIENTED_EDGE('',*,*,#10476,.F.);
#14660=ORIENTED_EDGE('',*,*,#10477,.T.);
#14661=ORIENTED_EDGE('',*,*,#10478,.F.);
#14662=ORIENTED_EDGE('',*,*,#10479,.F.);
#14663=ORIENTED_EDGE('',*,*,#10480,.F.);
#14664=ORIENTED_EDGE('',*,*,#10479,.T.);
#14665=ORIENTED_EDGE('',*,*,#10481,.T.);
#14666=ORIENTED_EDGE('',*,*,#10482,.F.);
#14667=ORIENTED_EDGE('',*,*,#10481,.F.);
#14668=ORIENTED_EDGE('',*,*,#10478,.T.);
#14669=ORIENTED_EDGE('',*,*,#10483,.T.);
#14670=ORIENTED_EDGE('',*,*,#10484,.F.);
#14671=ORIENTED_EDGE('',*,*,#10483,.F.);
#14672=ORIENTED_EDGE('',*,*,#10477,.F.);
#14673=ORIENTED_EDGE('',*,*,#10485,.F.);
#14674=ORIENTED_EDGE('',*,*,#10486,.T.);
#14675=ORIENTED_EDGE('',*,*,#10487,.F.);
#14676=ORIENTED_EDGE('',*,*,#10488,.F.);
#14677=ORIENTED_EDGE('',*,*,#10489,.F.);
#14678=ORIENTED_EDGE('',*,*,#10488,.T.);
#14679=ORIENTED_EDGE('',*,*,#10490,.T.);
#14680=ORIENTED_EDGE('',*,*,#10491,.F.);
#14681=ORIENTED_EDGE('',*,*,#10490,.F.);
#14682=ORIENTED_EDGE('',*,*,#10487,.T.);
#14683=ORIENTED_EDGE('',*,*,#10492,.T.);
#14684=ORIENTED_EDGE('',*,*,#10493,.F.);
#14685=ORIENTED_EDGE('',*,*,#10492,.F.);
#14686=ORIENTED_EDGE('',*,*,#10486,.F.);
#14687=ORIENTED_EDGE('',*,*,#10494,.F.);
#14688=ORIENTED_EDGE('',*,*,#10495,.T.);
#14689=ORIENTED_EDGE('',*,*,#10496,.F.);
#14690=ORIENTED_EDGE('',*,*,#10497,.F.);
#14691=ORIENTED_EDGE('',*,*,#10498,.F.);
#14692=ORIENTED_EDGE('',*,*,#10497,.T.);
#14693=ORIENTED_EDGE('',*,*,#10499,.T.);
#14694=ORIENTED_EDGE('',*,*,#10500,.F.);
#14695=ORIENTED_EDGE('',*,*,#10499,.F.);
#14696=ORIENTED_EDGE('',*,*,#10496,.T.);
#14697=ORIENTED_EDGE('',*,*,#10501,.T.);
#14698=ORIENTED_EDGE('',*,*,#10502,.F.);
#14699=ORIENTED_EDGE('',*,*,#10501,.F.);
#14700=ORIENTED_EDGE('',*,*,#10495,.F.);
#14701=ORIENTED_EDGE('',*,*,#10503,.F.);
#14702=ORIENTED_EDGE('',*,*,#10504,.T.);
#14703=ORIENTED_EDGE('',*,*,#10505,.F.);
#14704=ORIENTED_EDGE('',*,*,#10506,.F.);
#14705=ORIENTED_EDGE('',*,*,#10507,.F.);
#14706=ORIENTED_EDGE('',*,*,#10506,.T.);
#14707=ORIENTED_EDGE('',*,*,#10508,.T.);
#14708=ORIENTED_EDGE('',*,*,#10509,.F.);
#14709=ORIENTED_EDGE('',*,*,#10508,.F.);
#14710=ORIENTED_EDGE('',*,*,#10505,.T.);
#14711=ORIENTED_EDGE('',*,*,#10510,.T.);
#14712=ORIENTED_EDGE('',*,*,#10511,.F.);
#14713=ORIENTED_EDGE('',*,*,#10510,.F.);
#14714=ORIENTED_EDGE('',*,*,#10504,.F.);
#14715=ORIENTED_EDGE('',*,*,#10512,.F.);
#14716=ORIENTED_EDGE('',*,*,#10513,.F.);
#14717=ORIENTED_EDGE('',*,*,#10514,.T.);
#14718=ORIENTED_EDGE('',*,*,#10512,.T.);
#14719=ORIENTED_EDGE('',*,*,#10514,.F.);
#14720=ORIENTED_EDGE('',*,*,#10069,.F.);
#14721=ORIENTED_EDGE('',*,*,#9990,.F.);
#14722=ORIENTED_EDGE('',*,*,#10070,.F.);
#14723=ORIENTED_EDGE('',*,*,#10515,.T.);
#14724=ORIENTED_EDGE('',*,*,#10513,.T.);
#14725=ORIENTED_EDGE('',*,*,#10515,.F.);
#14726=ORIENTED_EDGE('',*,*,#10025,.T.);
#14727=ORIENTED_EDGE('',*,*,#10066,.T.);
#14728=ORIENTED_EDGE('',*,*,#10076,.F.);
#14729=ORIENTED_EDGE('',*,*,#10075,.T.);
#14730=ORIENTED_EDGE('',*,*,#10516,.F.);
#14731=ORIENTED_EDGE('',*,*,#10517,.T.);
#14732=ORIENTED_EDGE('',*,*,#10077,.T.);
#14733=ORIENTED_EDGE('',*,*,#10517,.F.);
#14734=ORIENTED_EDGE('',*,*,#10518,.F.);
#14735=ORIENTED_EDGE('',*,*,#10516,.T.);
#14736=ORIENTED_EDGE('',*,*,#10519,.F.);
#14737=ORIENTED_EDGE('',*,*,#10520,.T.);
#14738=ORIENTED_EDGE('',*,*,#10518,.T.);
#14739=ORIENTED_EDGE('',*,*,#10520,.F.);
#14740=ORIENTED_EDGE('',*,*,#10521,.F.);
#14741=ORIENTED_EDGE('',*,*,#10522,.T.);
#14742=ORIENTED_EDGE('',*,*,#10376,.T.);
#14743=ORIENTED_EDGE('',*,*,#10366,.T.);
#14744=ORIENTED_EDGE('',*,*,#10370,.T.);
#14745=ORIENTED_EDGE('',*,*,#10523,.T.);
#14746=ORIENTED_EDGE('',*,*,#10519,.T.);
#14747=ORIENTED_EDGE('',*,*,#10523,.F.);
#14748=ORIENTED_EDGE('',*,*,#10372,.T.);
#14749=ORIENTED_EDGE('',*,*,#10373,.T.);
#14750=ORIENTED_EDGE('',*,*,#10375,.T.);
#14751=ORIENTED_EDGE('',*,*,#10522,.F.);
#14752=ORIENTED_EDGE('',*,*,#10246,.T.);
#14753=ORIENTED_EDGE('',*,*,#10248,.T.);
#14754=ORIENTED_EDGE('',*,*,#10240,.T.);
#14755=ORIENTED_EDGE('',*,*,#10244,.T.);
#14756=ORIENTED_EDGE('',*,*,#10255,.T.);
#14757=ORIENTED_EDGE('',*,*,#10257,.T.);
#14758=ORIENTED_EDGE('',*,*,#10249,.T.);
#14759=ORIENTED_EDGE('',*,*,#10253,.T.);
#14760=ORIENTED_EDGE('',*,*,#10264,.T.);
#14761=ORIENTED_EDGE('',*,*,#10266,.T.);
#14762=ORIENTED_EDGE('',*,*,#10258,.T.);
#14763=ORIENTED_EDGE('',*,*,#10262,.T.);
#14764=ORIENTED_EDGE('',*,*,#10273,.T.);
#14765=ORIENTED_EDGE('',*,*,#10275,.T.);
#14766=ORIENTED_EDGE('',*,*,#10267,.T.);
#14767=ORIENTED_EDGE('',*,*,#10271,.T.);
#14768=ORIENTED_EDGE('',*,*,#10282,.T.);
#14769=ORIENTED_EDGE('',*,*,#10284,.T.);
#14770=ORIENTED_EDGE('',*,*,#10276,.T.);
#14771=ORIENTED_EDGE('',*,*,#10280,.T.);
#14772=ORIENTED_EDGE('',*,*,#10291,.T.);
#14773=ORIENTED_EDGE('',*,*,#10293,.T.);
#14774=ORIENTED_EDGE('',*,*,#10285,.T.);
#14775=ORIENTED_EDGE('',*,*,#10289,.T.);
#14776=ORIENTED_EDGE('',*,*,#10300,.T.);
#14777=ORIENTED_EDGE('',*,*,#10302,.T.);
#14778=ORIENTED_EDGE('',*,*,#10294,.T.);
#14779=ORIENTED_EDGE('',*,*,#10298,.T.);
#14780=ORIENTED_EDGE('',*,*,#10309,.T.);
#14781=ORIENTED_EDGE('',*,*,#10311,.T.);
#14782=ORIENTED_EDGE('',*,*,#10303,.T.);
#14783=ORIENTED_EDGE('',*,*,#10307,.T.);
#14784=ORIENTED_EDGE('',*,*,#10318,.T.);
#14785=ORIENTED_EDGE('',*,*,#10320,.T.);
#14786=ORIENTED_EDGE('',*,*,#10312,.T.);
#14787=ORIENTED_EDGE('',*,*,#10316,.T.);
#14788=ORIENTED_EDGE('',*,*,#10327,.T.);
#14789=ORIENTED_EDGE('',*,*,#10329,.T.);
#14790=ORIENTED_EDGE('',*,*,#10321,.T.);
#14791=ORIENTED_EDGE('',*,*,#10325,.T.);
#14792=ORIENTED_EDGE('',*,*,#10336,.T.);
#14793=ORIENTED_EDGE('',*,*,#10338,.T.);
#14794=ORIENTED_EDGE('',*,*,#10330,.T.);
#14795=ORIENTED_EDGE('',*,*,#10334,.T.);
#14796=ORIENTED_EDGE('',*,*,#10345,.T.);
#14797=ORIENTED_EDGE('',*,*,#10347,.T.);
#14798=ORIENTED_EDGE('',*,*,#10339,.T.);
#14799=ORIENTED_EDGE('',*,*,#10343,.T.);
#14800=ORIENTED_EDGE('',*,*,#10354,.T.);
#14801=ORIENTED_EDGE('',*,*,#10356,.T.);
#14802=ORIENTED_EDGE('',*,*,#10348,.T.);
#14803=ORIENTED_EDGE('',*,*,#10352,.T.);
#14804=ORIENTED_EDGE('',*,*,#10363,.T.);
#14805=ORIENTED_EDGE('',*,*,#10365,.T.);
#14806=ORIENTED_EDGE('',*,*,#10357,.T.);
#14807=ORIENTED_EDGE('',*,*,#10361,.T.);
#14808=ORIENTED_EDGE('',*,*,#10383,.T.);
#14809=ORIENTED_EDGE('',*,*,#10385,.T.);
#14810=ORIENTED_EDGE('',*,*,#10377,.T.);
#14811=ORIENTED_EDGE('',*,*,#10381,.T.);
#14812=ORIENTED_EDGE('',*,*,#10392,.T.);
#14813=ORIENTED_EDGE('',*,*,#10394,.T.);
#14814=ORIENTED_EDGE('',*,*,#10386,.T.);
#14815=ORIENTED_EDGE('',*,*,#10390,.T.);
#14816=ORIENTED_EDGE('',*,*,#10401,.T.);
#14817=ORIENTED_EDGE('',*,*,#10403,.T.);
#14818=ORIENTED_EDGE('',*,*,#10395,.T.);
#14819=ORIENTED_EDGE('',*,*,#10399,.T.);
#14820=ORIENTED_EDGE('',*,*,#10410,.T.);
#14821=ORIENTED_EDGE('',*,*,#10412,.T.);
#14822=ORIENTED_EDGE('',*,*,#10404,.T.);
#14823=ORIENTED_EDGE('',*,*,#10408,.T.);
#14824=ORIENTED_EDGE('',*,*,#10419,.T.);
#14825=ORIENTED_EDGE('',*,*,#10421,.T.);
#14826=ORIENTED_EDGE('',*,*,#10413,.T.);
#14827=ORIENTED_EDGE('',*,*,#10417,.T.);
#14828=ORIENTED_EDGE('',*,*,#10428,.T.);
#14829=ORIENTED_EDGE('',*,*,#10430,.T.);
#14830=ORIENTED_EDGE('',*,*,#10422,.T.);
#14831=ORIENTED_EDGE('',*,*,#10426,.T.);
#14832=ORIENTED_EDGE('',*,*,#10437,.T.);
#14833=ORIENTED_EDGE('',*,*,#10439,.T.);
#14834=ORIENTED_EDGE('',*,*,#10431,.T.);
#14835=ORIENTED_EDGE('',*,*,#10435,.T.);
#14836=ORIENTED_EDGE('',*,*,#10446,.T.);
#14837=ORIENTED_EDGE('',*,*,#10448,.T.);
#14838=ORIENTED_EDGE('',*,*,#10440,.T.);
#14839=ORIENTED_EDGE('',*,*,#10444,.T.);
#14840=ORIENTED_EDGE('',*,*,#10455,.T.);
#14841=ORIENTED_EDGE('',*,*,#10457,.T.);
#14842=ORIENTED_EDGE('',*,*,#10449,.T.);
#14843=ORIENTED_EDGE('',*,*,#10453,.T.);
#14844=ORIENTED_EDGE('',*,*,#10464,.T.);
#14845=ORIENTED_EDGE('',*,*,#10466,.T.);
#14846=ORIENTED_EDGE('',*,*,#10458,.T.);
#14847=ORIENTED_EDGE('',*,*,#10462,.T.);
#14848=ORIENTED_EDGE('',*,*,#10473,.T.);
#14849=ORIENTED_EDGE('',*,*,#10475,.T.);
#14850=ORIENTED_EDGE('',*,*,#10467,.T.);
#14851=ORIENTED_EDGE('',*,*,#10471,.T.);
#14852=ORIENTED_EDGE('',*,*,#10482,.T.);
#14853=ORIENTED_EDGE('',*,*,#10484,.T.);
#14854=ORIENTED_EDGE('',*,*,#10476,.T.);
#14855=ORIENTED_EDGE('',*,*,#10480,.T.);
#14856=ORIENTED_EDGE('',*,*,#10491,.T.);
#14857=ORIENTED_EDGE('',*,*,#10493,.T.);
#14858=ORIENTED_EDGE('',*,*,#10485,.T.);
#14859=ORIENTED_EDGE('',*,*,#10489,.T.);
#14860=ORIENTED_EDGE('',*,*,#10500,.T.);
#14861=ORIENTED_EDGE('',*,*,#10502,.T.);
#14862=ORIENTED_EDGE('',*,*,#10494,.T.);
#14863=ORIENTED_EDGE('',*,*,#10498,.T.);
#14864=ORIENTED_EDGE('',*,*,#10509,.T.);
#14865=ORIENTED_EDGE('',*,*,#10511,.T.);
#14866=ORIENTED_EDGE('',*,*,#10503,.T.);
#14867=ORIENTED_EDGE('',*,*,#10507,.T.);
#14868=ORIENTED_EDGE('',*,*,#10524,.F.);
#14869=ORIENTED_EDGE('',*,*,#10525,.T.);
#14870=ORIENTED_EDGE('',*,*,#10521,.T.);
#14871=ORIENTED_EDGE('',*,*,#10525,.F.);
#14872=ORIENTED_EDGE('',*,*,#10524,.T.);
#14873=ORIENTED_EDGE('',*,*,#10078,.T.);
#14874=ORIENTED_EDGE('',*,*,#10109,.T.);
#14875=ORIENTED_EDGE('',*,*,#10106,.T.);
#14876=ORIENTED_EDGE('',*,*,#10103,.T.);
#14877=ORIENTED_EDGE('',*,*,#10100,.T.);
#14878=ORIENTED_EDGE('',*,*,#10097,.T.);
#14879=ORIENTED_EDGE('',*,*,#10094,.T.);
#14880=ORIENTED_EDGE('',*,*,#10091,.T.);
#14881=ORIENTED_EDGE('',*,*,#10088,.T.);
#14882=ORIENTED_EDGE('',*,*,#10085,.T.);
#14883=ORIENTED_EDGE('',*,*,#10082,.T.);
#14884=ORIENTED_EDGE('',*,*,#10111,.T.);
#14885=ORIENTED_EDGE('',*,*,#10139,.T.);
#14886=ORIENTED_EDGE('',*,*,#10136,.T.);
#14887=ORIENTED_EDGE('',*,*,#10133,.T.);
#14888=ORIENTED_EDGE('',*,*,#10130,.T.);
#14889=ORIENTED_EDGE('',*,*,#10127,.T.);
#14890=ORIENTED_EDGE('',*,*,#10124,.T.);
#14891=ORIENTED_EDGE('',*,*,#10121,.T.);
#14892=ORIENTED_EDGE('',*,*,#10118,.T.);
#14893=ORIENTED_EDGE('',*,*,#10115,.T.);
#14894=ORIENTED_EDGE('',*,*,#10141,.T.);
#14895=ORIENTED_EDGE('',*,*,#10172,.T.);
#14896=ORIENTED_EDGE('',*,*,#10169,.T.);
#14897=ORIENTED_EDGE('',*,*,#10166,.T.);
#14898=ORIENTED_EDGE('',*,*,#10163,.T.);
#14899=ORIENTED_EDGE('',*,*,#10160,.T.);
#14900=ORIENTED_EDGE('',*,*,#10157,.T.);
#14901=ORIENTED_EDGE('',*,*,#10154,.T.);
#14902=ORIENTED_EDGE('',*,*,#10151,.T.);
#14903=ORIENTED_EDGE('',*,*,#10148,.T.);
#14904=ORIENTED_EDGE('',*,*,#10145,.T.);
#14905=ORIENTED_EDGE('',*,*,#10174,.T.);
#14906=ORIENTED_EDGE('',*,*,#10202,.T.);
#14907=ORIENTED_EDGE('',*,*,#10199,.T.);
#14908=ORIENTED_EDGE('',*,*,#10196,.T.);
#14909=ORIENTED_EDGE('',*,*,#10193,.T.);
#14910=ORIENTED_EDGE('',*,*,#10190,.T.);
#14911=ORIENTED_EDGE('',*,*,#10187,.T.);
#14912=ORIENTED_EDGE('',*,*,#10184,.T.);
#14913=ORIENTED_EDGE('',*,*,#10181,.T.);
#14914=ORIENTED_EDGE('',*,*,#10178,.T.);
#14915=ORIENTED_EDGE('',*,*,#10204,.T.);
#14916=ORIENTED_EDGE('',*,*,#10232,.T.);
#14917=ORIENTED_EDGE('',*,*,#10229,.T.);
#14918=ORIENTED_EDGE('',*,*,#10226,.T.);
#14919=ORIENTED_EDGE('',*,*,#10223,.T.);
#14920=ORIENTED_EDGE('',*,*,#10220,.T.);
#14921=ORIENTED_EDGE('',*,*,#10217,.T.);
#14922=ORIENTED_EDGE('',*,*,#10214,.T.);
#14923=ORIENTED_EDGE('',*,*,#10211,.T.);
#14924=ORIENTED_EDGE('',*,*,#10208,.T.);
#14925=ORIENTED_EDGE('',*,*,#10237,.T.);
#14926=ORIENTED_EDGE('',*,*,#10526,.T.);
#14927=ORIENTED_EDGE('',*,*,#10527,.T.);
#14928=ORIENTED_EDGE('',*,*,#10528,.T.);
#14929=ORIENTED_EDGE('',*,*,#10529,.T.);
#14930=ORIENTED_EDGE('',*,*,#10527,.F.);
#14931=ORIENTED_EDGE('',*,*,#10530,.F.);
#14932=ORIENTED_EDGE('',*,*,#10531,.F.);
#14933=ORIENTED_EDGE('',*,*,#10532,.F.);
#14934=ORIENTED_EDGE('',*,*,#10533,.T.);
#14935=ORIENTED_EDGE('',*,*,#10534,.T.);
#14936=ORIENTED_EDGE('',*,*,#10535,.T.);
#14937=ORIENTED_EDGE('',*,*,#10536,.T.);
#14938=ORIENTED_EDGE('',*,*,#10534,.F.);
#14939=ORIENTED_EDGE('',*,*,#10537,.F.);
#14940=ORIENTED_EDGE('',*,*,#10538,.T.);
#14941=ORIENTED_EDGE('',*,*,#10539,.F.);
#14942=ORIENTED_EDGE('',*,*,#10540,.T.);
#14943=ORIENTED_EDGE('',*,*,#10541,.T.);
#14944=ORIENTED_EDGE('',*,*,#10542,.T.);
#14945=ORIENTED_EDGE('',*,*,#10543,.T.);
#14946=ORIENTED_EDGE('',*,*,#10544,.T.);
#14947=ORIENTED_EDGE('',*,*,#10545,.T.);
#14948=ORIENTED_EDGE('',*,*,#10546,.T.);
#14949=ORIENTED_EDGE('',*,*,#10547,.T.);
#14950=ORIENTED_EDGE('',*,*,#10544,.F.);
#14951=ORIENTED_EDGE('',*,*,#10548,.T.);
#14952=ORIENTED_EDGE('',*,*,#10549,.T.);
#14953=ORIENTED_EDGE('',*,*,#10546,.F.);
#14954=ORIENTED_EDGE('',*,*,#10550,.T.);
#14955=ORIENTED_EDGE('',*,*,#10551,.T.);
#14956=ORIENTED_EDGE('',*,*,#10548,.F.);
#14957=ORIENTED_EDGE('',*,*,#10552,.T.);
#14958=ORIENTED_EDGE('',*,*,#10540,.F.);
#14959=ORIENTED_EDGE('',*,*,#10547,.F.);
#14960=ORIENTED_EDGE('',*,*,#10549,.F.);
#14961=ORIENTED_EDGE('',*,*,#10530,.T.);
#14962=ORIENTED_EDGE('',*,*,#10526,.F.);
#14963=ORIENTED_EDGE('',*,*,#10553,.T.);
#14964=ORIENTED_EDGE('',*,*,#10537,.T.);
#14965=ORIENTED_EDGE('',*,*,#10533,.F.);
#14966=ORIENTED_EDGE('',*,*,#10554,.T.);
#14967=ORIENTED_EDGE('',*,*,#10555,.T.);
#14968=ORIENTED_EDGE('',*,*,#10556,.T.);
#14969=ORIENTED_EDGE('',*,*,#10557,.T.);
#14970=ORIENTED_EDGE('',*,*,#10558,.T.);
#14971=ORIENTED_EDGE('',*,*,#10559,.F.);
#14972=ORIENTED_EDGE('',*,*,#10560,.T.);
#14973=ORIENTED_EDGE('',*,*,#10561,.T.);
#14974=ORIENTED_EDGE('',*,*,#10562,.F.);
#14975=ORIENTED_EDGE('',*,*,#10563,.T.);
#14976=ORIENTED_EDGE('',*,*,#10564,.T.);
#14977=ORIENTED_EDGE('',*,*,#10564,.F.);
#14978=ORIENTED_EDGE('',*,*,#10565,.T.);
#14979=ORIENTED_EDGE('',*,*,#10566,.T.);
#14980=ORIENTED_EDGE('',*,*,#10567,.T.);
#14981=ORIENTED_EDGE('',*,*,#10568,.T.);
#14982=ORIENTED_EDGE('',*,*,#10566,.F.);
#14983=ORIENTED_EDGE('',*,*,#10569,.T.);
#14984=ORIENTED_EDGE('',*,*,#10561,.F.);
#14985=ORIENTED_EDGE('',*,*,#10570,.T.);
#14986=ORIENTED_EDGE('',*,*,#10558,.F.);
#14987=ORIENTED_EDGE('',*,*,#10571,.T.);
#14988=ORIENTED_EDGE('',*,*,#10572,.F.);
#14989=ORIENTED_EDGE('',*,*,#10573,.T.);
#14990=ORIENTED_EDGE('',*,*,#10574,.T.);
#14991=ORIENTED_EDGE('',*,*,#10557,.F.);
#14992=ORIENTED_EDGE('',*,*,#10575,.T.);
#14993=ORIENTED_EDGE('',*,*,#10576,.F.);
#14994=ORIENTED_EDGE('',*,*,#10571,.F.);
#14995=ORIENTED_EDGE('',*,*,#10569,.F.);
#14996=ORIENTED_EDGE('',*,*,#10577,.T.);
#14997=ORIENTED_EDGE('',*,*,#10578,.F.);
#14998=ORIENTED_EDGE('',*,*,#10575,.F.);
#14999=ORIENTED_EDGE('',*,*,#10565,.F.);
#15000=ORIENTED_EDGE('',*,*,#10579,.T.);
#15001=ORIENTED_EDGE('',*,*,#10580,.F.);
#15002=ORIENTED_EDGE('',*,*,#10577,.F.);
#15003=ORIENTED_EDGE('',*,*,#10552,.F.);
#15004=ORIENTED_EDGE('',*,*,#10581,.T.);
#15005=ORIENTED_EDGE('',*,*,#10582,.F.);
#15006=ORIENTED_EDGE('',*,*,#10583,.F.);
#15007=ORIENTED_EDGE('',*,*,#10584,.F.);
#15008=ORIENTED_EDGE('',*,*,#10579,.F.);
#15009=ORIENTED_EDGE('',*,*,#10563,.F.);
#15010=ORIENTED_EDGE('',*,*,#10585,.F.);
#15011=ORIENTED_EDGE('',*,*,#10531,.T.);
#15012=ORIENTED_EDGE('',*,*,#10551,.F.);
#15013=ORIENTED_EDGE('',*,*,#10585,.T.);
#15014=ORIENTED_EDGE('',*,*,#10562,.T.);
#15015=ORIENTED_EDGE('',*,*,#10586,.T.);
#15016=ORIENTED_EDGE('',*,*,#10587,.F.);
#15017=ORIENTED_EDGE('',*,*,#10588,.T.);
#15018=ORIENTED_EDGE('',*,*,#10589,.T.);
#15019=ORIENTED_EDGE('',*,*,#10587,.T.);
#15020=ORIENTED_EDGE('',*,*,#10590,.T.);
#15021=ORIENTED_EDGE('',*,*,#10591,.T.);
#15022=ORIENTED_EDGE('',*,*,#10592,.T.);
#15023=ORIENTED_EDGE('',*,*,#10593,.T.);
#15024=ORIENTED_EDGE('',*,*,#10594,.F.);
#15025=ORIENTED_EDGE('',*,*,#10595,.T.);
#15026=ORIENTED_EDGE('',*,*,#10591,.F.);
#15027=ORIENTED_EDGE('',*,*,#10596,.T.);
#15028=ORIENTED_EDGE('',*,*,#10542,.F.);
#15029=ORIENTED_EDGE('',*,*,#10589,.F.);
#15030=ORIENTED_EDGE('',*,*,#10597,.F.);
#15031=ORIENTED_EDGE('',*,*,#10598,.F.);
#15032=ORIENTED_EDGE('',*,*,#10599,.F.);
#15033=ORIENTED_EDGE('',*,*,#10600,.F.);
#15034=ORIENTED_EDGE('',*,*,#10601,.F.);
#15035=ORIENTED_EDGE('',*,*,#10602,.F.);
#15036=ORIENTED_EDGE('',*,*,#10603,.T.);
#15037=ORIENTED_EDGE('',*,*,#10604,.T.);
#15038=ORIENTED_EDGE('',*,*,#10588,.F.);
#15039=ORIENTED_EDGE('',*,*,#10592,.F.);
#15040=ORIENTED_EDGE('',*,*,#10605,.T.);
#15041=ORIENTED_EDGE('',*,*,#10606,.F.);
#15042=ORIENTED_EDGE('',*,*,#10607,.F.);
#15043=ORIENTED_EDGE('',*,*,#10597,.T.);
#15044=ORIENTED_EDGE('',*,*,#10595,.F.);
#15045=ORIENTED_EDGE('',*,*,#10608,.T.);
#15046=ORIENTED_EDGE('',*,*,#10609,.T.);
#15047=ORIENTED_EDGE('',*,*,#10573,.F.);
#15048=ORIENTED_EDGE('',*,*,#10610,.F.);
#15049=ORIENTED_EDGE('',*,*,#10611,.F.);
#15050=ORIENTED_EDGE('',*,*,#10605,.F.);
#15051=ORIENTED_EDGE('',*,*,#10612,.T.);
#15052=ORIENTED_EDGE('',*,*,#10613,.F.);
#15053=ORIENTED_EDGE('',*,*,#10614,.T.);
#15054=ORIENTED_EDGE('',*,*,#10615,.T.);
#15055=ORIENTED_EDGE('',*,*,#10613,.T.);
#15056=ORIENTED_EDGE('',*,*,#10616,.T.);
#15057=ORIENTED_EDGE('',*,*,#10572,.T.);
#15058=ORIENTED_EDGE('',*,*,#10617,.T.);
#15059=ORIENTED_EDGE('',*,*,#10614,.F.);
#15060=ORIENTED_EDGE('',*,*,#10617,.F.);
#15061=ORIENTED_EDGE('',*,*,#10576,.T.);
#15062=ORIENTED_EDGE('',*,*,#10618,.F.);
#15063=ORIENTED_EDGE('',*,*,#10619,.T.);
#15064=ORIENTED_EDGE('',*,*,#10560,.F.);
#15065=ORIENTED_EDGE('',*,*,#10620,.T.);
#15066=ORIENTED_EDGE('',*,*,#10535,.F.);
#15067=ORIENTED_EDGE('',*,*,#10539,.T.);
#15068=ORIENTED_EDGE('',*,*,#10621,.T.);
#15069=ORIENTED_EDGE('',*,*,#10528,.F.);
#15070=ORIENTED_EDGE('',*,*,#10532,.T.);
#15071=ORIENTED_EDGE('',*,*,#10567,.F.);
#15072=ORIENTED_EDGE('',*,*,#10568,.F.);
#15073=ORIENTED_EDGE('',*,*,#10622,.T.);
#15074=ORIENTED_EDGE('',*,*,#10623,.T.);
#15075=ORIENTED_EDGE('',*,*,#10536,.F.);
#15076=ORIENTED_EDGE('',*,*,#10620,.F.);
#15077=ORIENTED_EDGE('',*,*,#10559,.T.);
#15078=ORIENTED_EDGE('',*,*,#10570,.F.);
#15079=ORIENTED_EDGE('',*,*,#10624,.T.);
#15080=ORIENTED_EDGE('',*,*,#10625,.T.);
#15081=ORIENTED_EDGE('',*,*,#10626,.T.);
#15082=ORIENTED_EDGE('',*,*,#10593,.F.);
#15083=ORIENTED_EDGE('',*,*,#10541,.F.);
#15084=ORIENTED_EDGE('',*,*,#10554,.F.);
#15085=ORIENTED_EDGE('',*,*,#10607,.T.);
#15086=ORIENTED_EDGE('',*,*,#10627,.F.);
#15087=ORIENTED_EDGE('',*,*,#10628,.T.);
#15088=ORIENTED_EDGE('',*,*,#10598,.T.);
#15089=ORIENTED_EDGE('',*,*,#10629,.T.);
#15090=ORIENTED_EDGE('',*,*,#10630,.F.);
#15091=ORIENTED_EDGE('',*,*,#10631,.T.);
#15092=ORIENTED_EDGE('',*,*,#10632,.T.);
#15093=ORIENTED_EDGE('',*,*,#10630,.T.);
#15094=ORIENTED_EDGE('',*,*,#10633,.T.);
#15095=ORIENTED_EDGE('',*,*,#10634,.T.);
#15096=ORIENTED_EDGE('',*,*,#10635,.T.);
#15097=ORIENTED_EDGE('',*,*,#10634,.F.);
#15098=ORIENTED_EDGE('',*,*,#10583,.T.);
#15099=ORIENTED_EDGE('',*,*,#10636,.T.);
#15100=ORIENTED_EDGE('',*,*,#10611,.T.);
#15101=ORIENTED_EDGE('',*,*,#10627,.T.);
#15102=ORIENTED_EDGE('',*,*,#10606,.T.);
#15103=ORIENTED_EDGE('',*,*,#10636,.F.);
#15104=ORIENTED_EDGE('',*,*,#10637,.T.);
#15105=ORIENTED_EDGE('',*,*,#10628,.F.);
#15106=ORIENTED_EDGE('',*,*,#10637,.F.);
#15107=ORIENTED_EDGE('',*,*,#10582,.T.);
#15108=ORIENTED_EDGE('',*,*,#10638,.T.);
#15109=ORIENTED_EDGE('',*,*,#10599,.T.);
#15110=ORIENTED_EDGE('',*,*,#10633,.F.);
#15111=ORIENTED_EDGE('',*,*,#10629,.F.);
#15112=ORIENTED_EDGE('',*,*,#10639,.T.);
#15113=ORIENTED_EDGE('',*,*,#10640,.F.);
#15114=ORIENTED_EDGE('',*,*,#10584,.T.);
#15115=ORIENTED_EDGE('',*,*,#10612,.F.);
#15116=ORIENTED_EDGE('',*,*,#10641,.T.);
#15117=ORIENTED_EDGE('',*,*,#10631,.F.);
#15118=ORIENTED_EDGE('',*,*,#10635,.F.);
#15119=ORIENTED_EDGE('',*,*,#10610,.T.);
#15120=ORIENTED_EDGE('',*,*,#10616,.F.);
#15121=ORIENTED_EDGE('',*,*,#10578,.T.);
#15122=ORIENTED_EDGE('',*,*,#10642,.T.);
#15123=ORIENTED_EDGE('',*,*,#10643,.T.);
#15124=ORIENTED_EDGE('',*,*,#10618,.T.);
#15125=ORIENTED_EDGE('',*,*,#10640,.T.);
#15126=ORIENTED_EDGE('',*,*,#10644,.T.);
#15127=ORIENTED_EDGE('',*,*,#10642,.F.);
#15128=ORIENTED_EDGE('',*,*,#10580,.T.);
#15129=ORIENTED_EDGE('',*,*,#10615,.F.);
#15130=ORIENTED_EDGE('',*,*,#10619,.F.);
#15131=ORIENTED_EDGE('',*,*,#10643,.F.);
#15132=ORIENTED_EDGE('',*,*,#10644,.F.);
#15133=ORIENTED_EDGE('',*,*,#10639,.F.);
#15134=ORIENTED_EDGE('',*,*,#10632,.F.);
#15135=ORIENTED_EDGE('',*,*,#10641,.F.);
#15136=ORIENTED_EDGE('',*,*,#10645,.T.);
#15137=ORIENTED_EDGE('',*,*,#10646,.T.);
#15138=ORIENTED_EDGE('',*,*,#10586,.F.);
#15139=ORIENTED_EDGE('',*,*,#10602,.T.);
#15140=ORIENTED_EDGE('',*,*,#10647,.T.);
#15141=ORIENTED_EDGE('',*,*,#10648,.T.);
#15142=ORIENTED_EDGE('',*,*,#10590,.F.);
#15143=ORIENTED_EDGE('',*,*,#10649,.T.);
#15144=ORIENTED_EDGE('',*,*,#10600,.T.);
#15145=ORIENTED_EDGE('',*,*,#10638,.F.);
#15146=ORIENTED_EDGE('',*,*,#10650,.T.);
#15147=ORIENTED_EDGE('',*,*,#10601,.T.);
#15148=ORIENTED_EDGE('',*,*,#10649,.F.);
#15149=ORIENTED_EDGE('',*,*,#10651,.T.);
#15150=ORIENTED_EDGE('',*,*,#10647,.F.);
#15151=ORIENTED_EDGE('',*,*,#10545,.F.);
#15152=ORIENTED_EDGE('',*,*,#10652,.T.);
#15153=ORIENTED_EDGE('',*,*,#10651,.F.);
#15154=ORIENTED_EDGE('',*,*,#10653,.F.);
#15155=ORIENTED_EDGE('',*,*,#10550,.F.);
#15156=ORIENTED_EDGE('',*,*,#10653,.T.);
#15157=ORIENTED_EDGE('',*,*,#10650,.F.);
#15158=ORIENTED_EDGE('',*,*,#10581,.F.);
#15159=ORIENTED_EDGE('',*,*,#10623,.F.);
#15160=ORIENTED_EDGE('',*,*,#10654,.T.);
#15161=ORIENTED_EDGE('',*,*,#10646,.F.);
#15162=ORIENTED_EDGE('',*,*,#10654,.F.);
#15163=ORIENTED_EDGE('',*,*,#10604,.F.);
#15164=ORIENTED_EDGE('',*,*,#10655,.T.);
#15165=ORIENTED_EDGE('',*,*,#10556,.F.);
#15166=ORIENTED_EDGE('',*,*,#10655,.F.);
#15167=ORIENTED_EDGE('',*,*,#10622,.F.);
#15168=ORIENTED_EDGE('',*,*,#10656,.T.);
#15169=ORIENTED_EDGE('',*,*,#10645,.F.);
#15170=ORIENTED_EDGE('',*,*,#10656,.F.);
#15171=ORIENTED_EDGE('',*,*,#10603,.F.);
#15172=ORIENTED_EDGE('',*,*,#10657,.T.);
#15173=ORIENTED_EDGE('',*,*,#10555,.F.);
#15174=ORIENTED_EDGE('',*,*,#10657,.F.);
#15175=ORIENTED_EDGE('',*,*,#10658,.F.);
#15176=ORIENTED_EDGE('',*,*,#10659,.T.);
#15177=ORIENTED_EDGE('',*,*,#10608,.F.);
#15178=ORIENTED_EDGE('',*,*,#10594,.T.);
#15179=ORIENTED_EDGE('',*,*,#10626,.F.);
#15180=ORIENTED_EDGE('',*,*,#10660,.T.);
#15181=ORIENTED_EDGE('',*,*,#10624,.F.);
#15182=ORIENTED_EDGE('',*,*,#10574,.F.);
#15183=ORIENTED_EDGE('',*,*,#10609,.F.);
#15184=ORIENTED_EDGE('',*,*,#10659,.F.);
#15185=ORIENTED_EDGE('',*,*,#10661,.F.);
#15186=ORIENTED_EDGE('',*,*,#10662,.T.);
#15187=ORIENTED_EDGE('',*,*,#10658,.T.);
#15188=ORIENTED_EDGE('',*,*,#10662,.F.);
#15189=ORIENTED_EDGE('',*,*,#10661,.T.);
#15190=ORIENTED_EDGE('',*,*,#10625,.F.);
#15191=ORIENTED_EDGE('',*,*,#10660,.F.);
#15192=ORIENTED_EDGE('',*,*,#10529,.F.);
#15193=ORIENTED_EDGE('',*,*,#10621,.F.);
#15194=ORIENTED_EDGE('',*,*,#10538,.F.);
#15195=ORIENTED_EDGE('',*,*,#10553,.F.);
#15196=ORIENTED_EDGE('',*,*,#10543,.F.);
#15197=ORIENTED_EDGE('',*,*,#10596,.F.);
#15198=ORIENTED_EDGE('',*,*,#10648,.F.);
#15199=ORIENTED_EDGE('',*,*,#10652,.F.);
#15200=ORIENTED_EDGE('',*,*,#10663,.T.);
#15201=ORIENTED_EDGE('',*,*,#10664,.T.);
#15202=ORIENTED_EDGE('',*,*,#10665,.T.);
#15203=ORIENTED_EDGE('',*,*,#10664,.F.);
#15204=ORIENTED_EDGE('',*,*,#10663,.F.);
#15205=ORIENTED_EDGE('',*,*,#10666,.T.);
#15206=ORIENTED_EDGE('',*,*,#10667,.F.);
#15207=ORIENTED_EDGE('',*,*,#10666,.F.);
#15208=ORIENTED_EDGE('',*,*,#10668,.F.);
#15209=ORIENTED_EDGE('',*,*,#10669,.T.);
#15210=ORIENTED_EDGE('',*,*,#10665,.F.);
#15211=ORIENTED_EDGE('',*,*,#10669,.F.);
#15212=ORIENTED_EDGE('',*,*,#10667,.T.);
#15213=ORIENTED_EDGE('',*,*,#10670,.T.);
#15214=ORIENTED_EDGE('',*,*,#10671,.T.);
#15215=ORIENTED_EDGE('',*,*,#10670,.F.);
#15216=ORIENTED_EDGE('',*,*,#10671,.F.);
#15217=ORIENTED_EDGE('',*,*,#10672,.T.);
#15218=ORIENTED_EDGE('',*,*,#10673,.T.);
#15219=ORIENTED_EDGE('',*,*,#10674,.T.);
#15220=ORIENTED_EDGE('',*,*,#10675,.T.);
#15221=ORIENTED_EDGE('',*,*,#10676,.T.);
#15222=ORIENTED_EDGE('',*,*,#10674,.F.);
#15223=ORIENTED_EDGE('',*,*,#10676,.F.);
#15224=ORIENTED_EDGE('',*,*,#10677,.T.);
#15225=ORIENTED_EDGE('',*,*,#10678,.T.);
#15226=ORIENTED_EDGE('',*,*,#10679,.T.);
#15227=ORIENTED_EDGE('',*,*,#10677,.F.);
#15228=ORIENTED_EDGE('',*,*,#10675,.F.);
#15229=ORIENTED_EDGE('',*,*,#10673,.F.);
#15230=ORIENTED_EDGE('',*,*,#10680,.T.);
#15231=ORIENTED_EDGE('',*,*,#10681,.F.);
#15232=ORIENTED_EDGE('',*,*,#10682,.T.);
#15233=ORIENTED_EDGE('',*,*,#10680,.F.);
#15234=ORIENTED_EDGE('',*,*,#10682,.F.);
#15235=ORIENTED_EDGE('',*,*,#10672,.F.);
#15236=ORIENTED_EDGE('',*,*,#10683,.T.);
#15237=ORIENTED_EDGE('',*,*,#10681,.T.);
#15238=ORIENTED_EDGE('',*,*,#10683,.F.);
#15239=ORIENTED_EDGE('',*,*,#10678,.F.);
#15240=ORIENTED_EDGE('',*,*,#10679,.F.);
#15241=ORIENTED_EDGE('',*,*,#10684,.T.);
#15242=ORIENTED_EDGE('',*,*,#10668,.T.);
#15243=ORIENTED_EDGE('',*,*,#10684,.F.);
#15244=ORIENTED_EDGE('',*,*,#10685,.T.);
#15245=ORIENTED_EDGE('',*,*,#10686,.T.);
#15246=ORIENTED_EDGE('',*,*,#10687,.T.);
#15247=ORIENTED_EDGE('',*,*,#10688,.T.);
#15248=ORIENTED_EDGE('',*,*,#10689,.T.);
#15249=ORIENTED_EDGE('',*,*,#10690,.T.);
#15250=ORIENTED_EDGE('',*,*,#10685,.F.);
#15251=ORIENTED_EDGE('',*,*,#10691,.T.);
#15252=ORIENTED_EDGE('',*,*,#10692,.T.);
#15253=ORIENTED_EDGE('',*,*,#10693,.T.);
#15254=ORIENTED_EDGE('',*,*,#10689,.F.);
#15255=ORIENTED_EDGE('',*,*,#10694,.T.);
#15256=ORIENTED_EDGE('',*,*,#10687,.F.);
#15257=ORIENTED_EDGE('',*,*,#10695,.T.);
#15258=ORIENTED_EDGE('',*,*,#10692,.F.);
#15259=ORIENTED_EDGE('',*,*,#10696,.T.);
#15260=ORIENTED_EDGE('',*,*,#10695,.F.);
#15261=ORIENTED_EDGE('',*,*,#10697,.T.);
#15262=ORIENTED_EDGE('',*,*,#10698,.F.);
#15263=ORIENTED_EDGE('',*,*,#10699,.F.);
#15264=ORIENTED_EDGE('',*,*,#10686,.F.);
#15265=ORIENTED_EDGE('',*,*,#10700,.T.);
#15266=ORIENTED_EDGE('',*,*,#10701,.F.);
#15267=ORIENTED_EDGE('',*,*,#10697,.F.);
#15268=ORIENTED_EDGE('',*,*,#10688,.F.);
#15269=ORIENTED_EDGE('',*,*,#10696,.F.);
#15270=ORIENTED_EDGE('',*,*,#10694,.F.);
#15271=ORIENTED_EDGE('',*,*,#10691,.F.);
#15272=ORIENTED_EDGE('',*,*,#10702,.T.);
#15273=ORIENTED_EDGE('',*,*,#10703,.T.);
#15274=ORIENTED_EDGE('',*,*,#10704,.T.);
#15275=ORIENTED_EDGE('',*,*,#10705,.T.);
#15276=ORIENTED_EDGE('',*,*,#10706,.T.);
#15277=ORIENTED_EDGE('',*,*,#10698,.T.);
#15278=ORIENTED_EDGE('',*,*,#10707,.T.);
#15279=ORIENTED_EDGE('',*,*,#10708,.T.);
#15280=ORIENTED_EDGE('',*,*,#10704,.F.);
#15281=ORIENTED_EDGE('',*,*,#10701,.T.);
#15282=ORIENTED_EDGE('',*,*,#10709,.T.);
#15283=ORIENTED_EDGE('',*,*,#10710,.T.);
#15284=ORIENTED_EDGE('',*,*,#10707,.F.);
#15285=ORIENTED_EDGE('',*,*,#10711,.T.);
#15286=ORIENTED_EDGE('',*,*,#10706,.F.);
#15287=ORIENTED_EDGE('',*,*,#10712,.T.);
#15288=ORIENTED_EDGE('',*,*,#10709,.F.);
#15289=ORIENTED_EDGE('',*,*,#10713,.T.);
#15290=ORIENTED_EDGE('',*,*,#10712,.F.);
#15291=ORIENTED_EDGE('',*,*,#10714,.F.);
#15292=ORIENTED_EDGE('',*,*,#10715,.F.);
#15293=ORIENTED_EDGE('',*,*,#10716,.F.);
#15294=ORIENTED_EDGE('',*,*,#10705,.F.);
#15295=ORIENTED_EDGE('',*,*,#10717,.T.);
#15296=ORIENTED_EDGE('',*,*,#10718,.F.);
#15297=ORIENTED_EDGE('',*,*,#10714,.T.);
#15298=ORIENTED_EDGE('',*,*,#10719,.T.);
#15299=ORIENTED_EDGE('',*,*,#10718,.T.);
#15300=ORIENTED_EDGE('',*,*,#10720,.T.);
#15301=ORIENTED_EDGE('',*,*,#10721,.T.);
#15302=ORIENTED_EDGE('',*,*,#10722,.T.);
#15303=ORIENTED_EDGE('',*,*,#10715,.T.);
#15304=ORIENTED_EDGE('',*,*,#10719,.F.);
#15305=ORIENTED_EDGE('',*,*,#10723,.T.);
#15306=ORIENTED_EDGE('',*,*,#10724,.T.);
#15307=ORIENTED_EDGE('',*,*,#10725,.T.);
#15308=ORIENTED_EDGE('',*,*,#10722,.F.);
#15309=ORIENTED_EDGE('',*,*,#10726,.T.);
#15310=ORIENTED_EDGE('',*,*,#10720,.F.);
#15311=ORIENTED_EDGE('',*,*,#10727,.T.);
#15312=ORIENTED_EDGE('',*,*,#10724,.F.);
#15313=ORIENTED_EDGE('',*,*,#10728,.T.);
#15314=ORIENTED_EDGE('',*,*,#10708,.F.);
#15315=ORIENTED_EDGE('',*,*,#10729,.T.);
#15316=ORIENTED_EDGE('',*,*,#10727,.F.);
#15317=ORIENTED_EDGE('',*,*,#10717,.F.);
#15318=ORIENTED_EDGE('',*,*,#10721,.F.);
#15319=ORIENTED_EDGE('',*,*,#10728,.F.);
#15320=ORIENTED_EDGE('',*,*,#10726,.F.);
#15321=ORIENTED_EDGE('',*,*,#10723,.F.);
#15322=ORIENTED_EDGE('',*,*,#10730,.T.);
#15323=ORIENTED_EDGE('',*,*,#10731,.T.);
#15324=ORIENTED_EDGE('',*,*,#10710,.F.);
#15325=ORIENTED_EDGE('',*,*,#10716,.T.);
#15326=ORIENTED_EDGE('',*,*,#10725,.F.);
#15327=ORIENTED_EDGE('',*,*,#10729,.F.);
#15328=ORIENTED_EDGE('',*,*,#10703,.F.);
#15329=ORIENTED_EDGE('',*,*,#10732,.T.);
#15330=ORIENTED_EDGE('',*,*,#10730,.F.);
#15331=ORIENTED_EDGE('',*,*,#10732,.F.);
#15332=ORIENTED_EDGE('',*,*,#10702,.F.);
#15333=ORIENTED_EDGE('',*,*,#10733,.T.);
#15334=ORIENTED_EDGE('',*,*,#10731,.F.);
#15335=ORIENTED_EDGE('',*,*,#10733,.F.);
#15336=ORIENTED_EDGE('',*,*,#10693,.F.);
#15337=ORIENTED_EDGE('',*,*,#10699,.T.);
#15338=ORIENTED_EDGE('',*,*,#10713,.F.);
#15339=ORIENTED_EDGE('',*,*,#10734,.F.);
#15340=ORIENTED_EDGE('',*,*,#10690,.F.);
#15341=ORIENTED_EDGE('',*,*,#10734,.T.);
#15342=ORIENTED_EDGE('',*,*,#10711,.F.);
#15343=ORIENTED_EDGE('',*,*,#10700,.F.);
#15344=ORIENTED_EDGE('',*,*,#10735,.F.);
#15345=ORIENTED_EDGE('',*,*,#10736,.F.);
#15346=ORIENTED_EDGE('',*,*,#10737,.T.);
#15347=ORIENTED_EDGE('',*,*,#10735,.T.);
#15348=ORIENTED_EDGE('',*,*,#10737,.F.);
#15349=ORIENTED_EDGE('',*,*,#10738,.F.);
#15350=ORIENTED_EDGE('',*,*,#10739,.T.);
#15351=ORIENTED_EDGE('',*,*,#10736,.T.);
#15352=ORIENTED_EDGE('',*,*,#10739,.F.);
#15353=ORIENTED_EDGE('',*,*,#10738,.T.);
#15354=ORIENTED_EDGE('',*,*,#10740,.F.);
#15355=ORIENTED_EDGE('',*,*,#10741,.F.);
#15356=ORIENTED_EDGE('',*,*,#10742,.T.);
#15357=ORIENTED_EDGE('',*,*,#10740,.T.);
#15358=ORIENTED_EDGE('',*,*,#10742,.F.);
#15359=ORIENTED_EDGE('',*,*,#10743,.F.);
#15360=ORIENTED_EDGE('',*,*,#10741,.T.);
#15361=ORIENTED_EDGE('',*,*,#10744,.F.);
#15362=ORIENTED_EDGE('',*,*,#10745,.T.);
#15363=ORIENTED_EDGE('',*,*,#10743,.T.);
#15364=ORIENTED_EDGE('',*,*,#10745,.F.);
#15365=ORIENTED_EDGE('',*,*,#10744,.T.);
#15366=ORIENTED_EDGE('',*,*,#10746,.F.);
#15367=ORIENTED_EDGE('',*,*,#10747,.F.);
#15368=ORIENTED_EDGE('',*,*,#10748,.T.);
#15369=ORIENTED_EDGE('',*,*,#10746,.T.);
#15370=ORIENTED_EDGE('',*,*,#10748,.F.);
#15371=ORIENTED_EDGE('',*,*,#10749,.F.);
#15372=ORIENTED_EDGE('',*,*,#10747,.T.);
#15373=ORIENTED_EDGE('',*,*,#10750,.F.);
#15374=ORIENTED_EDGE('',*,*,#10751,.T.);
#15375=ORIENTED_EDGE('',*,*,#10749,.T.);
#15376=ORIENTED_EDGE('',*,*,#10751,.F.);
#15377=ORIENTED_EDGE('',*,*,#10752,.F.);
#15378=ORIENTED_EDGE('',*,*,#10753,.T.);
#15379=ORIENTED_EDGE('',*,*,#10750,.T.);
#15380=ORIENTED_EDGE('',*,*,#10753,.F.);
#15381=ORIENTED_EDGE('',*,*,#10752,.T.);
#15382=ORIENTED_EDGE('',*,*,#10754,.T.);
#15383=ORIENTED_EDGE('',*,*,#10755,.T.);
#15384=ORIENTED_EDGE('',*,*,#10756,.T.);
#15385=ORIENTED_EDGE('',*,*,#10757,.F.);
#15386=ORIENTED_EDGE('',*,*,#10758,.T.);
#15387=ORIENTED_EDGE('',*,*,#10759,.T.);
#15388=ORIENTED_EDGE('',*,*,#10760,.T.);
#15389=ORIENTED_EDGE('',*,*,#10755,.F.);
#15390=ORIENTED_EDGE('',*,*,#10761,.T.);
#15391=ORIENTED_EDGE('',*,*,#10762,.T.);
#15392=ORIENTED_EDGE('',*,*,#10763,.T.);
#15393=ORIENTED_EDGE('',*,*,#10759,.F.);
#15394=ORIENTED_EDGE('',*,*,#10764,.T.);
#15395=ORIENTED_EDGE('',*,*,#10762,.F.);
#15396=ORIENTED_EDGE('',*,*,#10765,.T.);
#15397=ORIENTED_EDGE('',*,*,#10757,.T.);
#15398=ORIENTED_EDGE('',*,*,#10764,.F.);
#15399=ORIENTED_EDGE('',*,*,#10766,.F.);
#15400=ORIENTED_EDGE('',*,*,#10767,.F.);
#15401=ORIENTED_EDGE('',*,*,#10768,.T.);
#15402=ORIENTED_EDGE('',*,*,#10756,.F.);
#15403=ORIENTED_EDGE('',*,*,#10769,.F.);
#15404=ORIENTED_EDGE('',*,*,#10770,.F.);
#15405=ORIENTED_EDGE('',*,*,#10766,.T.);
#15406=ORIENTED_EDGE('',*,*,#10754,.F.);
#15407=ORIENTED_EDGE('',*,*,#10765,.F.);
#15408=ORIENTED_EDGE('',*,*,#10761,.F.);
#15409=ORIENTED_EDGE('',*,*,#10758,.F.);
#15410=ORIENTED_EDGE('',*,*,#10771,.T.);
#15411=ORIENTED_EDGE('',*,*,#10770,.T.);
#15412=ORIENTED_EDGE('',*,*,#10772,.T.);
#15413=ORIENTED_EDGE('',*,*,#10773,.T.);
#15414=ORIENTED_EDGE('',*,*,#10774,.T.);
#15415=ORIENTED_EDGE('',*,*,#10775,.T.);
#15416=ORIENTED_EDGE('',*,*,#10776,.T.);
#15417=ORIENTED_EDGE('',*,*,#10767,.T.);
#15418=ORIENTED_EDGE('',*,*,#10774,.F.);
#15419=ORIENTED_EDGE('',*,*,#10777,.T.);
#15420=ORIENTED_EDGE('',*,*,#10778,.T.);
#15421=ORIENTED_EDGE('',*,*,#10779,.T.);
#15422=ORIENTED_EDGE('',*,*,#10776,.F.);
#15423=ORIENTED_EDGE('',*,*,#10780,.T.);
#15424=ORIENTED_EDGE('',*,*,#10778,.F.);
#15425=ORIENTED_EDGE('',*,*,#10781,.T.);
#15426=ORIENTED_EDGE('',*,*,#10772,.F.);
#15427=ORIENTED_EDGE('',*,*,#10760,.F.);
#15428=ORIENTED_EDGE('',*,*,#10782,.F.);
#15429=ORIENTED_EDGE('',*,*,#10780,.F.);
#15430=ORIENTED_EDGE('',*,*,#10769,.T.);
#15431=ORIENTED_EDGE('',*,*,#10773,.F.);
#15432=ORIENTED_EDGE('',*,*,#10781,.F.);
#15433=ORIENTED_EDGE('',*,*,#10777,.F.);
#15434=ORIENTED_EDGE('',*,*,#10775,.F.);
#15435=ORIENTED_EDGE('',*,*,#10783,.T.);
#15436=ORIENTED_EDGE('',*,*,#10783,.F.);
#15437=ORIENTED_EDGE('',*,*,#10784,.T.);
#15438=ORIENTED_EDGE('',*,*,#10771,.F.);
#15439=ORIENTED_EDGE('',*,*,#10784,.F.);
#15440=ORIENTED_EDGE('',*,*,#10763,.F.);
#15441=ORIENTED_EDGE('',*,*,#10768,.F.);
#15442=ORIENTED_EDGE('',*,*,#10779,.F.);
#15443=ORIENTED_EDGE('',*,*,#10782,.T.);
#15444=ORIENTED_EDGE('',*,*,#10785,.F.);
#15445=ORIENTED_EDGE('',*,*,#10786,.F.);
#15446=ORIENTED_EDGE('',*,*,#10787,.F.);
#15447=ORIENTED_EDGE('',*,*,#10788,.T.);
#15448=ORIENTED_EDGE('',*,*,#10786,.T.);
#15449=ORIENTED_EDGE('',*,*,#10788,.F.);
#15450=ORIENTED_EDGE('',*,*,#10785,.T.);
#15451=ORIENTED_EDGE('',*,*,#10789,.T.);
#15452=ORIENTED_EDGE('',*,*,#10787,.T.);
#15453=ORIENTED_EDGE('',*,*,#10789,.F.);
#15454=ORIENTED_EDGE('',*,*,#10790,.T.);
#15455=ORIENTED_EDGE('',*,*,#10791,.T.);
#15456=ORIENTED_EDGE('',*,*,#10792,.F.);
#15457=ORIENTED_EDGE('',*,*,#10793,.F.);
#15458=ORIENTED_EDGE('',*,*,#10794,.F.);
#15459=ORIENTED_EDGE('',*,*,#10793,.T.);
#15460=ORIENTED_EDGE('',*,*,#10795,.F.);
#15461=ORIENTED_EDGE('',*,*,#10796,.F.);
#15462=ORIENTED_EDGE('',*,*,#10797,.F.);
#15463=ORIENTED_EDGE('',*,*,#10796,.T.);
#15464=ORIENTED_EDGE('',*,*,#10798,.F.);
#15465=ORIENTED_EDGE('',*,*,#10799,.F.);
#15466=ORIENTED_EDGE('',*,*,#10800,.T.);
#15467=ORIENTED_EDGE('',*,*,#10799,.T.);
#15468=ORIENTED_EDGE('',*,*,#10801,.F.);
#15469=ORIENTED_EDGE('',*,*,#10791,.F.);
#15470=ORIENTED_EDGE('',*,*,#10801,.T.);
#15471=ORIENTED_EDGE('',*,*,#10798,.T.);
#15472=ORIENTED_EDGE('',*,*,#10795,.T.);
#15473=ORIENTED_EDGE('',*,*,#10792,.T.);
#15474=ORIENTED_EDGE('',*,*,#10800,.F.);
#15475=ORIENTED_EDGE('',*,*,#10790,.F.);
#15476=ORIENTED_EDGE('',*,*,#10794,.T.);
#15477=ORIENTED_EDGE('',*,*,#10797,.T.);
#15478=CONICAL_SURFACE('',#16760,15.45,0.785398163397451);
#15479=CONICAL_SURFACE('',#16768,15.45,0.785398163397451);
#15480=CONICAL_SURFACE('',#16895,26.5,0.785398163397451);
#15481=CONICAL_SURFACE('',#16963,21.525,0.759762754875774);
#15482=CONICAL_SURFACE('',#17027,4.25,0.785398163397441);
#15483=CONICAL_SURFACE('',#17036,4.25,0.785398163397441);
#15484=CONICAL_SURFACE('',#17040,24.9267766952966,1.17809724509617);
#15485=CONICAL_SURFACE('',#17044,25.5,0.785398163397451);
#15486=CONICAL_SURFACE('',#17048,9.82322330470336,0.39269908169873);
#15487=CONICAL_SURFACE('',#17051,9.6,0.785398163397448);
#15488=CONICAL_SURFACE('',#17053,9.12677669529663,1.17809724509617);
#15489=CONICAL_SURFACE('',#17076,5.25,0.785398163397437);
#15490=CONICAL_SURFACE('',#17083,4.20999999999999,0.785398163397437);
#15491=CONICAL_SURFACE('',#17087,12.6,0.785398163397448);
#15492=CONICAL_SURFACE('',#17104,20.6,0.785398163397448);
#15493=CONICAL_SURFACE('',#17109,25.5,0.785398163397442);
#15494=CONICAL_SURFACE('',#17110,16.1,0.785398163397437);
#15495=CONICAL_SURFACE('',#17118,14.6,0.785398163397454);
#15496=CONICAL_SURFACE('',#17124,17.71,0.785398163397442);
#15497=CONICAL_SURFACE('',#17144,17.71,0.785398163397459);
#15498=CONICAL_SURFACE('',#17168,2.9,0.785398163397449);
#15499=CONICAL_SURFACE('',#17172,2.9,0.785398163397448);
#15500=CONICAL_SURFACE('',#17256,2.8,0.785398163397448);
#15501=CONICAL_SURFACE('',#17276,2.8,0.785398163397448);
#15502=CONICAL_SURFACE('',#17305,14.9061737618886,1.12276863450922);
#15503=CONICAL_SURFACE('',#17309,19.,0.674740942223553);
#15504=CONICAL_SURFACE('',#17314,22.8438262381114,0.337370471111777);
#15505=CONICAL_SURFACE('',#17330,22.6,0.785398163397437);
#15506=CONICAL_SURFACE('',#17331,11.6,0.785398163397437);
#15507=CONICAL_SURFACE('',#17437,6.8,0.785398163397415);
#15508=CONICAL_SURFACE('',#17544,4.8,0.785398163397415);
#15509=CONICAL_SURFACE('',#17549,6.8,0.785398163397415);
#15510=CONICAL_SURFACE('',#17550,6.8,0.785398163397415);
#15511=CONICAL_SURFACE('',#17552,9.75,0.785398163397442);
#15512=CONICAL_SURFACE('',#17564,12.8,0.785398163397459);
#15513=CONICAL_SURFACE('',#17568,11.5,0.785398163397447);
#15514=CONICAL_SURFACE('',#17573,7.98717082451265,1.40992104959656);
#15515=CONICAL_SURFACE('',#17577,10.25,1.24904577239826);
#15516=CONICAL_SURFACE('',#17581,12.4081387239171,0.934647629190528);
#15517=CONICAL_SURFACE('',#17584,13.75,0.620249485982819);
#15518=CONICAL_SURFACE('',#17587,14.8546904515702,0.310124742991409);
#15519=CONICAL_SURFACE('',#17597,14.65,0.78539816339747);
#15520=CONICAL_SURFACE('',#17600,11.5,0.785398163397447);
#15521=CONICAL_SURFACE('',#17864,3.,0.982793723247329);
#15522=CONICAL_SURFACE('',#17866,4.75,0.785398163397448);
#15523=CONICAL_SURFACE('',#17872,12.7,0.785398163397447);
#15524=CONICAL_SURFACE('',#17876,12.7,0.785398163397448);
#15525=CONICAL_SURFACE('',#17886,8.75,0.785398163397448);
#15526=CONICAL_SURFACE('',#17895,8.75,0.785398163397448);
#15527=CONICAL_SURFACE('',#17959,10.8232233047034,0.392699081698727);
#15528=CONICAL_SURFACE('',#17962,10.5,0.785398163397451);
#15529=CONICAL_SURFACE('',#17966,9.92677669529664,1.17809724509617);
#15530=CONICAL_SURFACE('',#17988,5.9,0.785398163397448);
#15531=CONICAL_SURFACE('',#17992,5.9,0.785398163397448);
#15532=CONICAL_SURFACE('',#18003,5.92928932188135,0.392699081698723);
#15533=CONICAL_SURFACE('',#18006,5.92928932188134,0.392699081698725);
#15534=CONICAL_SURFACE('',#18009,5.8,0.785398163397448);
#15535=CONICAL_SURFACE('',#18013,5.57071067811865,1.17809724509617);
#15536=CONICAL_SURFACE('',#18016,5.57071067811865,1.17809724509617);
#15537=CONICAL_SURFACE('',#18019,5.8,0.785398163397448);
#15538=CONICAL_SURFACE('',#18031,2.8,0.785398163397448);
#15539=CONICAL_SURFACE('',#18051,2.8,0.785398163397448);
#15540=CONICAL_SURFACE('',#18055,5.305,0.785398163397448);
#15541=CONICAL_SURFACE('',#18066,5.305,0.785398163397449);
#15542=CONICAL_SURFACE('',#18079,3.74,0.78539816339745);
#15543=ADVANCED_FACE('',(#1815),#15478,.F.);
#15544=ADVANCED_FACE('',(#1816),#1563,.F.);
#15545=ADVANCED_FACE('',(#1817,#939),#1062,.F.);
#15546=ADVANCED_FACE('',(#1818),#15479,.F.);
#15547=ADVANCED_FACE('',(#1819,#940),#1063,.F.);
#15548=ADVANCED_FACE('',(#1820),#814,.T.);
#15549=ADVANCED_FACE('',(#1821),#815,.T.);
#15550=ADVANCED_FACE('',(#1822),#1064,.T.);
#15551=ADVANCED_FACE('',(#1823),#1065,.F.);
#15552=ADVANCED_FACE('',(#1824),#1564,.T.);
#15553=ADVANCED_FACE('',(#1825),#1066,.T.);
#15554=ADVANCED_FACE('',(#1826),#816,.T.);
#15555=ADVANCED_FACE('',(#1827),#817,.T.);
#15556=ADVANCED_FACE('',(#1828),#818,.T.);
#15557=ADVANCED_FACE('',(#1829),#819,.T.);
#15558=ADVANCED_FACE('',(#1830),#820,.T.);
#15559=ADVANCED_FACE('',(#1831),#1067,.T.);
#15560=ADVANCED_FACE('',(#1832),#821,.T.);
#15561=ADVANCED_FACE('',(#1833),#822,.T.);
#15562=ADVANCED_FACE('',(#1834),#823,.T.);
#15563=ADVANCED_FACE('',(#1835),#824,.T.);
#15564=ADVANCED_FACE('',(#1836),#825,.T.);
#15565=ADVANCED_FACE('',(#1837),#1565,.T.);
#15566=ADVANCED_FACE('',(#1838),#1068,.T.);
#15567=ADVANCED_FACE('',(#1839),#1566,.T.);
#15568=ADVANCED_FACE('',(#1840),#1069,.T.);
#15569=ADVANCED_FACE('',(#1841),#1567,.T.);
#15570=ADVANCED_FACE('',(#1842),#231,.T.);
#15571=ADVANCED_FACE('',(#1843),#232,.T.);
#15572=ADVANCED_FACE('',(#1844),#1568,.T.);
#15573=ADVANCED_FACE('',(#1845),#1569,.T.);
#15574=ADVANCED_FACE('',(#1846),#1070,.T.);
#15575=ADVANCED_FACE('',(#1847),#233,.T.);
#15576=ADVANCED_FACE('',(#1848),#1570,.T.);
#15577=ADVANCED_FACE('',(#1849),#1571,.T.);
#15578=ADVANCED_FACE('',(#1850),#234,.T.);
#15579=ADVANCED_FACE('',(#1851),#235,.T.);
#15580=ADVANCED_FACE('',(#1852),#1572,.T.);
#15581=ADVANCED_FACE('',(#1853),#1573,.T.);
#15582=ADVANCED_FACE('',(#1854),#236,.T.);
#15583=ADVANCED_FACE('',(#1855),#237,.T.);
#15584=ADVANCED_FACE('',(#1856),#1574,.T.);
#15585=ADVANCED_FACE('',(#1857),#1575,.T.);
#15586=ADVANCED_FACE('',(#1858),#238,.T.);
#15587=ADVANCED_FACE('',(#1859),#239,.T.);
#15588=ADVANCED_FACE('',(#1860),#1576,.T.);
#15589=ADVANCED_FACE('',(#1861),#1577,.T.);
#15590=ADVANCED_FACE('',(#1862),#240,.T.);
#15591=ADVANCED_FACE('',(#1863),#1578,.T.);
#15592=ADVANCED_FACE('',(#1864),#241,.T.);
#15593=ADVANCED_FACE('',(#1865),#1579,.T.);
#15594=ADVANCED_FACE('',(#1866),#1580,.T.);
#15595=ADVANCED_FACE('',(#1867),#242,.T.);
#15596=ADVANCED_FACE('',(#1868),#1581,.T.);
#15597=ADVANCED_FACE('',(#1869),#243,.T.);
#15598=ADVANCED_FACE('',(#1870,#941,#942,#943,#944),#1071,.T.);
#15599=ADVANCED_FACE('',(#1871),#1072,.T.);
#15600=ADVANCED_FACE('',(#1872),#1582,.T.);
#15601=ADVANCED_FACE('',(#1873),#1583,.T.);
#15602=ADVANCED_FACE('',(#1874),#1584,.T.);
#15603=ADVANCED_FACE('',(#1875),#1073,.T.);
#15604=ADVANCED_FACE('',(#1876),#1585,.T.);
#15605=ADVANCED_FACE('',(#1877),#1586,.T.);
#15606=ADVANCED_FACE('',(#1878),#1587,.T.);
#15607=ADVANCED_FACE('',(#1879),#1588,.T.);
#15608=ADVANCED_FACE('',(#1880),#1074,.T.);
#15609=ADVANCED_FACE('',(#1881),#1075,.T.);
#15610=ADVANCED_FACE('',(#1882),#1589,.T.);
#15611=ADVANCED_FACE('',(#1883),#1590,.T.);
#15612=ADVANCED_FACE('',(#1884),#1076,.F.);
#15613=ADVANCED_FACE('',(#1885),#244,.T.);
#15614=ADVANCED_FACE('',(#1886),#1591,.T.);
#15615=ADVANCED_FACE('',(#1887),#1592,.T.);
#15616=ADVANCED_FACE('',(#1888),#245,.T.);
#15617=ADVANCED_FACE('',(#1889),#1593,.T.);
#15618=ADVANCED_FACE('',(#1890),#1077,.T.);
#15619=ADVANCED_FACE('',(#1891),#1594,.T.);
#15620=ADVANCED_FACE('',(#1892),#1595,.T.);
#15621=ADVANCED_FACE('',(#1893),#1078,.T.);
#15622=ADVANCED_FACE('',(#1894),#215,.T.);
#15623=ADVANCED_FACE('',(#1895),#15480,.T.);
#15624=ADVANCED_FACE('',(#1896,#945),#1079,.T.);
#15625=ADVANCED_FACE('',(#1897),#216,.T.);
#15626=ADVANCED_FACE('',(#1898),#1596,.T.);
#15627=ADVANCED_FACE('',(#1899),#217,.T.);
#15628=ADVANCED_FACE('',(#1900),#1597,.T.);
#15629=ADVANCED_FACE('',(#1901),#218,.T.);
#15630=ADVANCED_FACE('',(#1902),#1598,.T.);
#15631=ADVANCED_FACE('',(#1903),#219,.T.);
#15632=ADVANCED_FACE('',(#1904),#1599,.T.);
#15633=ADVANCED_FACE('',(#1905),#220,.T.);
#15634=ADVANCED_FACE('',(#1906),#221,.T.);
#15635=ADVANCED_FACE('',(#1907),#222,.T.);
#15636=ADVANCED_FACE('',(#1908),#1600,.T.);
#15637=ADVANCED_FACE('',(#1909),#223,.T.);
#15638=ADVANCED_FACE('',(#1910,#946),#1080,.F.);
#15639=ADVANCED_FACE('',(#1911),#1601,.F.);
#15640=ADVANCED_FACE('',(#1912),#1081,.F.);
#15641=ADVANCED_FACE('',(#1913),#1602,.F.);
#15642=ADVANCED_FACE('',(#1914),#826,.F.);
#15643=ADVANCED_FACE('',(#1915),#827,.F.);
#15644=ADVANCED_FACE('',(#1916),#828,.F.);
#15645=ADVANCED_FACE('',(#1917),#829,.F.);
#15646=ADVANCED_FACE('',(#1918),#830,.F.);
#15647=ADVANCED_FACE('',(#1919),#831,.F.);
#15648=ADVANCED_FACE('',(#1920),#832,.F.);
#15649=ADVANCED_FACE('',(#1921),#833,.F.);
#15650=ADVANCED_FACE('',(#1922),#834,.F.);
#15651=ADVANCED_FACE('',(#1923),#835,.F.);
#15652=ADVANCED_FACE('',(#1924),#836,.F.);
#15653=ADVANCED_FACE('',(#1925),#1082,.T.);
#15654=ADVANCED_FACE('',(#1926),#1083,.F.);
#15655=ADVANCED_FACE('',(#1927),#1084,.F.);
#15656=ADVANCED_FACE('',(#1928),#1085,.F.);
#15657=ADVANCED_FACE('',(#1929),#1086,.F.);
#15658=ADVANCED_FACE('',(#1930),#1087,.F.);
#15659=ADVANCED_FACE('',(#1931),#1088,.F.);
#15660=ADVANCED_FACE('',(#1932),#1089,.F.);
#15661=ADVANCED_FACE('',(#1933),#1090,.F.);
#15662=ADVANCED_FACE('',(#1934),#1091,.F.);
#15663=ADVANCED_FACE('',(#1935),#837,.F.);
#15664=ADVANCED_FACE('',(#1936),#838,.F.);
#15665=ADVANCED_FACE('',(#1937),#839,.F.);
#15666=ADVANCED_FACE('',(#1938),#840,.F.);
#15667=ADVANCED_FACE('',(#1939),#841,.F.);
#15668=ADVANCED_FACE('',(#1940),#842,.F.);
#15669=ADVANCED_FACE('',(#1941),#843,.F.);
#15670=ADVANCED_FACE('',(#1942),#844,.F.);
#15671=ADVANCED_FACE('',(#1943),#845,.F.);
#15672=ADVANCED_FACE('',(#1944),#846,.F.);
#15673=ADVANCED_FACE('',(#1945),#847,.F.);
#15674=ADVANCED_FACE('',(#1946),#848,.F.);
#15675=ADVANCED_FACE('',(#1947),#849,.F.);
#15676=ADVANCED_FACE('',(#1948),#850,.F.);
#15677=ADVANCED_FACE('',(#1949),#851,.F.);
#15678=ADVANCED_FACE('',(#1950),#852,.F.);
#15679=ADVANCED_FACE('',(#1951),#1092,.T.);
#15680=ADVANCED_FACE('',(#1952),#1093,.F.);
#15681=ADVANCED_FACE('',(#1953),#1094,.F.);
#15682=ADVANCED_FACE('',(#1954),#1095,.F.);
#15683=ADVANCED_FACE('',(#1955),#1096,.F.);
#15684=ADVANCED_FACE('',(#1956),#1097,.F.);
#15685=ADVANCED_FACE('',(#1957),#1098,.F.);
#15686=ADVANCED_FACE('',(#1958),#1099,.F.);
#15687=ADVANCED_FACE('',(#1959),#1100,.F.);
#15688=ADVANCED_FACE('',(#1960),#1101,.F.);
#15689=ADVANCED_FACE('',(#1961),#1102,.F.);
#15690=ADVANCED_FACE('',(#1962),#1103,.F.);
#15691=ADVANCED_FACE('',(#1963),#1603,.F.);
#15692=ADVANCED_FACE('',(#1964),#1104,.T.);
#15693=ADVANCED_FACE('',(#1965),#15481,.F.);
#15694=ADVANCED_FACE('',(#1966),#1604,.F.);
#15695=ADVANCED_FACE('',(#1967),#1105,.T.);
#15696=ADVANCED_FACE('',(#1968),#1106,.T.);
#15697=ADVANCED_FACE('',(#1969),#1107,.T.);
#15698=ADVANCED_FACE('',(#1970),#1605,.T.);
#15699=ADVANCED_FACE('',(#1971),#1606,.T.);
#15700=ADVANCED_FACE('',(#1972),#1607,.T.);
#15701=ADVANCED_FACE('',(#1973),#1608,.T.);
#15702=ADVANCED_FACE('',(#1974),#1609,.T.);
#15703=ADVANCED_FACE('',(#1975),#1610,.T.);
#15704=ADVANCED_FACE('',(#1976),#1611,.T.);
#15705=ADVANCED_FACE('',(#1977),#1612,.T.);
#15706=ADVANCED_FACE('',(#1978),#1613,.T.);
#15707=ADVANCED_FACE('',(#1979),#1614,.T.);
#15708=ADVANCED_FACE('',(#1980),#1615,.T.);
#15709=ADVANCED_FACE('',(#1981),#1616,.T.);
#15710=ADVANCED_FACE('',(#1982),#1617,.T.);
#15711=ADVANCED_FACE('',(#1983),#1618,.T.);
#15712=ADVANCED_FACE('',(#1984),#1619,.T.);
#15713=ADVANCED_FACE('',(#1985),#1620,.T.);
#15714=ADVANCED_FACE('',(#1986),#1621,.T.);
#15715=ADVANCED_FACE('',(#1987),#1622,.T.);
#15716=ADVANCED_FACE('',(#1988),#1623,.T.);
#15717=ADVANCED_FACE('',(#1989),#1624,.T.);
#15718=ADVANCED_FACE('',(#1990),#1625,.T.);
#15719=ADVANCED_FACE('',(#1991),#1626,.T.);
#15720=ADVANCED_FACE('',(#1992),#1627,.T.);
#15721=ADVANCED_FACE('',(#1993),#1628,.T.);
#15722=ADVANCED_FACE('',(#1994),#1629,.T.);
#15723=ADVANCED_FACE('',(#1995),#1630,.T.);
#15724=ADVANCED_FACE('',(#1996),#1631,.T.);
#15725=ADVANCED_FACE('',(#1997),#1632,.T.);
#15726=ADVANCED_FACE('',(#1998),#1633,.T.);
#15727=ADVANCED_FACE('',(#1999),#1634,.T.);
#15728=ADVANCED_FACE('',(#2000),#1635,.T.);
#15729=ADVANCED_FACE('',(#2001),#1636,.T.);
#15730=ADVANCED_FACE('',(#2002),#1637,.T.);
#15731=ADVANCED_FACE('',(#2003),#1638,.T.);
#15732=ADVANCED_FACE('',(#2004),#1639,.T.);
#15733=ADVANCED_FACE('',(#2005),#1640,.T.);
#15734=ADVANCED_FACE('',(#2006),#1641,.T.);
#15735=ADVANCED_FACE('',(#2007),#1642,.T.);
#15736=ADVANCED_FACE('',(#2008),#1643,.T.);
#15737=ADVANCED_FACE('',(#2009),#1644,.T.);
#15738=ADVANCED_FACE('',(#2010),#1645,.T.);
#15739=ADVANCED_FACE('',(#2011),#1646,.T.);
#15740=ADVANCED_FACE('',(#2012),#1647,.T.);
#15741=ADVANCED_FACE('',(#2013),#1648,.T.);
#15742=ADVANCED_FACE('',(#2014),#1649,.T.);
#15743=ADVANCED_FACE('',(#2015),#1650,.T.);
#15744=ADVANCED_FACE('',(#2016),#1651,.T.);
#15745=ADVANCED_FACE('',(#2017),#1652,.T.);
#15746=ADVANCED_FACE('',(#2018),#1653,.T.);
#15747=ADVANCED_FACE('',(#2019),#1654,.T.);
#15748=ADVANCED_FACE('',(#2020),#1655,.T.);
#15749=ADVANCED_FACE('',(#2021),#1656,.T.);
#15750=ADVANCED_FACE('',(#2022),#15482,.F.);
#15751=ADVANCED_FACE('',(#2023),#1657,.F.);
#15752=ADVANCED_FACE('',(#2024,#947),#1108,.T.);
#15753=ADVANCED_FACE('',(#2025),#15483,.F.);
#15754=ADVANCED_FACE('',(#2026,#948),#1109,.T.);
#15755=ADVANCED_FACE('',(#2027),#15484,.T.);
#15756=ADVANCED_FACE('',(#2028),#15485,.T.);
#15757=ADVANCED_FACE('',(#2029,#949),#1110,.T.);
#15758=ADVANCED_FACE('',(#2030),#15486,.T.);
#15759=ADVANCED_FACE('',(#2031),#15487,.T.);
#15760=ADVANCED_FACE('',(#2032),#15488,.T.);
#15761=ADVANCED_FACE('',(#2033,#950),#1111,.T.);
#15762=ADVANCED_FACE('',(#2034),#1112,.F.);
#15763=ADVANCED_FACE('',(#2035),#853,.F.);
#15764=ADVANCED_FACE('',(#2036),#1658,.T.);
#15765=ADVANCED_FACE('',(#2037),#854,.F.);
#15766=ADVANCED_FACE('',(#2038),#1659,.T.);
#15767=ADVANCED_FACE('',(#2039),#855,.F.);
#15768=ADVANCED_FACE('',(#2040),#1113,.T.);
#15769=ADVANCED_FACE('',(#2041),#1660,.T.);
#15770=ADVANCED_FACE('',(#2042),#856,.F.);
#15771=ADVANCED_FACE('',(#2043),#1661,.T.);
#15772=ADVANCED_FACE('',(#2044),#1662,.T.);
#15773=ADVANCED_FACE('',(#2045),#1114,.T.);
#15774=ADVANCED_FACE('',(#2046),#1663,.T.);
#15775=ADVANCED_FACE('',(#2047),#1664,.T.);
#15776=ADVANCED_FACE('',(#2048),#1665,.T.);
#15777=ADVANCED_FACE('',(#2049),#15489,.F.);
#15778=ADVANCED_FACE('',(#2050,#951),#1115,.F.);
#15779=ADVANCED_FACE('',(#2051),#1666,.F.);
#15780=ADVANCED_FACE('',(#2052),#15490,.F.);
#15781=ADVANCED_FACE('',(#2053),#1667,.F.);
#15782=ADVANCED_FACE('',(#2054),#15491,.T.);
#15783=ADVANCED_FACE('',(#2055),#1668,.T.);
#15784=ADVANCED_FACE('',(#2056),#1669,.T.);
#15785=ADVANCED_FACE('',(#2057),#1116,.F.);
#15786=ADVANCED_FACE('',(#2058),#1117,.T.);
#15787=ADVANCED_FACE('',(#2059),#1670,.F.);
#15788=ADVANCED_FACE('',(#2060,#952),#1671,.T.);
#15789=ADVANCED_FACE('',(#2061,#953),#1118,.F.);
#15790=ADVANCED_FACE('',(#2062,#954),#1119,.T.);
#15791=ADVANCED_FACE('',(#2063),#1672,.F.);
#15792=ADVANCED_FACE('',(#2064,#955),#1120,.T.);
#15793=ADVANCED_FACE('',(#2065),#15492,.T.);
#15794=ADVANCED_FACE('',(#2066),#1673,.T.);
#15795=ADVANCED_FACE('',(#2067,#956),#1121,.T.);
#15796=ADVANCED_FACE('',(#2068),#15493,.T.);
#15797=ADVANCED_FACE('',(#2069),#15494,.T.);
#15798=ADVANCED_FACE('',(#2070),#1674,.F.);
#15799=ADVANCED_FACE('',(#2071),#1122,.F.);
#15800=ADVANCED_FACE('',(#2072,#957),#1123,.T.);
#15801=ADVANCED_FACE('',(#2073),#15495,.T.);
#15802=ADVANCED_FACE('',(#2074),#1675,.T.);
#15803=ADVANCED_FACE('',(#2075,#958),#1124,.T.);
#15804=ADVANCED_FACE('',(#2076),#15496,.T.);
#15805=ADVANCED_FACE('',(#2077),#1676,.T.);
#15806=ADVANCED_FACE('',(#2078,#959),#1125,.T.);
#15807=ADVANCED_FACE('',(#2079),#1677,.T.);
#15808=ADVANCED_FACE('',(#2080,#960),#1126,.T.);
#15809=ADVANCED_FACE('',(#2081),#1678,.T.);
#15810=ADVANCED_FACE('',(#2082,#961),#1127,.T.);
#15811=ADVANCED_FACE('',(#2083),#1679,.T.);
#15812=ADVANCED_FACE('',(#2084,#962),#1128,.T.);
#15813=ADVANCED_FACE('',(#2085),#1680,.T.);
#15814=ADVANCED_FACE('',(#2086),#15497,.T.);
#15815=ADVANCED_FACE('',(#2087),#1129,.T.);
#15816=ADVANCED_FACE('',(#2088),#857,.T.);
#15817=ADVANCED_FACE('',(#2089),#1130,.T.);
#15818=ADVANCED_FACE('',(#2090),#1131,.F.);
#15819=ADVANCED_FACE('',(#2091),#224,.T.);
#15820=ADVANCED_FACE('',(#2092),#1681,.F.);
#15821=ADVANCED_FACE('',(#2093,#963),#1132,.T.);
#15822=ADVANCED_FACE('',(#2094),#1682,.T.);
#15823=ADVANCED_FACE('',(#2095,#964),#1133,.T.);
#15824=ADVANCED_FACE('',(#2096),#1134,.T.);
#15825=ADVANCED_FACE('',(#2097),#15498,.T.);
#15826=ADVANCED_FACE('',(#2098),#1683,.T.);
#15827=ADVANCED_FACE('',(#2099),#15499,.T.);
#15828=ADVANCED_FACE('',(#2100),#1135,.T.);
#15829=ADVANCED_FACE('',(#2101),#1136,.T.);
#15830=ADVANCED_FACE('',(#2102),#1137,.T.);
#15831=ADVANCED_FACE('',(#2103),#1138,.T.);
#15832=ADVANCED_FACE('',(#2104),#1139,.T.);
#15833=ADVANCED_FACE('',(#2105),#1140,.T.);
#15834=ADVANCED_FACE('',(#2106),#1141,.T.);
#15835=ADVANCED_FACE('',(#2107),#1142,.T.);
#15836=ADVANCED_FACE('',(#2108),#1143,.T.);
#15837=ADVANCED_FACE('',(#2109),#1144,.T.);
#15838=ADVANCED_FACE('',(#2110),#1145,.T.);
#15839=ADVANCED_FACE('',(#2111),#1146,.T.);
#15840=ADVANCED_FACE('',(#2112),#1147,.T.);
#15841=ADVANCED_FACE('',(#2113),#1148,.T.);
#15842=ADVANCED_FACE('',(#2114),#1149,.T.);
#15843=ADVANCED_FACE('',(#2115),#1150,.T.);
#15844=ADVANCED_FACE('',(#2116),#1151,.T.);
#15845=ADVANCED_FACE('',(#2117),#1152,.T.);
#15846=ADVANCED_FACE('',(#2118),#1153,.T.);
#15847=ADVANCED_FACE('',(#2119),#1154,.T.);
#15848=ADVANCED_FACE('',(#2120),#1155,.T.);
#15849=ADVANCED_FACE('',(#2121),#1156,.T.);
#15850=ADVANCED_FACE('',(#2122),#1157,.T.);
#15851=ADVANCED_FACE('',(#2123),#1158,.T.);
#15852=ADVANCED_FACE('',(#2124),#1159,.T.);
#15853=ADVANCED_FACE('',(#2125),#1160,.T.);
#15854=ADVANCED_FACE('',(#2126,#965,#966,#967,#968,#969),#1161,.F.);
#15855=ADVANCED_FACE('',(#2127),#1162,.T.);
#15856=ADVANCED_FACE('',(#2128),#1163,.T.);
#15857=ADVANCED_FACE('',(#2129),#1164,.T.);
#15858=ADVANCED_FACE('',(#2130),#1165,.T.);
#15859=ADVANCED_FACE('',(#2131),#1166,.T.);
#15860=ADVANCED_FACE('',(#2132),#1167,.T.);
#15861=ADVANCED_FACE('',(#2133),#1168,.T.);
#15862=ADVANCED_FACE('',(#2134),#858,.F.);
#15863=ADVANCED_FACE('',(#2135),#859,.F.);
#15864=ADVANCED_FACE('',(#2136),#1169,.F.);
#15865=ADVANCED_FACE('',(#2137),#1170,.F.);
#15866=ADVANCED_FACE('',(#2138),#1171,.F.);
#15867=ADVANCED_FACE('',(#2139),#1172,.F.);
#15868=ADVANCED_FACE('',(#2140),#1173,.F.);
#15869=ADVANCED_FACE('',(#2141),#860,.F.);
#15870=ADVANCED_FACE('',(#2142),#861,.F.);
#15871=ADVANCED_FACE('',(#2143),#1174,.F.);
#15872=ADVANCED_FACE('',(#2144),#1175,.F.);
#15873=ADVANCED_FACE('',(#2145),#1176,.F.);
#15874=ADVANCED_FACE('',(#2146),#862,.F.);
#15875=ADVANCED_FACE('',(#2147),#863,.F.);
#15876=ADVANCED_FACE('',(#2148),#1177,.F.);
#15877=ADVANCED_FACE('',(#2149),#1178,.F.);
#15878=ADVANCED_FACE('',(#2150),#1179,.F.);
#15879=ADVANCED_FACE('',(#2151),#1180,.F.);
#15880=ADVANCED_FACE('',(#2152),#1181,.F.);
#15881=ADVANCED_FACE('',(#2153),#1182,.T.);
#15882=ADVANCED_FACE('',(#2154),#1183,.F.);
#15883=ADVANCED_FACE('',(#2155),#1184,.F.);
#15884=ADVANCED_FACE('',(#2156),#1185,.F.);
#15885=ADVANCED_FACE('',(#2157),#1186,.F.);
#15886=ADVANCED_FACE('',(#2158),#1187,.F.);
#15887=ADVANCED_FACE('',(#2159),#1188,.F.);
#15888=ADVANCED_FACE('',(#2160),#1189,.F.);
#15889=ADVANCED_FACE('',(#2161),#1190,.F.);
#15890=ADVANCED_FACE('',(#2162),#1191,.F.);
#15891=ADVANCED_FACE('',(#2163),#864,.F.);
#15892=ADVANCED_FACE('',(#2164),#865,.F.);
#15893=ADVANCED_FACE('',(#2165),#866,.F.);
#15894=ADVANCED_FACE('',(#2166),#867,.F.);
#15895=ADVANCED_FACE('',(#2167),#868,.F.);
#15896=ADVANCED_FACE('',(#2168),#869,.F.);
#15897=ADVANCED_FACE('',(#2169),#870,.F.);
#15898=ADVANCED_FACE('',(#2170),#871,.F.);
#15899=ADVANCED_FACE('',(#2171),#872,.F.);
#15900=ADVANCED_FACE('',(#2172),#873,.F.);
#15901=ADVANCED_FACE('',(#2173),#874,.F.);
#15902=ADVANCED_FACE('',(#2174),#875,.F.);
#15903=ADVANCED_FACE('',(#2175),#1192,.T.);
#15904=ADVANCED_FACE('',(#2176),#876,.F.);
#15905=ADVANCED_FACE('',(#2177),#877,.F.);
#15906=ADVANCED_FACE('',(#2178),#1193,.F.);
#15907=ADVANCED_FACE('',(#2179),#878,.F.);
#15908=ADVANCED_FACE('',(#2180),#879,.F.);
#15909=ADVANCED_FACE('',(#2181),#1194,.F.);
#15910=ADVANCED_FACE('',(#2182),#1195,.F.);
#15911=ADVANCED_FACE('',(#2183),#1196,.F.);
#15912=ADVANCED_FACE('',(#2184),#1197,.F.);
#15913=ADVANCED_FACE('',(#2185),#1198,.T.);
#15914=ADVANCED_FACE('',(#2186),#880,.F.);
#15915=ADVANCED_FACE('',(#2187),#881,.F.);
#15916=ADVANCED_FACE('',(#2188),#882,.F.);
#15917=ADVANCED_FACE('',(#2189),#883,.F.);
#15918=ADVANCED_FACE('',(#2190),#884,.F.);
#15919=ADVANCED_FACE('',(#2191),#885,.F.);
#15920=ADVANCED_FACE('',(#2192),#886,.F.);
#15921=ADVANCED_FACE('',(#2193),#887,.F.);
#15922=ADVANCED_FACE('',(#2194),#888,.F.);
#15923=ADVANCED_FACE('',(#2195),#889,.F.);
#15924=ADVANCED_FACE('',(#2196),#890,.F.);
#15925=ADVANCED_FACE('',(#2197),#891,.F.);
#15926=ADVANCED_FACE('',(#2198),#1199,.F.);
#15927=ADVANCED_FACE('',(#2199),#892,.F.);
#15928=ADVANCED_FACE('',(#2200),#893,.F.);
#15929=ADVANCED_FACE('',(#2201),#894,.F.);
#15930=ADVANCED_FACE('',(#2202),#895,.F.);
#15931=ADVANCED_FACE('',(#2203),#896,.F.);
#15932=ADVANCED_FACE('',(#2204),#897,.F.);
#15933=ADVANCED_FACE('',(#2205),#898,.F.);
#15934=ADVANCED_FACE('',(#2206),#899,.F.);
#15935=ADVANCED_FACE('',(#2207),#900,.F.);
#15936=ADVANCED_FACE('',(#2208),#901,.F.);
#15937=ADVANCED_FACE('',(#2209),#902,.F.);
#15938=ADVANCED_FACE('',(#2210),#1200,.F.);
#15939=ADVANCED_FACE('',(#2211),#1201,.F.);
#15940=ADVANCED_FACE('',(#2212),#1202,.F.);
#15941=ADVANCED_FACE('',(#2213),#1203,.F.);
#15942=ADVANCED_FACE('',(#2214),#1204,.F.);
#15943=ADVANCED_FACE('',(#2215),#1205,.T.);
#15944=ADVANCED_FACE('',(#2216),#1206,.T.);
#15945=ADVANCED_FACE('',(#2217),#1207,.T.);
#15946=ADVANCED_FACE('',(#2218),#1208,.T.);
#15947=ADVANCED_FACE('',(#2219),#1209,.F.);
#15948=ADVANCED_FACE('',(#2220),#1210,.T.);
#15949=ADVANCED_FACE('',(#2221),#1211,.F.);
#15950=ADVANCED_FACE('',(#2222),#1212,.F.);
#15951=ADVANCED_FACE('',(#2223),#1213,.T.);
#15952=ADVANCED_FACE('',(#2224),#15500,.T.);
#15953=ADVANCED_FACE('',(#2225),#1684,.T.);
#15954=ADVANCED_FACE('',(#2226,#970),#1214,.T.);
#15955=ADVANCED_FACE('',(#2227),#1685,.T.);
#15956=ADVANCED_FACE('',(#2228,#971),#1215,.T.);
#15957=ADVANCED_FACE('',(#2229),#1686,.T.);
#15958=ADVANCED_FACE('',(#2230,#972),#1216,.T.);
#15959=ADVANCED_FACE('',(#2231),#1687,.T.);
#15960=ADVANCED_FACE('',(#2232,#973),#1217,.T.);
#15961=ADVANCED_FACE('',(#2233),#1688,.T.);
#15962=ADVANCED_FACE('',(#2234),#15501,.T.);
#15963=ADVANCED_FACE('',(#2235),#1218,.T.);
#15964=ADVANCED_FACE('',(#2236),#1689,.T.);
#15965=ADVANCED_FACE('',(#2237),#1690,.T.);
#15966=ADVANCED_FACE('',(#2238),#1691,.T.);
#15967=ADVANCED_FACE('',(#2239),#1692,.T.);
#15968=ADVANCED_FACE('',(#2240),#1693,.T.);
#15969=ADVANCED_FACE('',(#2241),#1694,.T.);
#15970=ADVANCED_FACE('',(#2242),#1695,.T.);
#15971=ADVANCED_FACE('',(#2243),#1696,.T.);
#15972=ADVANCED_FACE('',(#2244),#1697,.T.);
#15973=ADVANCED_FACE('',(#2245),#1698,.T.);
#15974=ADVANCED_FACE('',(#2246),#1699,.T.);
#15975=ADVANCED_FACE('',(#2247),#1700,.T.);
#15976=ADVANCED_FACE('',(#2248),#1701,.T.);
#15977=ADVANCED_FACE('',(#2249),#1702,.T.);
#15978=ADVANCED_FACE('',(#2250),#1703,.T.);
#15979=ADVANCED_FACE('',(#2251),#1704,.T.);
#15980=ADVANCED_FACE('',(#2252),#1705,.T.);
#15981=ADVANCED_FACE('',(#2253),#1706,.T.);
#15982=ADVANCED_FACE('',(#2254),#1707,.T.);
#15983=ADVANCED_FACE('',(#2255),#1708,.T.);
#15984=ADVANCED_FACE('',(#2256),#1709,.T.);
#15985=ADVANCED_FACE('',(#2257),#1710,.T.);
#15986=ADVANCED_FACE('',(#2258),#1711,.T.);
#15987=ADVANCED_FACE('',(#2259),#15502,.T.);
#15988=ADVANCED_FACE('',(#2260),#15503,.T.);
#15989=ADVANCED_FACE('',(#2261,#974),#1219,.T.);
#15990=ADVANCED_FACE('',(#2262),#15504,.T.);
#15991=ADVANCED_FACE('',(#2263),#1712,.T.);
#15992=ADVANCED_FACE('',(#2264),#1220,.F.);
#15993=ADVANCED_FACE('',(#2265),#903,.F.);
#15994=ADVANCED_FACE('',(#2266),#1713,.T.);
#15995=ADVANCED_FACE('',(#2267),#904,.F.);
#15996=ADVANCED_FACE('',(#2268),#1714,.T.);
#15997=ADVANCED_FACE('',(#2269),#1715,.F.);
#15998=ADVANCED_FACE('',(#2270,#975),#1221,.T.);
#15999=ADVANCED_FACE('',(#2271),#15505,.T.);
#16000=ADVANCED_FACE('',(#2272),#15506,.T.);
#16001=ADVANCED_FACE('',(#2273,#976),#1222,.T.);
#16002=ADVANCED_FACE('',(#2274),#1716,.F.);
#16003=ADVANCED_FACE('',(#2275,#977),#1223,.T.);
#16004=ADVANCED_FACE('',(#2276),#1717,.F.);
#16005=ADVANCED_FACE('',(#2277,#978),#1224,.T.);
#16006=ADVANCED_FACE('',(#2278),#1718,.T.);
#16007=ADVANCED_FACE('',(#2279),#1719,.T.);
#16008=ADVANCED_FACE('',(#2280),#1720,.T.);
#16009=ADVANCED_FACE('',(#2281),#1721,.T.);
#16010=ADVANCED_FACE('',(#2282),#1722,.T.);
#16011=ADVANCED_FACE('',(#2283),#1723,.T.);
#16012=ADVANCED_FACE('',(#2284),#1724,.T.);
#16013=ADVANCED_FACE('',(#2285),#1725,.T.);
#16014=ADVANCED_FACE('',(#2286),#1726,.T.);
#16015=ADVANCED_FACE('',(#2287),#1727,.T.);
#16016=ADVANCED_FACE('',(#2288),#1728,.T.);
#16017=ADVANCED_FACE('',(#2289),#1729,.T.);
#16018=ADVANCED_FACE('',(#2290),#1730,.T.);
#16019=ADVANCED_FACE('',(#2291),#1731,.T.);
#16020=ADVANCED_FACE('',(#2292),#1732,.T.);
#16021=ADVANCED_FACE('',(#2293),#1733,.T.);
#16022=ADVANCED_FACE('',(#2294),#1734,.T.);
#16023=ADVANCED_FACE('',(#2295),#1735,.T.);
#16024=ADVANCED_FACE('',(#2296),#1736,.T.);
#16025=ADVANCED_FACE('',(#2297),#1737,.T.);
#16026=ADVANCED_FACE('',(#2298),#1738,.T.);
#16027=ADVANCED_FACE('',(#2299),#1739,.T.);
#16028=ADVANCED_FACE('',(#2300),#1740,.T.);
#16029=ADVANCED_FACE('',(#2301),#1741,.T.);
#16030=ADVANCED_FACE('',(#2302),#1742,.T.);
#16031=ADVANCED_FACE('',(#2303),#1743,.T.);
#16032=ADVANCED_FACE('',(#2304),#1225,.T.);
#16033=ADVANCED_FACE('',(#2305),#1226,.T.);
#16034=ADVANCED_FACE('',(#2306),#1227,.T.);
#16035=ADVANCED_FACE('',(#2307,#979,#980,#981,#982,#983,#984,#985,#986,
#987,#988,#989,#990,#991,#992,#993,#994,#995,#996,#997,#998,#999),#1744,
 .T.);
#16036=ADVANCED_FACE('',(#2308),#15507,.T.);
#16037=ADVANCED_FACE('',(#2309),#1228,.T.);
#16038=ADVANCED_FACE('',(#2310),#905,.F.);
#16039=ADVANCED_FACE('',(#2311),#1229,.T.);
#16040=ADVANCED_FACE('',(#2312),#1745,.T.);
#16041=ADVANCED_FACE('',(#2313),#906,.F.);
#16042=ADVANCED_FACE('',(#2314),#1230,.F.);
#16043=ADVANCED_FACE('',(#2315),#1231,.F.);
#16044=ADVANCED_FACE('',(#2316),#1232,.F.);
#16045=ADVANCED_FACE('',(#2317),#1233,.F.);
#16046=ADVANCED_FACE('',(#2318),#1234,.F.);
#16047=ADVANCED_FACE('',(#2319),#1235,.T.);
#16048=ADVANCED_FACE('',(#2320),#1236,.F.);
#16049=ADVANCED_FACE('',(#2321),#1237,.F.);
#16050=ADVANCED_FACE('',(#2322),#1238,.F.);
#16051=ADVANCED_FACE('',(#2323),#1239,.T.);
#16052=ADVANCED_FACE('',(#2324),#1240,.F.);
#16053=ADVANCED_FACE('',(#2325),#1241,.F.);
#16054=ADVANCED_FACE('',(#2326),#1242,.F.);
#16055=ADVANCED_FACE('',(#2327),#1243,.T.);
#16056=ADVANCED_FACE('',(#2328),#1244,.F.);
#16057=ADVANCED_FACE('',(#2329),#1245,.F.);
#16058=ADVANCED_FACE('',(#2330),#1246,.F.);
#16059=ADVANCED_FACE('',(#2331),#1247,.T.);
#16060=ADVANCED_FACE('',(#2332),#1248,.F.);
#16061=ADVANCED_FACE('',(#2333),#1249,.F.);
#16062=ADVANCED_FACE('',(#2334),#1250,.F.);
#16063=ADVANCED_FACE('',(#2335),#1251,.T.);
#16064=ADVANCED_FACE('',(#2336),#1252,.F.);
#16065=ADVANCED_FACE('',(#2337),#1253,.F.);
#16066=ADVANCED_FACE('',(#2338),#1254,.F.);
#16067=ADVANCED_FACE('',(#2339),#1255,.T.);
#16068=ADVANCED_FACE('',(#2340),#1256,.F.);
#16069=ADVANCED_FACE('',(#2341),#1257,.T.);
#16070=ADVANCED_FACE('',(#2342),#1258,.F.);
#16071=ADVANCED_FACE('',(#2343),#1259,.F.);
#16072=ADVANCED_FACE('',(#2344),#1260,.F.);
#16073=ADVANCED_FACE('',(#2345),#1261,.T.);
#16074=ADVANCED_FACE('',(#2346),#1262,.F.);
#16075=ADVANCED_FACE('',(#2347),#1263,.F.);
#16076=ADVANCED_FACE('',(#2348),#1264,.F.);
#16077=ADVANCED_FACE('',(#2349),#1265,.T.);
#16078=ADVANCED_FACE('',(#2350),#1266,.F.);
#16079=ADVANCED_FACE('',(#2351),#1267,.F.);
#16080=ADVANCED_FACE('',(#2352),#1268,.F.);
#16081=ADVANCED_FACE('',(#2353),#1269,.T.);
#16082=ADVANCED_FACE('',(#2354),#1270,.F.);
#16083=ADVANCED_FACE('',(#2355),#1271,.F.);
#16084=ADVANCED_FACE('',(#2356),#1272,.F.);
#16085=ADVANCED_FACE('',(#2357),#1273,.T.);
#16086=ADVANCED_FACE('',(#2358),#1274,.F.);
#16087=ADVANCED_FACE('',(#2359),#1275,.F.);
#16088=ADVANCED_FACE('',(#2360),#1276,.F.);
#16089=ADVANCED_FACE('',(#2361),#1277,.T.);
#16090=ADVANCED_FACE('',(#2362),#1278,.F.);
#16091=ADVANCED_FACE('',(#2363),#1279,.F.);
#16092=ADVANCED_FACE('',(#2364),#1280,.F.);
#16093=ADVANCED_FACE('',(#2365),#1281,.T.);
#16094=ADVANCED_FACE('',(#2366),#1282,.F.);
#16095=ADVANCED_FACE('',(#2367),#1283,.F.);
#16096=ADVANCED_FACE('',(#2368),#1284,.F.);
#16097=ADVANCED_FACE('',(#2369),#1285,.T.);
#16098=ADVANCED_FACE('',(#2370),#1286,.F.);
#16099=ADVANCED_FACE('',(#2371),#1287,.F.);
#16100=ADVANCED_FACE('',(#2372),#1288,.F.);
#16101=ADVANCED_FACE('',(#2373),#1289,.T.);
#16102=ADVANCED_FACE('',(#2374),#1290,.F.);
#16103=ADVANCED_FACE('',(#2375),#1291,.F.);
#16104=ADVANCED_FACE('',(#2376),#1292,.F.);
#16105=ADVANCED_FACE('',(#2377),#1293,.T.);
#16106=ADVANCED_FACE('',(#2378),#1294,.F.);
#16107=ADVANCED_FACE('',(#2379),#1295,.F.);
#16108=ADVANCED_FACE('',(#2380),#1296,.F.);
#16109=ADVANCED_FACE('',(#2381),#1297,.T.);
#16110=ADVANCED_FACE('',(#2382),#1298,.F.);
#16111=ADVANCED_FACE('',(#2383),#1299,.F.);
#16112=ADVANCED_FACE('',(#2384),#1300,.F.);
#16113=ADVANCED_FACE('',(#2385),#1301,.T.);
#16114=ADVANCED_FACE('',(#2386),#1302,.F.);
#16115=ADVANCED_FACE('',(#2387),#1303,.F.);
#16116=ADVANCED_FACE('',(#2388),#1304,.T.);
#16117=ADVANCED_FACE('',(#2389),#1305,.F.);
#16118=ADVANCED_FACE('',(#2390),#1306,.F.);
#16119=ADVANCED_FACE('',(#2391),#1307,.F.);
#16120=ADVANCED_FACE('',(#2392),#1308,.T.);
#16121=ADVANCED_FACE('',(#2393),#1309,.F.);
#16122=ADVANCED_FACE('',(#2394),#1310,.F.);
#16123=ADVANCED_FACE('',(#2395),#1311,.F.);
#16124=ADVANCED_FACE('',(#2396),#1312,.T.);
#16125=ADVANCED_FACE('',(#2397),#1313,.F.);
#16126=ADVANCED_FACE('',(#2398),#1314,.F.);
#16127=ADVANCED_FACE('',(#2399),#1315,.F.);
#16128=ADVANCED_FACE('',(#2400),#1316,.T.);
#16129=ADVANCED_FACE('',(#2401),#1317,.F.);
#16130=ADVANCED_FACE('',(#2402),#1318,.F.);
#16131=ADVANCED_FACE('',(#2403),#1319,.F.);
#16132=ADVANCED_FACE('',(#2404),#1320,.T.);
#16133=ADVANCED_FACE('',(#2405),#1321,.F.);
#16134=ADVANCED_FACE('',(#2406),#1322,.F.);
#16135=ADVANCED_FACE('',(#2407),#1323,.F.);
#16136=ADVANCED_FACE('',(#2408),#1324,.T.);
#16137=ADVANCED_FACE('',(#2409),#1325,.F.);
#16138=ADVANCED_FACE('',(#2410),#1326,.F.);
#16139=ADVANCED_FACE('',(#2411),#1327,.T.);
#16140=ADVANCED_FACE('',(#2412),#15508,.T.);
#16141=ADVANCED_FACE('',(#2413),#1746,.T.);
#16142=ADVANCED_FACE('',(#2414,#1000),#1328,.T.);
#16143=ADVANCED_FACE('',(#2415),#15509,.T.);
#16144=ADVANCED_FACE('',(#2416),#15510,.T.);
#16145=ADVANCED_FACE('',(#2417),#15511,.F.);
#16146=ADVANCED_FACE('',(#2418),#1747,.F.);
#16147=ADVANCED_FACE('',(#2419,#1001),#1329,.T.);
#16148=ADVANCED_FACE('',(#2420),#1748,.F.);
#16149=ADVANCED_FACE('',(#2421,#1002),#1330,.T.);
#16150=ADVANCED_FACE('',(#2422),#15512,.T.);
#16151=ADVANCED_FACE('',(#2423),#1749,.T.);
#16152=ADVANCED_FACE('',(#2424),#15513,.T.);
#16153=ADVANCED_FACE('',(#2425),#1331,.T.);
#16154=ADVANCED_FACE('',(#2426),#1332,.T.);
#16155=ADVANCED_FACE('',(#2427),#15514,.T.);
#16156=ADVANCED_FACE('',(#2428),#15515,.T.);
#16157=ADVANCED_FACE('',(#2429),#1333,.T.);
#16158=ADVANCED_FACE('',(#2430),#15516,.T.);
#16159=ADVANCED_FACE('',(#2431),#15517,.T.);
#16160=ADVANCED_FACE('',(#2432),#15518,.T.);
#16161=ADVANCED_FACE('',(#2433),#1750,.T.);
#16162=ADVANCED_FACE('',(#2434),#1751,.F.);
#16163=ADVANCED_FACE('',(#2435,#1003),#1334,.T.);
#16164=ADVANCED_FACE('',(#2436),#15519,.T.);
#16165=ADVANCED_FACE('',(#2437),#1335,.T.);
#16166=ADVANCED_FACE('',(#2438),#15520,.F.);
#16167=ADVANCED_FACE('',(#2439),#1752,.T.);
#16168=ADVANCED_FACE('',(#2440),#1753,.T.);
#16169=ADVANCED_FACE('',(#2441),#1754,.T.);
#16170=ADVANCED_FACE('',(#2442),#1755,.T.);
#16171=ADVANCED_FACE('',(#2443),#1756,.T.);
#16172=ADVANCED_FACE('',(#2444),#1757,.T.);
#16173=ADVANCED_FACE('',(#2445),#1758,.T.);
#16174=ADVANCED_FACE('',(#2446),#1759,.T.);
#16175=ADVANCED_FACE('',(#2447),#1760,.T.);
#16176=ADVANCED_FACE('',(#2448),#1761,.T.);
#16177=ADVANCED_FACE('',(#2449),#1762,.T.);
#16178=ADVANCED_FACE('',(#2450),#1763,.T.);
#16179=ADVANCED_FACE('',(#2451),#1764,.T.);
#16180=ADVANCED_FACE('',(#2452),#1765,.T.);
#16181=ADVANCED_FACE('',(#2453),#1766,.T.);
#16182=ADVANCED_FACE('',(#2454),#1767,.T.);
#16183=ADVANCED_FACE('',(#2455),#1768,.T.);
#16184=ADVANCED_FACE('',(#2456),#1769,.T.);
#16185=ADVANCED_FACE('',(#2457),#1770,.T.);
#16186=ADVANCED_FACE('',(#2458),#1771,.T.);
#16187=ADVANCED_FACE('',(#2459),#1772,.T.);
#16188=ADVANCED_FACE('',(#2460),#1773,.T.);
#16189=ADVANCED_FACE('',(#2461),#1774,.T.);
#16190=ADVANCED_FACE('',(#2462),#1775,.T.);
#16191=ADVANCED_FACE('',(#2463),#1776,.T.);
#16192=ADVANCED_FACE('',(#2464),#907,.F.);
#16193=ADVANCED_FACE('',(#2465),#1336,.T.);
#16194=ADVANCED_FACE('',(#2466),#1777,.T.);
#16195=ADVANCED_FACE('',(#2467),#908,.F.);
#16196=ADVANCED_FACE('',(#2468,#1004),#1337,.T.);
#16197=ADVANCED_FACE('',(#2469),#909,.F.);
#16198=ADVANCED_FACE('',(#2470),#910,.F.);
#16199=ADVANCED_FACE('',(#2471),#911,.F.);
#16200=ADVANCED_FACE('',(#2472),#912,.F.);
#16201=ADVANCED_FACE('',(#2473),#913,.F.);
#16202=ADVANCED_FACE('',(#2474),#914,.F.);
#16203=ADVANCED_FACE('',(#2475),#915,.F.);
#16204=ADVANCED_FACE('',(#2476),#916,.F.);
#16205=ADVANCED_FACE('',(#2477),#917,.F.);
#16206=ADVANCED_FACE('',(#2478),#918,.F.);
#16207=ADVANCED_FACE('',(#2479),#919,.F.);
#16208=ADVANCED_FACE('',(#2480),#1338,.T.);
#16209=ADVANCED_FACE('',(#2481),#1339,.F.);
#16210=ADVANCED_FACE('',(#2482),#1340,.F.);
#16211=ADVANCED_FACE('',(#2483),#1341,.F.);
#16212=ADVANCED_FACE('',(#2484),#1342,.F.);
#16213=ADVANCED_FACE('',(#2485),#1343,.F.);
#16214=ADVANCED_FACE('',(#2486),#1344,.F.);
#16215=ADVANCED_FACE('',(#2487),#1345,.F.);
#16216=ADVANCED_FACE('',(#2488),#1346,.F.);
#16217=ADVANCED_FACE('',(#2489),#1347,.F.);
#16218=ADVANCED_FACE('',(#2490),#1348,.F.);
#16219=ADVANCED_FACE('',(#2491),#1349,.F.);
#16220=ADVANCED_FACE('',(#2492),#920,.F.);
#16221=ADVANCED_FACE('',(#2493),#921,.F.);
#16222=ADVANCED_FACE('',(#2494),#922,.F.);
#16223=ADVANCED_FACE('',(#2495),#923,.F.);
#16224=ADVANCED_FACE('',(#2496),#924,.F.);
#16225=ADVANCED_FACE('',(#2497),#925,.F.);
#16226=ADVANCED_FACE('',(#2498),#926,.F.);
#16227=ADVANCED_FACE('',(#2499),#927,.F.);
#16228=ADVANCED_FACE('',(#2500),#928,.F.);
#16229=ADVANCED_FACE('',(#2501),#929,.F.);
#16230=ADVANCED_FACE('',(#2502),#930,.F.);
#16231=ADVANCED_FACE('',(#2503),#1350,.T.);
#16232=ADVANCED_FACE('',(#2504),#1351,.F.);
#16233=ADVANCED_FACE('',(#2505),#1352,.F.);
#16234=ADVANCED_FACE('',(#2506),#1353,.F.);
#16235=ADVANCED_FACE('',(#2507),#1354,.F.);
#16236=ADVANCED_FACE('',(#2508),#1355,.F.);
#16237=ADVANCED_FACE('',(#2509),#1356,.F.);
#16238=ADVANCED_FACE('',(#2510),#1357,.F.);
#16239=ADVANCED_FACE('',(#2511),#1358,.F.);
#16240=ADVANCED_FACE('',(#2512),#1359,.F.);
#16241=ADVANCED_FACE('',(#2513),#1360,.F.);
#16242=ADVANCED_FACE('',(#2514),#1361,.F.);
#16243=ADVANCED_FACE('',(#2515),#1362,.F.);
#16244=ADVANCED_FACE('',(#2516),#1363,.F.);
#16245=ADVANCED_FACE('',(#2517),#1364,.F.);
#16246=ADVANCED_FACE('',(#2518),#1365,.F.);
#16247=ADVANCED_FACE('',(#2519),#1366,.F.);
#16248=ADVANCED_FACE('',(#2520),#1367,.F.);
#16249=ADVANCED_FACE('',(#2521),#1368,.F.);
#16250=ADVANCED_FACE('',(#2522),#1369,.F.);
#16251=ADVANCED_FACE('',(#2523),#1370,.F.);
#16252=ADVANCED_FACE('',(#2524),#1371,.F.);
#16253=ADVANCED_FACE('',(#2525),#1372,.F.);
#16254=ADVANCED_FACE('',(#2526,#1005),#1373,.F.);
#16255=ADVANCED_FACE('',(#2527),#1778,.F.);
#16256=ADVANCED_FACE('',(#2528),#1779,.T.);
#16257=ADVANCED_FACE('',(#2529),#1374,.T.);
#16258=ADVANCED_FACE('',(#2530),#1375,.F.);
#16259=ADVANCED_FACE('',(#2531),#1376,.T.);
#16260=ADVANCED_FACE('',(#2532),#1377,.F.);
#16261=ADVANCED_FACE('',(#2533),#1378,.F.);
#16262=ADVANCED_FACE('',(#2534),#1379,.F.);
#16263=ADVANCED_FACE('',(#2535),#1380,.T.);
#16264=ADVANCED_FACE('',(#2536),#1381,.F.);
#16265=ADVANCED_FACE('',(#2537),#1382,.F.);
#16266=ADVANCED_FACE('',(#2538),#1383,.F.);
#16267=ADVANCED_FACE('',(#2539),#1384,.T.);
#16268=ADVANCED_FACE('',(#2540),#1385,.F.);
#16269=ADVANCED_FACE('',(#2541),#1386,.F.);
#16270=ADVANCED_FACE('',(#2542),#1387,.F.);
#16271=ADVANCED_FACE('',(#2543),#1388,.T.);
#16272=ADVANCED_FACE('',(#2544),#1389,.F.);
#16273=ADVANCED_FACE('',(#2545),#1390,.F.);
#16274=ADVANCED_FACE('',(#2546),#1391,.F.);
#16275=ADVANCED_FACE('',(#2547),#1392,.T.);
#16276=ADVANCED_FACE('',(#2548),#1393,.F.);
#16277=ADVANCED_FACE('',(#2549),#1394,.F.);
#16278=ADVANCED_FACE('',(#2550),#1395,.F.);
#16279=ADVANCED_FACE('',(#2551),#1396,.T.);
#16280=ADVANCED_FACE('',(#2552),#1397,.F.);
#16281=ADVANCED_FACE('',(#2553),#1398,.F.);
#16282=ADVANCED_FACE('',(#2554),#1399,.F.);
#16283=ADVANCED_FACE('',(#2555),#1400,.T.);
#16284=ADVANCED_FACE('',(#2556),#1401,.F.);
#16285=ADVANCED_FACE('',(#2557),#1402,.F.);
#16286=ADVANCED_FACE('',(#2558),#1403,.F.);
#16287=ADVANCED_FACE('',(#2559),#1404,.T.);
#16288=ADVANCED_FACE('',(#2560),#1405,.F.);
#16289=ADVANCED_FACE('',(#2561),#1406,.F.);
#16290=ADVANCED_FACE('',(#2562),#1407,.F.);
#16291=ADVANCED_FACE('',(#2563),#1408,.T.);
#16292=ADVANCED_FACE('',(#2564),#1409,.F.);
#16293=ADVANCED_FACE('',(#2565),#1410,.F.);
#16294=ADVANCED_FACE('',(#2566),#1411,.F.);
#16295=ADVANCED_FACE('',(#2567),#1412,.T.);
#16296=ADVANCED_FACE('',(#2568),#1413,.F.);
#16297=ADVANCED_FACE('',(#2569),#1414,.F.);
#16298=ADVANCED_FACE('',(#2570),#1415,.F.);
#16299=ADVANCED_FACE('',(#2571),#1416,.T.);
#16300=ADVANCED_FACE('',(#2572),#1417,.F.);
#16301=ADVANCED_FACE('',(#2573),#1418,.F.);
#16302=ADVANCED_FACE('',(#2574),#1419,.F.);
#16303=ADVANCED_FACE('',(#2575),#1420,.T.);
#16304=ADVANCED_FACE('',(#2576),#1421,.F.);
#16305=ADVANCED_FACE('',(#2577),#1422,.F.);
#16306=ADVANCED_FACE('',(#2578),#1423,.F.);
#16307=ADVANCED_FACE('',(#2579),#1424,.T.);
#16308=ADVANCED_FACE('',(#2580),#1425,.F.);
#16309=ADVANCED_FACE('',(#2581),#1426,.F.);
#16310=ADVANCED_FACE('',(#2582),#1427,.F.);
#16311=ADVANCED_FACE('',(#2583),#1428,.T.);
#16312=ADVANCED_FACE('',(#2584),#1429,.F.);
#16313=ADVANCED_FACE('',(#2585),#1430,.F.);
#16314=ADVANCED_FACE('',(#2586),#1431,.F.);
#16315=ADVANCED_FACE('',(#2587),#1432,.T.);
#16316=ADVANCED_FACE('',(#2588),#1433,.F.);
#16317=ADVANCED_FACE('',(#2589),#1434,.F.);
#16318=ADVANCED_FACE('',(#2590),#1435,.F.);
#16319=ADVANCED_FACE('',(#2591),#1436,.T.);
#16320=ADVANCED_FACE('',(#2592),#1437,.F.);
#16321=ADVANCED_FACE('',(#2593),#1438,.F.);
#16322=ADVANCED_FACE('',(#2594),#1439,.F.);
#16323=ADVANCED_FACE('',(#2595),#1440,.T.);
#16324=ADVANCED_FACE('',(#2596),#1441,.F.);
#16325=ADVANCED_FACE('',(#2597),#1442,.F.);
#16326=ADVANCED_FACE('',(#2598),#1443,.F.);
#16327=ADVANCED_FACE('',(#2599),#1444,.T.);
#16328=ADVANCED_FACE('',(#2600),#1445,.F.);
#16329=ADVANCED_FACE('',(#2601),#1446,.F.);
#16330=ADVANCED_FACE('',(#2602),#1447,.F.);
#16331=ADVANCED_FACE('',(#2603),#1448,.T.);
#16332=ADVANCED_FACE('',(#2604),#1449,.F.);
#16333=ADVANCED_FACE('',(#2605),#1450,.F.);
#16334=ADVANCED_FACE('',(#2606),#1451,.F.);
#16335=ADVANCED_FACE('',(#2607),#1452,.T.);
#16336=ADVANCED_FACE('',(#2608),#1453,.F.);
#16337=ADVANCED_FACE('',(#2609),#1454,.F.);
#16338=ADVANCED_FACE('',(#2610),#1455,.F.);
#16339=ADVANCED_FACE('',(#2611),#1456,.T.);
#16340=ADVANCED_FACE('',(#2612),#1457,.F.);
#16341=ADVANCED_FACE('',(#2613),#1458,.F.);
#16342=ADVANCED_FACE('',(#2614),#1459,.F.);
#16343=ADVANCED_FACE('',(#2615),#1460,.T.);
#16344=ADVANCED_FACE('',(#2616),#1461,.F.);
#16345=ADVANCED_FACE('',(#2617),#1462,.F.);
#16346=ADVANCED_FACE('',(#2618),#1463,.F.);
#16347=ADVANCED_FACE('',(#2619),#1464,.T.);
#16348=ADVANCED_FACE('',(#2620),#1465,.F.);
#16349=ADVANCED_FACE('',(#2621),#1466,.F.);
#16350=ADVANCED_FACE('',(#2622),#1467,.F.);
#16351=ADVANCED_FACE('',(#2623),#1468,.T.);
#16352=ADVANCED_FACE('',(#2624),#1469,.F.);
#16353=ADVANCED_FACE('',(#2625),#1470,.F.);
#16354=ADVANCED_FACE('',(#2626),#1471,.F.);
#16355=ADVANCED_FACE('',(#2627),#1472,.T.);
#16356=ADVANCED_FACE('',(#2628),#1473,.F.);
#16357=ADVANCED_FACE('',(#2629),#1474,.F.);
#16358=ADVANCED_FACE('',(#2630),#1475,.F.);
#16359=ADVANCED_FACE('',(#2631),#1476,.T.);
#16360=ADVANCED_FACE('',(#2632),#1477,.F.);
#16361=ADVANCED_FACE('',(#2633),#1478,.F.);
#16362=ADVANCED_FACE('',(#2634),#1479,.F.);
#16363=ADVANCED_FACE('',(#2635),#1480,.T.);
#16364=ADVANCED_FACE('',(#2636),#1481,.F.);
#16365=ADVANCED_FACE('',(#2637),#1482,.F.);
#16366=ADVANCED_FACE('',(#2638),#1483,.F.);
#16367=ADVANCED_FACE('',(#2639),#1484,.T.);
#16368=ADVANCED_FACE('',(#2640),#1485,.F.);
#16369=ADVANCED_FACE('',(#2641),#1486,.F.);
#16370=ADVANCED_FACE('',(#2642),#1487,.F.);
#16371=ADVANCED_FACE('',(#2643),#1488,.T.);
#16372=ADVANCED_FACE('',(#2644),#1489,.F.);
#16373=ADVANCED_FACE('',(#2645),#1490,.F.);
#16374=ADVANCED_FACE('',(#2646),#1491,.F.);
#16375=ADVANCED_FACE('',(#2647),#1492,.T.);
#16376=ADVANCED_FACE('',(#2648),#1493,.F.);
#16377=ADVANCED_FACE('',(#2649),#1494,.F.);
#16378=ADVANCED_FACE('',(#2650),#1495,.T.);
#16379=ADVANCED_FACE('',(#2651),#15521,.T.);
#16380=ADVANCED_FACE('',(#2652),#15522,.T.);
#16381=ADVANCED_FACE('',(#2653),#1780,.T.);
#16382=ADVANCED_FACE('',(#2654),#1781,.T.);
#16383=ADVANCED_FACE('',(#2655,#1006),#1496,.T.);
#16384=ADVANCED_FACE('',(#2656),#15523,.T.);
#16385=ADVANCED_FACE('',(#2657,#1007,#1008,#1009,#1010,#1011,#1012,#1013,
#1014,#1015,#1016,#1017,#1018,#1019,#1020,#1021,#1022,#1023,#1024,#1025,
#1026,#1027,#1028,#1029,#1030,#1031,#1032,#1033,#1034,#1035),#1782,.T.);
#16386=ADVANCED_FACE('',(#2658),#15524,.T.);
#16387=ADVANCED_FACE('',(#2659,#1036,#1037,#1038,#1039,#1040,#1041),#1497,
 .T.);
#16388=ADVANCED_FACE('',(#2660),#1498,.T.);
#16389=ADVANCED_FACE('',(#2661),#1499,.T.);
#16390=ADVANCED_FACE('',(#2662),#1500,.T.);
#16391=ADVANCED_FACE('',(#2663),#1501,.T.);
#16392=ADVANCED_FACE('',(#2664),#1502,.T.);
#16393=ADVANCED_FACE('',(#2665),#1503,.T.);
#16394=ADVANCED_FACE('',(#2666),#15525,.T.);
#16395=ADVANCED_FACE('',(#2667),#1504,.T.);
#16396=ADVANCED_FACE('',(#2668,#1042,#1043),#1505,.T.);
#16397=ADVANCED_FACE('',(#2669),#1506,.T.);
#16398=ADVANCED_FACE('',(#2670),#1507,.T.);
#16399=ADVANCED_FACE('',(#2671),#15526,.T.);
#16400=ADVANCED_FACE('',(#2672),#1508,.T.);
#16401=ADVANCED_FACE('',(#2673),#1509,.T.);
#16402=ADVANCED_FACE('',(#2674),#1510,.T.);
#16403=ADVANCED_FACE('',(#2675),#1511,.T.);
#16404=ADVANCED_FACE('',(#2676),#1783,.T.);
#16405=ADVANCED_FACE('',(#2677),#1512,.T.);
#16406=ADVANCED_FACE('',(#2678),#1513,.T.);
#16407=ADVANCED_FACE('',(#2679),#931,.T.);
#16408=ADVANCED_FACE('',(#2680),#932,.T.);
#16409=ADVANCED_FACE('',(#2681),#1514,.T.);
#16410=ADVANCED_FACE('',(#2682,#1044,#1045),#1515,.F.);
#16411=ADVANCED_FACE('',(#2683),#1784,.T.);
#16412=ADVANCED_FACE('',(#2684),#1516,.T.);
#16413=ADVANCED_FACE('',(#2685),#933,.T.);
#16414=ADVANCED_FACE('',(#2686),#934,.T.);
#16415=ADVANCED_FACE('',(#2687),#1785,.T.);
#16416=ADVANCED_FACE('',(#2688,#1046,#1047),#1517,.F.);
#16417=ADVANCED_FACE('',(#2689),#1518,.T.);
#16418=ADVANCED_FACE('',(#2690),#935,.T.);
#16419=ADVANCED_FACE('',(#2691),#936,.T.);
#16420=ADVANCED_FACE('',(#2692),#937,.T.);
#16421=ADVANCED_FACE('',(#2693),#1519,.T.);
#16422=ADVANCED_FACE('',(#2694),#938,.T.);
#16423=ADVANCED_FACE('',(#2695),#1786,.T.);
#16424=ADVANCED_FACE('',(#2696),#1787,.T.);
#16425=ADVANCED_FACE('',(#2697),#1788,.T.);
#16426=ADVANCED_FACE('',(#2698),#1789,.T.);
#16427=ADVANCED_FACE('',(#2699),#225,.T.);
#16428=ADVANCED_FACE('',(#2700,#1048,#1049),#1520,.T.);
#16429=ADVANCED_FACE('',(#2701),#1790,.T.);
#16430=ADVANCED_FACE('',(#2702),#226,.T.);
#16431=ADVANCED_FACE('',(#2703),#1791,.T.);
#16432=ADVANCED_FACE('',(#2704),#1521,.T.);
#16433=ADVANCED_FACE('',(#2705),#1792,.T.);
#16434=ADVANCED_FACE('',(#2706),#1793,.F.);
#16435=ADVANCED_FACE('',(#2707),#1794,.F.);
#16436=ADVANCED_FACE('',(#2708),#1795,.F.);
#16437=ADVANCED_FACE('',(#2709),#1796,.F.);
#16438=ADVANCED_FACE('',(#2710),#1797,.T.);
#16439=ADVANCED_FACE('',(#2711),#227,.T.);
#16440=ADVANCED_FACE('',(#2712),#1522,.T.);
#16441=ADVANCED_FACE('',(#2713),#1523,.F.);
#16442=ADVANCED_FACE('',(#2714),#1524,.T.);
#16443=ADVANCED_FACE('',(#2715),#1525,.T.);
#16444=ADVANCED_FACE('',(#2716),#15527,.T.);
#16445=ADVANCED_FACE('',(#2717),#15528,.T.);
#16446=ADVANCED_FACE('',(#2718),#1798,.T.);
#16447=ADVANCED_FACE('',(#2719),#15529,.T.);
#16448=ADVANCED_FACE('',(#2720,#1050),#1526,.F.);
#16449=ADVANCED_FACE('',(#2721),#228,.T.);
#16450=ADVANCED_FACE('',(#2722),#1799,.T.);
#16451=ADVANCED_FACE('',(#2723),#1527,.F.);
#16452=ADVANCED_FACE('',(#2724),#1528,.T.);
#16453=ADVANCED_FACE('',(#2725),#229,.F.);
#16454=ADVANCED_FACE('',(#2726),#1800,.F.);
#16455=ADVANCED_FACE('',(#2727),#230,.T.);
#16456=ADVANCED_FACE('',(#2728),#15530,.T.);
#16457=ADVANCED_FACE('',(#2729),#1529,.T.);
#16458=ADVANCED_FACE('',(#2730),#15531,.T.);
#16459=ADVANCED_FACE('',(#2731),#1530,.T.);
#16460=ADVANCED_FACE('',(#2732),#1531,.T.);
#16461=ADVANCED_FACE('',(#2733),#1801,.T.);
#16462=ADVANCED_FACE('',(#2734,#1051,#1052),#1532,.F.);
#16463=ADVANCED_FACE('',(#2735),#1533,.T.);
#16464=ADVANCED_FACE('',(#2736),#15532,.T.);
#16465=ADVANCED_FACE('',(#2737),#1534,.T.);
#16466=ADVANCED_FACE('',(#2738),#15533,.T.);
#16467=ADVANCED_FACE('',(#2739),#15534,.T.);
#16468=ADVANCED_FACE('',(#2740),#1535,.T.);
#16469=ADVANCED_FACE('',(#2741),#1536,.T.);
#16470=ADVANCED_FACE('',(#2742),#15535,.T.);
#16471=ADVANCED_FACE('',(#2743),#1537,.T.);
#16472=ADVANCED_FACE('',(#2744),#15536,.T.);
#16473=ADVANCED_FACE('',(#2745),#15537,.T.);
#16474=ADVANCED_FACE('',(#2746,#1053,#1054),#1538,.T.);
#16475=ADVANCED_FACE('',(#2747),#1539,.T.);
#16476=ADVANCED_FACE('',(#2748),#1802,.F.);
#16477=ADVANCED_FACE('',(#2749),#1803,.F.);
#16478=ADVANCED_FACE('',(#2750),#1804,.T.);
#16479=ADVANCED_FACE('',(#2751),#1540,.T.);
#16480=ADVANCED_FACE('',(#2752),#1541,.T.);
#16481=ADVANCED_FACE('',(#2753),#15538,.T.);
#16482=ADVANCED_FACE('',(#2754),#1805,.T.);
#16483=ADVANCED_FACE('',(#2755,#1055),#1542,.T.);
#16484=ADVANCED_FACE('',(#2756),#1806,.T.);
#16485=ADVANCED_FACE('',(#2757,#1056),#1543,.T.);
#16486=ADVANCED_FACE('',(#2758),#1807,.T.);
#16487=ADVANCED_FACE('',(#2759,#1057),#1544,.T.);
#16488=ADVANCED_FACE('',(#2760),#1808,.T.);
#16489=ADVANCED_FACE('',(#2761,#1058),#1545,.T.);
#16490=ADVANCED_FACE('',(#2762),#1809,.T.);
#16491=ADVANCED_FACE('',(#2763),#15539,.T.);
#16492=ADVANCED_FACE('',(#2764),#1546,.T.);
#16493=ADVANCED_FACE('',(#2765),#15540,.T.);
#16494=ADVANCED_FACE('',(#2766),#1547,.T.);
#16495=ADVANCED_FACE('',(#2767),#1548,.T.);
#16496=ADVANCED_FACE('',(#2768),#1549,.T.);
#16497=ADVANCED_FACE('',(#2769),#1550,.T.);
#16498=ADVANCED_FACE('',(#2770),#1810,.T.);
#16499=ADVANCED_FACE('',(#2771,#1059),#1551,.T.);
#16500=ADVANCED_FACE('',(#2772),#15541,.T.);
#16501=ADVANCED_FACE('',(#2773),#1552,.T.);
#16502=ADVANCED_FACE('',(#2774),#1553,.T.);
#16503=ADVANCED_FACE('',(#2775),#1554,.T.);
#16504=ADVANCED_FACE('',(#2776),#1555,.T.);
#16505=ADVANCED_FACE('',(#2777,#1060),#1556,.F.);
#16506=ADVANCED_FACE('',(#2778),#1811,.F.);
#16507=ADVANCED_FACE('',(#2779,#1061),#1557,.T.);
#16508=ADVANCED_FACE('',(#2780),#1558,.T.);
#16509=ADVANCED_FACE('',(#2781),#15542,.T.);
#16510=ADVANCED_FACE('',(#2782),#1812,.T.);
#16511=ADVANCED_FACE('',(#2783),#1813,.T.);
#16512=ADVANCED_FACE('',(#2784),#1559,.T.);
#16513=ADVANCED_FACE('',(#2785),#1814,.F.);
#16514=ADVANCED_FACE('',(#2786),#1560,.T.);
#16515=ADVANCED_FACE('',(#2787),#1561,.T.);
#16516=ADVANCED_FACE('',(#2788),#1562,.F.);
#16517=CLOSED_SHELL('',(#15543,#15544,#15545,#15546,#15547,#15548,#15549,
#15550,#15551,#15552,#15553,#15554,#15555,#15556,#15557,#15558,#15559,#15560,
#15561,#15562,#15563,#15564,#15565,#15566,#15567,#15568,#15569,#15570,#15571,
#15572,#15573,#15574,#15575,#15576,#15577,#15578,#15579,#15580,#15581,#15582,
#15583,#15584,#15585,#15586,#15587,#15588,#15589,#15590,#15591,#15592,#15593,
#15594,#15595,#15596,#15597,#15598,#15599,#15600,#15601,#15602,#15603,#15604,
#15605,#15606,#15607,#15608,#15609,#15610,#15611,#15612,#15613,#15614,#15615,
#15616,#15617,#15618,#15619,#15620,#15621,#15622,#15623,#15624,#15625,#15626,
#15627,#15628,#15629,#15630,#15631,#15632,#15633,#15634,#15635,#15636,#15637,
#15638,#15639,#15640,#15641,#15642,#15643,#15644,#15645,#15646,#15647,#15648,
#15649,#15650,#15651,#15652,#15653,#15654,#15655,#15656,#15657,#15658,#15659,
#15660,#15661,#15662,#15663,#15664,#15665,#15666,#15667,#15668,#15669,#15670,
#15671,#15672,#15673,#15674,#15675,#15676,#15677,#15678,#15679,#15680,#15681,
#15682,#15683,#15684,#15685,#15686,#15687,#15688,#15689,#15690,#15691,#15692,
#15693,#15694,#15695,#15696,#15697));
#16518=CLOSED_SHELL('',(#15698,#15699,#15700,#15701,#15702,#15703,#15704,
#15705,#15706,#15707,#15708,#15709,#15710,#15711,#15712,#15713,#15714,#15715,
#15716,#15717,#15718,#15719,#15720,#15721,#15722,#15723,#15724,#15725,#15726,
#15727,#15728,#15729,#15730,#15731,#15732,#15733,#15734,#15735,#15736,#15737,
#15738,#15739,#15740,#15741,#15742,#15743,#15744,#15745,#15746,#15747,#15748,
#15749,#15750,#15751,#15752,#15753,#15754,#15755,#15756,#15757,#15758,#15759,
#15760,#15761,#15762,#15763,#15764,#15765,#15766,#15767,#15768,#15769,#15770,
#15771,#15772,#15773,#15774,#15775,#15776,#15777,#15778,#15779,#15780,#15781,
#15782,#15783,#15784,#15785,#15786,#15787,#15788,#15789,#15790,#15791,#15792,
#15793,#15794,#15795,#15796,#15797));
#16519=CLOSED_SHELL('',(#15798,#15799,#15800,#15801,#15802,#15803,#15804,
#15805,#15806,#15807,#15808,#15809,#15810,#15811,#15812,#15813,#15814,#15815));
#16520=CLOSED_SHELL('',(#15816,#15817,#15818));
#16521=CLOSED_SHELL('',(#15819));
#16522=CLOSED_SHELL('',(#15820,#15821,#15822,#15823));
#16523=CLOSED_SHELL('',(#15824,#15825,#15826,#15827,#15828));
#16524=CLOSED_SHELL('',(#15829,#15830,#15831,#15832,#15833,#15834,#15835,
#15836,#15837,#15838,#15839,#15840,#15841,#15842,#15843,#15844,#15845,#15846,
#15847,#15848,#15849,#15850,#15851,#15852,#15853,#15854,#15855,#15856,#15857,
#15858,#15859,#15860,#15861,#15862,#15863,#15864,#15865,#15866,#15867,#15868,
#15869,#15870,#15871,#15872,#15873,#15874,#15875,#15876,#15877,#15878,#15879,
#15880,#15881,#15882,#15883,#15884,#15885,#15886,#15887,#15888,#15889,#15890,
#15891,#15892,#15893,#15894,#15895,#15896,#15897,#15898,#15899,#15900,#15901,
#15902,#15903,#15904,#15905,#15906,#15907,#15908,#15909,#15910,#15911,#15912,
#15913,#15914,#15915,#15916,#15917,#15918,#15919,#15920,#15921,#15922,#15923,
#15924,#15925,#15926,#15927,#15928,#15929,#15930,#15931,#15932,#15933,#15934,
#15935,#15936,#15937,#15938,#15939,#15940,#15941,#15942,#15943,#15944,#15945,
#15946,#15947,#15948,#15949,#15950));
#16525=CLOSED_SHELL('',(#15951,#15952,#15953,#15954,#15955,#15956,#15957,
#15958,#15959,#15960,#15961,#15962,#15963));
#16526=CLOSED_SHELL('',(#15964,#15965,#15966,#15967,#15968,#15969,#15970,
#15971,#15972,#15973,#15974,#15975,#15976,#15977,#15978,#15979,#15980,#15981,
#15982,#15983,#15984,#15985,#15986,#15987,#15988,#15989,#15990,#15991,#15992,
#15993,#15994,#15995,#15996,#15997,#15998,#15999,#16000,#16001,#16002,#16003,
#16004,#16005));
#16527=CLOSED_SHELL('',(#16006,#16007,#16008,#16009,#16010,#16011,#16012,
#16013,#16014,#16015,#16016,#16017,#16018,#16019,#16020,#16021,#16022,#16023,
#16024,#16025,#16026,#16027,#16028,#16029,#16030,#16031,#16032,#16033,#16034,
#16035,#16036,#16037,#16038,#16039,#16040,#16041,#16042,#16043,#16044,#16045,
#16046,#16047,#16048,#16049,#16050,#16051,#16052,#16053,#16054,#16055,#16056,
#16057,#16058,#16059,#16060,#16061,#16062,#16063,#16064,#16065,#16066,#16067,
#16068,#16069,#16070,#16071,#16072,#16073,#16074,#16075,#16076,#16077,#16078,
#16079,#16080,#16081,#16082,#16083,#16084,#16085,#16086,#16087,#16088,#16089,
#16090,#16091,#16092,#16093,#16094,#16095,#16096,#16097,#16098,#16099,#16100,
#16101,#16102,#16103,#16104,#16105,#16106,#16107,#16108,#16109,#16110,#16111,
#16112,#16113,#16114,#16115,#16116,#16117,#16118,#16119,#16120,#16121,#16122,
#16123,#16124,#16125,#16126,#16127,#16128,#16129,#16130,#16131,#16132,#16133,
#16134,#16135,#16136,#16137,#16138,#16139,#16140,#16141,#16142,#16143,#16144));
#16528=CLOSED_SHELL('',(#16145,#16146,#16147,#16148,#16149,#16150,#16151,
#16152,#16153,#16154));
#16529=CLOSED_SHELL('',(#16155,#16156,#16157,#16158,#16159,#16160,#16161,
#16162,#16163,#16164,#16165,#16166));
#16530=CLOSED_SHELL('',(#16167,#16168,#16169,#16170,#16171,#16172,#16173,
#16174,#16175,#16176,#16177,#16178,#16179,#16180,#16181,#16182,#16183,#16184,
#16185,#16186,#16187,#16188,#16189,#16190,#16191,#16192,#16193,#16194,#16195,
#16196,#16197,#16198,#16199,#16200,#16201,#16202,#16203,#16204,#16205,#16206,
#16207,#16208,#16209,#16210,#16211,#16212,#16213,#16214,#16215,#16216,#16217,
#16218,#16219,#16220,#16221,#16222,#16223,#16224,#16225,#16226,#16227,#16228,
#16229,#16230,#16231,#16232,#16233,#16234,#16235,#16236,#16237,#16238,#16239,
#16240,#16241,#16242,#16243,#16244,#16245,#16246,#16247,#16248,#16249,#16250,
#16251,#16252,#16253,#16254,#16255,#16256,#16257,#16258,#16259,#16260,#16261,
#16262,#16263,#16264,#16265,#16266,#16267,#16268,#16269,#16270,#16271,#16272,
#16273,#16274,#16275,#16276,#16277,#16278,#16279,#16280,#16281,#16282,#16283,
#16284,#16285,#16286,#16287,#16288,#16289,#16290,#16291,#16292,#16293,#16294,
#16295,#16296,#16297,#16298,#16299,#16300,#16301,#16302,#16303,#16304,#16305,
#16306,#16307,#16308,#16309,#16310,#16311,#16312,#16313,#16314,#16315,#16316,
#16317,#16318,#16319,#16320,#16321,#16322,#16323,#16324,#16325,#16326,#16327,
#16328,#16329,#16330,#16331,#16332,#16333,#16334,#16335,#16336,#16337,#16338,
#16339,#16340,#16341,#16342,#16343,#16344,#16345,#16346,#16347,#16348,#16349,
#16350,#16351,#16352,#16353,#16354,#16355,#16356,#16357,#16358,#16359,#16360,
#16361,#16362,#16363,#16364,#16365,#16366,#16367,#16368,#16369,#16370,#16371,
#16372,#16373,#16374,#16375,#16376,#16377,#16378,#16379,#16380,#16381,#16382,
#16383,#16384,#16385,#16386,#16387));
#16531=CLOSED_SHELL('',(#16388,#16389,#16390,#16391,#16392,#16393,#16394,
#16395,#16396,#16397,#16398,#16399,#16400,#16401,#16402,#16403,#16404,#16405,
#16406,#16407,#16408,#16409,#16410,#16411,#16412,#16413,#16414,#16415,#16416,
#16417,#16418,#16419,#16420,#16421,#16422,#16423,#16424,#16425,#16426,#16427,
#16428,#16429,#16430,#16431,#16432,#16433,#16434,#16435,#16436,#16437,#16438,
#16439,#16440,#16441,#16442,#16443));
#16532=CLOSED_SHELL('',(#16444,#16445,#16446,#16447,#16448,#16449,#16450,
#16451,#16452,#16453,#16454,#16455));
#16533=CLOSED_SHELL('',(#16456,#16457,#16458,#16459,#16460,#16461,#16462,
#16463,#16464,#16465,#16466,#16467,#16468,#16469,#16470,#16471,#16472,#16473,
#16474,#16475,#16476,#16477,#16478,#16479));
#16534=CLOSED_SHELL('',(#16480,#16481,#16482,#16483,#16484,#16485,#16486,
#16487,#16488,#16489,#16490,#16491,#16492));
#16535=CLOSED_SHELL('',(#16493,#16494,#16495,#16496,#16497,#16498,#16499,
#16500,#16501,#16502,#16503,#16504,#16505,#16506,#16507,#16508,#16509,#16510));
#16536=CLOSED_SHELL('',(#16511,#16512,#16513,#16514,#16515,#16516));
#16537=DERIVED_UNIT_ELEMENT(#16577,1.);
#16538=DERIVED_UNIT_ELEMENT(#45238,-3.);
#16539=DERIVED_UNIT_ELEMENT(#16577,1.);
#16540=DERIVED_UNIT_ELEMENT(#45238,-3.);
#16541=DERIVED_UNIT_ELEMENT(#16577,1.);
#16542=DERIVED_UNIT_ELEMENT(#45238,-3.);
#16543=DERIVED_UNIT_ELEMENT(#16577,1.);
#16544=DERIVED_UNIT_ELEMENT(#45238,-3.);
#16545=DERIVED_UNIT_ELEMENT(#16577,1.);
#16546=DERIVED_UNIT_ELEMENT(#45238,-3.);
#16547=DERIVED_UNIT_ELEMENT(#16577,1.);
#16548=DERIVED_UNIT_ELEMENT(#45238,-3.);
#16549=DERIVED_UNIT_ELEMENT(#16577,1.);
#16550=DERIVED_UNIT_ELEMENT(#45238,-3.);
#16551=DERIVED_UNIT_ELEMENT(#16577,1.);
#16552=DERIVED_UNIT_ELEMENT(#45238,-3.);
#16553=DERIVED_UNIT_ELEMENT(#16577,1.);
#16554=DERIVED_UNIT_ELEMENT(#45238,-3.);
#16555=DERIVED_UNIT_ELEMENT(#16577,1.);
#16556=DERIVED_UNIT_ELEMENT(#45238,-3.);
#16557=DERIVED_UNIT_ELEMENT(#16577,1.);
#16558=DERIVED_UNIT_ELEMENT(#45238,-3.);
#16559=DERIVED_UNIT_ELEMENT(#16577,1.);
#16560=DERIVED_UNIT_ELEMENT(#45238,-3.);
#16561=DERIVED_UNIT_ELEMENT(#16577,1.);
#16562=DERIVED_UNIT_ELEMENT(#45238,-3.);
#16563=DERIVED_UNIT_ELEMENT(#16577,1.);
#16564=DERIVED_UNIT_ELEMENT(#45238,-3.);
#16565=DERIVED_UNIT_ELEMENT(#16577,1.);
#16566=DERIVED_UNIT_ELEMENT(#45238,-3.);
#16567=DERIVED_UNIT_ELEMENT(#16577,1.);
#16568=DERIVED_UNIT_ELEMENT(#45238,-3.);
#16569=DERIVED_UNIT_ELEMENT(#16577,1.);
#16570=DERIVED_UNIT_ELEMENT(#45238,-3.);
#16571=DERIVED_UNIT_ELEMENT(#16577,1.);
#16572=DERIVED_UNIT_ELEMENT(#45238,-3.);
#16573=DERIVED_UNIT_ELEMENT(#16577,1.);
#16574=DERIVED_UNIT_ELEMENT(#45238,-3.);
#16575=DERIVED_UNIT_ELEMENT(#16577,1.);
#16576=DERIVED_UNIT_ELEMENT(#45238,-3.);
#16577=(
MASS_UNIT()
NAMED_UNIT(*)
SI_UNIT(.KILO.,.GRAM.)
);
#16578=DERIVED_UNIT((#16537,#16538));
#16579=DERIVED_UNIT((#16539,#16540));
#16580=DERIVED_UNIT((#16541,#16542));
#16581=DERIVED_UNIT((#16543,#16544));
#16582=DERIVED_UNIT((#16545,#16546));
#16583=DERIVED_UNIT((#16547,#16548));
#16584=DERIVED_UNIT((#16549,#16550));
#16585=DERIVED_UNIT((#16551,#16552));
#16586=DERIVED_UNIT((#16553,#16554));
#16587=DERIVED_UNIT((#16555,#16556));
#16588=DERIVED_UNIT((#16557,#16558));
#16589=DERIVED_UNIT((#16559,#16560));
#16590=DERIVED_UNIT((#16561,#16562));
#16591=DERIVED_UNIT((#16563,#16564));
#16592=DERIVED_UNIT((#16565,#16566));
#16593=DERIVED_UNIT((#16567,#16568));
#16594=DERIVED_UNIT((#16569,#16570));
#16595=DERIVED_UNIT((#16571,#16572));
#16596=DERIVED_UNIT((#16573,#16574));
#16597=DERIVED_UNIT((#16575,#16576));
#16598=MEASURE_REPRESENTATION_ITEM('density measure',
POSITIVE_RATIO_MEASURE(7850.),#16578);
#16599=MEASURE_REPRESENTATION_ITEM('density measure',
POSITIVE_RATIO_MEASURE(7850.),#16579);
#16600=MEASURE_REPRESENTATION_ITEM('density measure',
POSITIVE_RATIO_MEASURE(7850.),#16580);
#16601=MEASURE_REPRESENTATION_ITEM('density measure',
POSITIVE_RATIO_MEASURE(7850.),#16581);
#16602=MEASURE_REPRESENTATION_ITEM('density measure',
POSITIVE_RATIO_MEASURE(7850.),#16582);
#16603=MEASURE_REPRESENTATION_ITEM('density measure',
POSITIVE_RATIO_MEASURE(7850.),#16583);
#16604=MEASURE_REPRESENTATION_ITEM('density measure',
POSITIVE_RATIO_MEASURE(7850.),#16584);
#16605=MEASURE_REPRESENTATION_ITEM('density measure',
POSITIVE_RATIO_MEASURE(7850.),#16585);
#16606=MEASURE_REPRESENTATION_ITEM('density measure',
POSITIVE_RATIO_MEASURE(7850.),#16586);
#16607=MEASURE_REPRESENTATION_ITEM('density measure',
POSITIVE_RATIO_MEASURE(7850.),#16587);
#16608=MEASURE_REPRESENTATION_ITEM('density measure',
POSITIVE_RATIO_MEASURE(7850.),#16588);
#16609=MEASURE_REPRESENTATION_ITEM('density measure',
POSITIVE_RATIO_MEASURE(7850.),#16589);
#16610=MEASURE_REPRESENTATION_ITEM('density measure',
POSITIVE_RATIO_MEASURE(7850.),#16590);
#16611=MEASURE_REPRESENTATION_ITEM('density measure',
POSITIVE_RATIO_MEASURE(7850.),#16591);
#16612=MEASURE_REPRESENTATION_ITEM('density measure',
POSITIVE_RATIO_MEASURE(7850.),#16592);
#16613=MEASURE_REPRESENTATION_ITEM('density measure',
POSITIVE_RATIO_MEASURE(7850.),#16593);
#16614=MEASURE_REPRESENTATION_ITEM('density measure',
POSITIVE_RATIO_MEASURE(7850.),#16594);
#16615=MEASURE_REPRESENTATION_ITEM('density measure',
POSITIVE_RATIO_MEASURE(7850.),#16595);
#16616=MEASURE_REPRESENTATION_ITEM('density measure',
POSITIVE_RATIO_MEASURE(7850.),#16596);
#16617=MEASURE_REPRESENTATION_ITEM('density measure',
POSITIVE_RATIO_MEASURE(7850.),#16597);
#16618=PROPERTY_DEFINITION_REPRESENTATION(#16718,#16658);
#16619=PROPERTY_DEFINITION_REPRESENTATION(#16719,#16659);
#16620=PROPERTY_DEFINITION_REPRESENTATION(#16720,#16660);
#16621=PROPERTY_DEFINITION_REPRESENTATION(#16721,#16661);
#16622=PROPERTY_DEFINITION_REPRESENTATION(#16722,#16662);
#16623=PROPERTY_DEFINITION_REPRESENTATION(#16723,#16663);
#16624=PROPERTY_DEFINITION_REPRESENTATION(#16724,#16664);
#16625=PROPERTY_DEFINITION_REPRESENTATION(#16725,#16665);
#16626=PROPERTY_DEFINITION_REPRESENTATION(#16726,#16666);
#16627=PROPERTY_DEFINITION_REPRESENTATION(#16727,#16667);
#16628=PROPERTY_DEFINITION_REPRESENTATION(#16728,#16668);
#16629=PROPERTY_DEFINITION_REPRESENTATION(#16729,#16669);
#16630=PROPERTY_DEFINITION_REPRESENTATION(#16730,#16670);
#16631=PROPERTY_DEFINITION_REPRESENTATION(#16731,#16671);
#16632=PROPERTY_DEFINITION_REPRESENTATION(#16732,#16672);
#16633=PROPERTY_DEFINITION_REPRESENTATION(#16733,#16673);
#16634=PROPERTY_DEFINITION_REPRESENTATION(#16734,#16674);
#16635=PROPERTY_DEFINITION_REPRESENTATION(#16735,#16675);
#16636=PROPERTY_DEFINITION_REPRESENTATION(#16736,#16676);
#16637=PROPERTY_DEFINITION_REPRESENTATION(#16737,#16677);
#16638=PROPERTY_DEFINITION_REPRESENTATION(#16738,#16678);
#16639=PROPERTY_DEFINITION_REPRESENTATION(#16739,#16679);
#16640=PROPERTY_DEFINITION_REPRESENTATION(#16740,#16680);
#16641=PROPERTY_DEFINITION_REPRESENTATION(#16741,#16681);
#16642=PROPERTY_DEFINITION_REPRESENTATION(#16742,#16682);
#16643=PROPERTY_DEFINITION_REPRESENTATION(#16743,#16683);
#16644=PROPERTY_DEFINITION_REPRESENTATION(#16744,#16684);
#16645=PROPERTY_DEFINITION_REPRESENTATION(#16745,#16685);
#16646=PROPERTY_DEFINITION_REPRESENTATION(#16746,#16686);
#16647=PROPERTY_DEFINITION_REPRESENTATION(#16747,#16687);
#16648=PROPERTY_DEFINITION_REPRESENTATION(#16748,#16688);
#16649=PROPERTY_DEFINITION_REPRESENTATION(#16749,#16689);
#16650=PROPERTY_DEFINITION_REPRESENTATION(#16750,#16690);
#16651=PROPERTY_DEFINITION_REPRESENTATION(#16751,#16691);
#16652=PROPERTY_DEFINITION_REPRESENTATION(#16752,#16692);
#16653=PROPERTY_DEFINITION_REPRESENTATION(#16753,#16693);
#16654=PROPERTY_DEFINITION_REPRESENTATION(#16754,#16694);
#16655=PROPERTY_DEFINITION_REPRESENTATION(#16755,#16695);
#16656=PROPERTY_DEFINITION_REPRESENTATION(#16756,#16696);
#16657=PROPERTY_DEFINITION_REPRESENTATION(#16757,#16697);
#16658=REPRESENTATION('material name',(#16698),#45216);
#16659=REPRESENTATION('density',(#16598),#45216);
#16660=REPRESENTATION('material name',(#16699),#45217);
#16661=REPRESENTATION('density',(#16599),#45217);
#16662=REPRESENTATION('material name',(#16700),#45218);
#16663=REPRESENTATION('density',(#16600),#45218);
#16664=REPRESENTATION('material name',(#16701),#45219);
#16665=REPRESENTATION('density',(#16601),#45219);
#16666=REPRESENTATION('material name',(#16702),#45220);
#16667=REPRESENTATION('density',(#16602),#45220);
#16668=REPRESENTATION('material name',(#16703),#45221);
#16669=REPRESENTATION('density',(#16603),#45221);
#16670=REPRESENTATION('material name',(#16704),#45222);
#16671=REPRESENTATION('density',(#16604),#45222);
#16672=REPRESENTATION('material name',(#16705),#45223);
#16673=REPRESENTATION('density',(#16605),#45223);
#16674=REPRESENTATION('material name',(#16706),#45224);
#16675=REPRESENTATION('density',(#16606),#45224);
#16676=REPRESENTATION('material name',(#16707),#45225);
#16677=REPRESENTATION('density',(#16607),#45225);
#16678=REPRESENTATION('material name',(#16708),#45226);
#16679=REPRESENTATION('density',(#16608),#45226);
#16680=REPRESENTATION('material name',(#16709),#45227);
#16681=REPRESENTATION('density',(#16609),#45227);
#16682=REPRESENTATION('material name',(#16710),#45228);
#16683=REPRESENTATION('density',(#16610),#45228);
#16684=REPRESENTATION('material name',(#16711),#45229);
#16685=REPRESENTATION('density',(#16611),#45229);
#16686=REPRESENTATION('material name',(#16712),#45230);
#16687=REPRESENTATION('density',(#16612),#45230);
#16688=REPRESENTATION('material name',(#16713),#45231);
#16689=REPRESENTATION('density',(#16613),#45231);
#16690=REPRESENTATION('material name',(#16714),#45232);
#16691=REPRESENTATION('density',(#16614),#45232);
#16692=REPRESENTATION('material name',(#16715),#45233);
#16693=REPRESENTATION('density',(#16615),#45233);
#16694=REPRESENTATION('material name',(#16716),#45234);
#16695=REPRESENTATION('density',(#16616),#45234);
#16696=REPRESENTATION('material name',(#16717),#45235);
#16697=REPRESENTATION('density',(#16617),#45235);
#16698=DESCRIPTIVE_REPRESENTATION_ITEM('Steel','Steel');
#16699=DESCRIPTIVE_REPRESENTATION_ITEM('Steel','Steel');
#16700=DESCRIPTIVE_REPRESENTATION_ITEM('Steel','Steel');
#16701=DESCRIPTIVE_REPRESENTATION_ITEM('Steel','Steel');
#16702=DESCRIPTIVE_REPRESENTATION_ITEM('Steel','Steel');
#16703=DESCRIPTIVE_REPRESENTATION_ITEM('Steel','Steel');
#16704=DESCRIPTIVE_REPRESENTATION_ITEM('Steel','Steel');
#16705=DESCRIPTIVE_REPRESENTATION_ITEM('Steel','Steel');
#16706=DESCRIPTIVE_REPRESENTATION_ITEM('Steel','Steel');
#16707=DESCRIPTIVE_REPRESENTATION_ITEM('Steel','Steel');
#16708=DESCRIPTIVE_REPRESENTATION_ITEM('Steel','Steel');
#16709=DESCRIPTIVE_REPRESENTATION_ITEM('Steel','Steel');
#16710=DESCRIPTIVE_REPRESENTATION_ITEM('Steel','Steel');
#16711=DESCRIPTIVE_REPRESENTATION_ITEM('Steel','Steel');
#16712=DESCRIPTIVE_REPRESENTATION_ITEM('Steel','Steel');
#16713=DESCRIPTIVE_REPRESENTATION_ITEM('Steel','Steel');
#16714=DESCRIPTIVE_REPRESENTATION_ITEM('Steel','Steel');
#16715=DESCRIPTIVE_REPRESENTATION_ITEM('Steel','Steel');
#16716=DESCRIPTIVE_REPRESENTATION_ITEM('Steel','Steel');
#16717=DESCRIPTIVE_REPRESENTATION_ITEM('Steel','Steel');
#16718=PROPERTY_DEFINITION('material property','material name',#45336);
#16719=PROPERTY_DEFINITION('material property','density of part',#45336);
#16720=PROPERTY_DEFINITION('material property','material name',#45337);
#16721=PROPERTY_DEFINITION('material property','density of part',#45337);
#16722=PROPERTY_DEFINITION('material property','material name',#45338);
#16723=PROPERTY_DEFINITION('material property','density of part',#45338);
#16724=PROPERTY_DEFINITION('material property','material name',#45339);
#16725=PROPERTY_DEFINITION('material property','density of part',#45339);
#16726=PROPERTY_DEFINITION('material property','material name',#45340);
#16727=PROPERTY_DEFINITION('material property','density of part',#45340);
#16728=PROPERTY_DEFINITION('material property','material name',#45341);
#16729=PROPERTY_DEFINITION('material property','density of part',#45341);
#16730=PROPERTY_DEFINITION('material property','material name',#45342);
#16731=PROPERTY_DEFINITION('material property','density of part',#45342);
#16732=PROPERTY_DEFINITION('material property','material name',#45343);
#16733=PROPERTY_DEFINITION('material property','density of part',#45343);
#16734=PROPERTY_DEFINITION('material property','material name',#45344);
#16735=PROPERTY_DEFINITION('material property','density of part',#45344);
#16736=PROPERTY_DEFINITION('material property','material name',#45345);
#16737=PROPERTY_DEFINITION('material property','density of part',#45345);
#16738=PROPERTY_DEFINITION('material property','material name',#45346);
#16739=PROPERTY_DEFINITION('material property','density of part',#45346);
#16740=PROPERTY_DEFINITION('material property','material name',#45347);
#16741=PROPERTY_DEFINITION('material property','density of part',#45347);
#16742=PROPERTY_DEFINITION('material property','material name',#45348);
#16743=PROPERTY_DEFINITION('material property','density of part',#45348);
#16744=PROPERTY_DEFINITION('material property','material name',#45349);
#16745=PROPERTY_DEFINITION('material property','density of part',#45349);
#16746=PROPERTY_DEFINITION('material property','material name',#45350);
#16747=PROPERTY_DEFINITION('material property','density of part',#45350);
#16748=PROPERTY_DEFINITION('material property','material name',#45351);
#16749=PROPERTY_DEFINITION('material property','density of part',#45351);
#16750=PROPERTY_DEFINITION('material property','material name',#45352);
#16751=PROPERTY_DEFINITION('material property','density of part',#45352);
#16752=PROPERTY_DEFINITION('material property','material name',#45353);
#16753=PROPERTY_DEFINITION('material property','density of part',#45353);
#16754=PROPERTY_DEFINITION('material property','material name',#45354);
#16755=PROPERTY_DEFINITION('material property','density of part',#45354);
#16756=PROPERTY_DEFINITION('material property','material name',#45355);
#16757=PROPERTY_DEFINITION('material property','density of part',#45355);
#16758=AXIS2_PLACEMENT_3D('',#22164,#18123,#18124);
#16759=AXIS2_PLACEMENT_3D('',#22165,#18125,#18126);
#16760=AXIS2_PLACEMENT_3D('',#22166,#18127,#18128);
#16761=AXIS2_PLACEMENT_3D('',#22169,#18129,#18130);
#16762=AXIS2_PLACEMENT_3D('',#22170,#18131,#18132);
#16763=AXIS2_PLACEMENT_3D('',#22173,#18134,#18135);
#16764=AXIS2_PLACEMENT_3D('',#22174,#18136,#18137);
#16765=AXIS2_PLACEMENT_3D('',#22176,#18138,#18139);
#16766=AXIS2_PLACEMENT_3D('',#22178,#18141,#18142);
#16767=AXIS2_PLACEMENT_3D('',#22180,#18143,#18144);
#16768=AXIS2_PLACEMENT_3D('',#22181,#18145,#18146);
#16769=AXIS2_PLACEMENT_3D('',#22183,#18147,#18148);
#16770=AXIS2_PLACEMENT_3D('',#22185,#18150,#18151);
#16771=AXIS2_PLACEMENT_3D('',#22188,#18152,#18153);
#16772=AXIS2_PLACEMENT_3D('',#22196,#18157,#18158);
#16773=AXIS2_PLACEMENT_3D('',#22202,#18161,#18162);
#16774=AXIS2_PLACEMENT_3D('',#22382,#18167,#18168);
#16775=AXIS2_PLACEMENT_3D('',#22385,#18169,#18170);
#16776=AXIS2_PLACEMENT_3D('',#22388,#18173,#18174);
#16777=AXIS2_PLACEMENT_3D('',#22404,#18182,#18183);
#16778=AXIS2_PLACEMENT_3D('',#22408,#18185,#18186);
#16779=AXIS2_PLACEMENT_3D('',#22414,#18190,#18191);
#16780=AXIS2_PLACEMENT_3D('',#22417,#18193,#18194);
#16781=AXIS2_PLACEMENT_3D('',#22418,#18195,#18196);
#16782=AXIS2_PLACEMENT_3D('',#22420,#18197,#18198);
#16783=AXIS2_PLACEMENT_3D('',#22793,#18207,#18208);
#16784=AXIS2_PLACEMENT_3D('',#22931,#18216,#18217);
#16785=AXIS2_PLACEMENT_3D('',#22935,#18219,#18220);
#16786=AXIS2_PLACEMENT_3D('',#22937,#18222,#18223);
#16787=AXIS2_PLACEMENT_3D('',#22943,#18227,#18228);
#16788=AXIS2_PLACEMENT_3D('',#22946,#18230,#18231);
#16789=AXIS2_PLACEMENT_3D('',#22947,#18232,#18233);
#16790=AXIS2_PLACEMENT_3D('',#22951,#18236,#18237);
#16791=AXIS2_PLACEMENT_3D('',#22954,#18238,#18239);
#16792=AXIS2_PLACEMENT_3D('',#22958,#18241,#18242);
#16793=AXIS2_PLACEMENT_3D('',#22960,#18244,#18245);
#16794=AXIS2_PLACEMENT_3D('',#22962,#18246,#18247);
#16795=AXIS2_PLACEMENT_3D('',#22963,#18248,#18249);
#16796=AXIS2_PLACEMENT_3D('',#22964,#18250,#18251);
#16797=AXIS2_PLACEMENT_3D('',#22965,#18252,#18253);
#16798=AXIS2_PLACEMENT_3D('',#22966,#18254,#18255);
#16799=AXIS2_PLACEMENT_3D('',#22967,#18256,#18257);
#16800=AXIS2_PLACEMENT_3D('',#22984,#18260,#18261);
#16801=AXIS2_PLACEMENT_3D('',#22999,#18264,#18265);
#16802=AXIS2_PLACEMENT_3D('',#23003,#18268,#18269);
#16803=AXIS2_PLACEMENT_3D('',#23005,#18270,#18271);
#16804=AXIS2_PLACEMENT_3D('',#23007,#18272,#18273);
#16805=AXIS2_PLACEMENT_3D('',#23008,#18274,#18275);
#16806=AXIS2_PLACEMENT_3D('',#23009,#18276,#18277);
#16807=AXIS2_PLACEMENT_3D('',#23020,#18279,#18280);
#16808=AXIS2_PLACEMENT_3D('',#23037,#18283,#18284);
#16809=AXIS2_PLACEMENT_3D('',#23040,#18285,#18286);
#16810=AXIS2_PLACEMENT_3D('',#23041,#18287,#18288);
#16811=AXIS2_PLACEMENT_3D('',#23042,#18289,#18290);
#16812=AXIS2_PLACEMENT_3D('',#23043,#18291,#18292);
#16813=AXIS2_PLACEMENT_3D('',#23045,#18293,#18294);
#16814=AXIS2_PLACEMENT_3D('',#23046,#18295,#18296);
#16815=AXIS2_PLACEMENT_3D('',#23047,#18297,#18298);
#16816=AXIS2_PLACEMENT_3D('',#23049,#18300,#18301);
#16817=AXIS2_PLACEMENT_3D('',#23051,#18303,#18304);
#16818=AXIS2_PLACEMENT_3D('',#23054,#18305,#18306);
#16819=AXIS2_PLACEMENT_3D('',#23056,#18307,#18308);
#16820=AXIS2_PLACEMENT_3D('',#23057,#18309,#18310);
#16821=AXIS2_PLACEMENT_3D('',#23058,#18311,#18312);
#16822=AXIS2_PLACEMENT_3D('',#23061,#18313,#18314);
#16823=AXIS2_PLACEMENT_3D('',#23062,#18315,#18316);
#16824=AXIS2_PLACEMENT_3D('',#23063,#18317,#18318);
#16825=AXIS2_PLACEMENT_3D('',#23064,#18319,#18320);
#16826=AXIS2_PLACEMENT_3D('',#23067,#18323,#18324);
#16827=AXIS2_PLACEMENT_3D('',#23070,#18327,#18328);
#16828=AXIS2_PLACEMENT_3D('',#23072,#18329,#18330);
#16829=AXIS2_PLACEMENT_3D('',#23073,#18331,#18332);
#16830=AXIS2_PLACEMENT_3D('',#23074,#18333,#18334);
#16831=AXIS2_PLACEMENT_3D('',#23076,#18335,#18336);
#16832=AXIS2_PLACEMENT_3D('',#23077,#18337,#18338);
#16833=AXIS2_PLACEMENT_3D('',#23078,#18339,#18340);
#16834=AXIS2_PLACEMENT_3D('',#23079,#18341,#18342);
#16835=AXIS2_PLACEMENT_3D('',#23081,#18344,#18345);
#16836=AXIS2_PLACEMENT_3D('',#23084,#18348,#18349);
#16837=AXIS2_PLACEMENT_3D('',#23086,#18350,#18351);
#16838=AXIS2_PLACEMENT_3D('',#23087,#18352,#18353);
#16839=AXIS2_PLACEMENT_3D('',#23088,#18354,#18355);
#16840=AXIS2_PLACEMENT_3D('',#23089,#18356,#18357);
#16841=AXIS2_PLACEMENT_3D('',#23091,#18358,#18359);
#16842=AXIS2_PLACEMENT_3D('',#23093,#18361,#18362);
#16843=AXIS2_PLACEMENT_3D('',#23095,#18363,#18364);
#16844=AXIS2_PLACEMENT_3D('',#23096,#18365,#18366);
#16845=AXIS2_PLACEMENT_3D('',#23097,#18367,#18368);
#16846=AXIS2_PLACEMENT_3D('',#23098,#18369,#18370);
#16847=AXIS2_PLACEMENT_3D('',#23099,#18371,#18372);
#16848=AXIS2_PLACEMENT_3D('',#23101,#18374,#18375);
#16849=AXIS2_PLACEMENT_3D('',#23104,#18376,#18377);
#16850=AXIS2_PLACEMENT_3D('',#23106,#18378,#18379);
#16851=AXIS2_PLACEMENT_3D('',#23107,#18380,#18381);
#16852=AXIS2_PLACEMENT_3D('',#23108,#18382,#18383);
#16853=AXIS2_PLACEMENT_3D('',#23111,#18386,#18387);
#16854=AXIS2_PLACEMENT_3D('',#23112,#18388,#18389);
#16855=AXIS2_PLACEMENT_3D('',#23113,#18390,#18391);
#16856=AXIS2_PLACEMENT_3D('',#23259,#18411,#18412);
#16857=AXIS2_PLACEMENT_3D('',#23261,#18414,#18415);
#16858=AXIS2_PLACEMENT_3D('',#23262,#18416,#18417);
#16859=AXIS2_PLACEMENT_3D('',#23263,#18418,#18419);
#16860=AXIS2_PLACEMENT_3D('',#23266,#18421,#18422);
#16861=AXIS2_PLACEMENT_3D('',#23267,#18423,#18424);
#16862=AXIS2_PLACEMENT_3D('',#23269,#18426,#18427);
#16863=AXIS2_PLACEMENT_3D('',#23271,#18429,#18430);
#16864=AXIS2_PLACEMENT_3D('',#23275,#18432,#18433);
#16865=AXIS2_PLACEMENT_3D('',#23277,#18435,#18436);
#16866=AXIS2_PLACEMENT_3D('',#23278,#18437,#18438);
#16867=AXIS2_PLACEMENT_3D('',#23293,#18440,#18441);
#16868=AXIS2_PLACEMENT_3D('',#23294,#18442,#18443);
#16869=AXIS2_PLACEMENT_3D('',#23295,#18444,#18445);
#16870=AXIS2_PLACEMENT_3D('',#23296,#18446,#18447);
#16871=AXIS2_PLACEMENT_3D('',#23297,#18448,#18449);
#16872=AXIS2_PLACEMENT_3D('',#23314,#18451,#18452);
#16873=AXIS2_PLACEMENT_3D('',#23329,#18453,#18454);
#16874=AXIS2_PLACEMENT_3D('',#23331,#18456,#18457);
#16875=AXIS2_PLACEMENT_3D('',#23334,#18458,#18459);
#16876=AXIS2_PLACEMENT_3D('',#23335,#18460,#18461);
#16877=AXIS2_PLACEMENT_3D('',#23336,#18462,#18463);
#16878=AXIS2_PLACEMENT_3D('',#23337,#18464,#18465);
#16879=AXIS2_PLACEMENT_3D('',#23354,#18467,#18468);
#16880=AXIS2_PLACEMENT_3D('',#23371,#18470,#18471);
#16881=AXIS2_PLACEMENT_3D('',#23374,#18472,#18473);
#16882=AXIS2_PLACEMENT_3D('',#23376,#18474,#18475);
#16883=AXIS2_PLACEMENT_3D('',#23377,#18476,#18477);
#16884=AXIS2_PLACEMENT_3D('',#23378,#18478,#18479);
#16885=AXIS2_PLACEMENT_3D('',#23381,#18482,#18483);
#16886=AXIS2_PLACEMENT_3D('',#23385,#18486,#18487);
#16887=AXIS2_PLACEMENT_3D('',#23398,#18489,#18490);
#16888=AXIS2_PLACEMENT_3D('',#23415,#18493,#18494);
#16889=AXIS2_PLACEMENT_3D('',#23416,#18495,#18496);
#16890=AXIS2_PLACEMENT_3D('',#23417,#18497,#18498);
#16891=AXIS2_PLACEMENT_3D('',#23419,#18499,#18500);
#16892=AXIS2_PLACEMENT_3D('',#23421,#18501,#18502);
#16893=AXIS2_PLACEMENT_3D('',#23423,#18503,#18504);
#16894=AXIS2_PLACEMENT_3D('',#23424,#18505,#18506);
#16895=AXIS2_PLACEMENT_3D('',#23425,#18507,#18508);
#16896=AXIS2_PLACEMENT_3D('',#23429,#18510,#18511);
#16897=AXIS2_PLACEMENT_3D('',#23430,#18512,#18513);
#16898=AXIS2_PLACEMENT_3D('',#23431,#18514,#18515);
#16899=AXIS2_PLACEMENT_3D('',#23433,#18516,#18517);
#16900=AXIS2_PLACEMENT_3D('',#23434,#18518,#18519);
#16901=AXIS2_PLACEMENT_3D('',#23436,#18520,#18521);
#16902=AXIS2_PLACEMENT_3D('',#23438,#18522,#18523);
#16903=AXIS2_PLACEMENT_3D('',#23439,#18524,#18525);
#16904=AXIS2_PLACEMENT_3D('',#23440,#18526,#18527);
#16905=AXIS2_PLACEMENT_3D('',#23443,#18529,#18530);
#16906=AXIS2_PLACEMENT_3D('',#23444,#18531,#18532);
#16907=AXIS2_PLACEMENT_3D('',#23447,#18534,#18535);
#16908=AXIS2_PLACEMENT_3D('',#23449,#18537,#18538);
#16909=AXIS2_PLACEMENT_3D('',#23450,#18539,#18540);
#16910=AXIS2_PLACEMENT_3D('',#23451,#18541,#18542);
#16911=AXIS2_PLACEMENT_3D('',#23452,#18543,#18544);
#16912=AXIS2_PLACEMENT_3D('',#23455,#18545,#18546);
#16913=AXIS2_PLACEMENT_3D('',#23459,#18548,#18549);
#16914=AXIS2_PLACEMENT_3D('',#23461,#18551,#18552);
#16915=AXIS2_PLACEMENT_3D('',#23462,#18553,#18554);
#16916=AXIS2_PLACEMENT_3D('',#23463,#18555,#18556);
#16917=AXIS2_PLACEMENT_3D('',#23464,#18557,#18558);
#16918=AXIS2_PLACEMENT_3D('',#23466,#18559,#18560);
#16919=AXIS2_PLACEMENT_3D('',#23469,#18562,#18563);
#16920=AXIS2_PLACEMENT_3D('',#23470,#18564,#18565);
#16921=AXIS2_PLACEMENT_3D('',#23471,#18566,#18567);
#16922=AXIS2_PLACEMENT_3D('',#23472,#18568,#18569);
#16923=AXIS2_PLACEMENT_3D('',#23473,#18570,#18571);
#16924=AXIS2_PLACEMENT_3D('',#23488,#18572,#18573);
#16925=AXIS2_PLACEMENT_3D('',#23489,#18574,#18575);
#16926=AXIS2_PLACEMENT_3D('',#23490,#18576,#18577);
#16927=AXIS2_PLACEMENT_3D('',#23491,#18578,#18579);
#16928=AXIS2_PLACEMENT_3D('',#23493,#18580,#18581);
#16929=AXIS2_PLACEMENT_3D('',#23494,#18582,#18583);
#16930=AXIS2_PLACEMENT_3D('',#23495,#18584,#18585);
#16931=AXIS2_PLACEMENT_3D('',#23496,#18586,#18587);
#16932=AXIS2_PLACEMENT_3D('',#23512,#18589,#18590);
#16933=AXIS2_PLACEMENT_3D('',#23513,#18591,#18592);
#16934=AXIS2_PLACEMENT_3D('',#23516,#18594,#18595);
#16935=AXIS2_PLACEMENT_3D('',#23517,#18596,#18597);
#16936=AXIS2_PLACEMENT_3D('',#23519,#18599,#18600);
#16937=AXIS2_PLACEMENT_3D('',#23521,#18602,#18603);
#16938=AXIS2_PLACEMENT_3D('',#23643,#18615,#18616);
#16939=AXIS2_PLACEMENT_3D('',#23644,#18617,#18618);
#16940=AXIS2_PLACEMENT_3D('',#23650,#18622,#18623);
#16941=AXIS2_PLACEMENT_3D('',#23654,#18626,#18627);
#16942=AXIS2_PLACEMENT_3D('',#23658,#18630,#18631);
#16943=AXIS2_PLACEMENT_3D('',#23662,#18634,#18635);
#16944=AXIS2_PLACEMENT_3D('',#23666,#18638,#18639);
#16945=AXIS2_PLACEMENT_3D('',#23670,#18642,#18643);
#16946=AXIS2_PLACEMENT_3D('',#23674,#18646,#18647);
#16947=AXIS2_PLACEMENT_3D('',#23676,#18649,#18650);
#16948=AXIS2_PLACEMENT_3D('',#23853,#18667,#18668);
#16949=AXIS2_PLACEMENT_3D('',#23854,#18669,#18670);
#16950=AXIS2_PLACEMENT_3D('',#23860,#18674,#18675);
#16951=AXIS2_PLACEMENT_3D('',#23864,#18678,#18679);
#16952=AXIS2_PLACEMENT_3D('',#23868,#18682,#18683);
#16953=AXIS2_PLACEMENT_3D('',#23872,#18686,#18687);
#16954=AXIS2_PLACEMENT_3D('',#23876,#18690,#18691);
#16955=AXIS2_PLACEMENT_3D('',#23880,#18694,#18695);
#16956=AXIS2_PLACEMENT_3D('',#23884,#18698,#18699);
#16957=AXIS2_PLACEMENT_3D('',#23888,#18702,#18703);
#16958=AXIS2_PLACEMENT_3D('',#23892,#18706,#18707);
#16959=AXIS2_PLACEMENT_3D('',#23894,#18709,#18710);
#16960=AXIS2_PLACEMENT_3D('',#23895,#18711,#18712);
#16961=AXIS2_PLACEMENT_3D('',#23898,#18714,#18715);
#16962=AXIS2_PLACEMENT_3D('',#23899,#18716,#18717);
#16963=AXIS2_PLACEMENT_3D('',#23900,#18718,#18719);
#16964=AXIS2_PLACEMENT_3D('',#23902,#18720,#18721);
#16965=AXIS2_PLACEMENT_3D('',#23904,#18723,#18724);
#16966=AXIS2_PLACEMENT_3D('',#23906,#18726,#18727);
#16967=AXIS2_PLACEMENT_3D('',#23907,#18728,#18729);
#16968=AXIS2_PLACEMENT_3D('',#23908,#18730,#18731);
#16969=AXIS2_PLACEMENT_3D('',#23909,#18732,#18733);
#16970=AXIS2_PLACEMENT_3D('',#23910,#18734,#18735);
#16971=AXIS2_PLACEMENT_3D('',#23932,#18737,#18738);
#16972=AXIS2_PLACEMENT_3D('',#23943,#18739,#18740);
#16973=AXIS2_PLACEMENT_3D('',#24027,#18742,#18743);
#16974=AXIS2_PLACEMENT_3D('',#24117,#18745,#18746);
#16975=AXIS2_PLACEMENT_3D('',#24207,#18748,#18749);
#16976=AXIS2_PLACEMENT_3D('',#24291,#18751,#18752);
#16977=AXIS2_PLACEMENT_3D('',#24381,#18754,#18755);
#16978=AXIS2_PLACEMENT_3D('',#24465,#18757,#18758);
#16979=AXIS2_PLACEMENT_3D('',#24555,#18760,#18761);
#16980=AXIS2_PLACEMENT_3D('',#24645,#18763,#18764);
#16981=AXIS2_PLACEMENT_3D('',#24729,#18766,#18767);
#16982=AXIS2_PLACEMENT_3D('',#24819,#18769,#18770);
#16983=AXIS2_PLACEMENT_3D('',#24909,#18772,#18773);
#16984=AXIS2_PLACEMENT_3D('',#24993,#18775,#18776);
#16985=AXIS2_PLACEMENT_3D('',#25083,#18778,#18779);
#16986=AXIS2_PLACEMENT_3D('',#25167,#18781,#18782);
#16987=AXIS2_PLACEMENT_3D('',#25257,#18784,#18785);
#16988=AXIS2_PLACEMENT_3D('',#25278,#18787,#18788);
#16989=AXIS2_PLACEMENT_3D('',#25291,#18789,#18790);
#16990=AXIS2_PLACEMENT_3D('',#25328,#18792,#18793);
#16991=AXIS2_PLACEMENT_3D('',#25365,#18795,#18796);
#16992=AXIS2_PLACEMENT_3D('',#25402,#18798,#18799);
#16993=AXIS2_PLACEMENT_3D('',#25439,#18801,#18802);
#16994=AXIS2_PLACEMENT_3D('',#25477,#18804,#18805);
#16995=AXIS2_PLACEMENT_3D('',#25514,#18807,#18808);
#16996=AXIS2_PLACEMENT_3D('',#25551,#18810,#18811);
#16997=AXIS2_PLACEMENT_3D('',#25589,#18813,#18814);
#16998=AXIS2_PLACEMENT_3D('',#25626,#18816,#18817);
#16999=AXIS2_PLACEMENT_3D('',#25663,#18819,#18820);
#17000=AXIS2_PLACEMENT_3D('',#25700,#18822,#18823);
#17001=AXIS2_PLACEMENT_3D('',#25737,#18825,#18826);
#17002=AXIS2_PLACEMENT_3D('',#25775,#18828,#18829);
#17003=AXIS2_PLACEMENT_3D('',#25812,#18831,#18832);
#17004=AXIS2_PLACEMENT_3D('',#25834,#18834,#18835);
#17005=AXIS2_PLACEMENT_3D('',#25845,#18836,#18837);
#17006=AXIS2_PLACEMENT_3D('',#25935,#18839,#18840);
#17007=AXIS2_PLACEMENT_3D('',#26019,#18842,#18843);
#17008=AXIS2_PLACEMENT_3D('',#26109,#18845,#18846);
#17009=AXIS2_PLACEMENT_3D('',#26199,#18848,#18849);
#17010=AXIS2_PLACEMENT_3D('',#26289,#18851,#18852);
#17011=AXIS2_PLACEMENT_3D('',#26373,#18854,#18855);
#17012=AXIS2_PLACEMENT_3D('',#26463,#18857,#18858);
#17013=AXIS2_PLACEMENT_3D('',#26553,#18860,#18861);
#17014=AXIS2_PLACEMENT_3D('',#26640,#18863,#18864);
#17015=AXIS2_PLACEMENT_3D('',#26645,#18866,#18867);
#17016=AXIS2_PLACEMENT_3D('',#26723,#18868,#18869);
#17017=AXIS2_PLACEMENT_3D('',#26739,#18871,#18872);
#17018=AXIS2_PLACEMENT_3D('',#26748,#18873,#18874);
#17019=AXIS2_PLACEMENT_3D('',#26786,#18876,#18877);
#17020=AXIS2_PLACEMENT_3D('',#26823,#18879,#18880);
#17021=AXIS2_PLACEMENT_3D('',#26861,#18882,#18883);
#17022=AXIS2_PLACEMENT_3D('',#26898,#18885,#18886);
#17023=AXIS2_PLACEMENT_3D('',#26935,#18888,#18889);
#17024=AXIS2_PLACEMENT_3D('',#26973,#18891,#18892);
#17025=AXIS2_PLACEMENT_3D('',#27011,#18894,#18895);
#17026=AXIS2_PLACEMENT_3D('',#27048,#18897,#18898);
#17027=AXIS2_PLACEMENT_3D('',#27085,#18900,#18901);
#17028=AXIS2_PLACEMENT_3D('',#27087,#18902,#18903);
#17029=AXIS2_PLACEMENT_3D('',#27091,#18905,#18906);
#17030=AXIS2_PLACEMENT_3D('',#27092,#18907,#18908);
#17031=AXIS2_PLACEMENT_3D('',#27093,#18909,#18910);
#17032=AXIS2_PLACEMENT_3D('',#27096,#18911,#18912);
#17033=AXIS2_PLACEMENT_3D('',#27097,#18913,#18914);
#17034=AXIS2_PLACEMENT_3D('',#27099,#18916,#18917);
#17035=AXIS2_PLACEMENT_3D('',#27101,#18918,#18919);
#17036=AXIS2_PLACEMENT_3D('',#27102,#18920,#18921);
#17037=AXIS2_PLACEMENT_3D('',#27105,#18923,#18924);
#17038=AXIS2_PLACEMENT_3D('',#27106,#18925,#18926);
#17039=AXIS2_PLACEMENT_3D('',#27108,#18927,#18928);
#17040=AXIS2_PLACEMENT_3D('',#27109,#18929,#18930);
#17041=AXIS2_PLACEMENT_3D('',#27111,#18931,#18932);
#17042=AXIS2_PLACEMENT_3D('',#27115,#18934,#18935);
#17043=AXIS2_PLACEMENT_3D('',#27116,#18936,#18937);
#17044=AXIS2_PLACEMENT_3D('',#27117,#18938,#18939);
#17045=AXIS2_PLACEMENT_3D('',#27120,#18941,#18942);
#17046=AXIS2_PLACEMENT_3D('',#27121,#18943,#18944);
#17047=AXIS2_PLACEMENT_3D('',#27263,#18945,#18946);
#17048=AXIS2_PLACEMENT_3D('',#27403,#18947,#18948);
#17049=AXIS2_PLACEMENT_3D('',#27405,#18949,#18950);
#17050=AXIS2_PLACEMENT_3D('',#27416,#18952,#18953);
#17051=AXIS2_PLACEMENT_3D('',#27423,#18954,#18955);
#17052=AXIS2_PLACEMENT_3D('',#27425,#18956,#18957);
#17053=AXIS2_PLACEMENT_3D('',#27427,#18959,#18960);
#17054=AXIS2_PLACEMENT_3D('',#27430,#18962,#18963);
#17055=AXIS2_PLACEMENT_3D('',#27431,#18964,#18965);
#17056=AXIS2_PLACEMENT_3D('',#27433,#18966,#18967);
#17057=AXIS2_PLACEMENT_3D('',#27434,#18968,#18969);
#17058=AXIS2_PLACEMENT_3D('',#27575,#18970,#18971);
#17059=AXIS2_PLACEMENT_3D('',#28282,#18972,#18973);
#17060=AXIS2_PLACEMENT_3D('',#28843,#18974,#18975);
#17061=AXIS2_PLACEMENT_3D('',#28844,#18976,#18977);
#17062=AXIS2_PLACEMENT_3D('',#29955,#18978,#18979);
#17063=AXIS2_PLACEMENT_3D('',#29957,#18980,#18981);
#17064=AXIS2_PLACEMENT_3D('',#29958,#18982,#18983);
#17065=AXIS2_PLACEMENT_3D('',#30096,#18984,#18985);
#17066=AXIS2_PLACEMENT_3D('',#30097,#18986,#18987);
#17067=AXIS2_PLACEMENT_3D('',#31063,#18988,#18989);
#17068=AXIS2_PLACEMENT_3D('',#31086,#18992,#18993);
#17069=AXIS2_PLACEMENT_3D('',#31097,#18995,#18996);
#17070=AXIS2_PLACEMENT_3D('',#31137,#18997,#18998);
#17071=AXIS2_PLACEMENT_3D('',#31138,#18999,#19000);
#17072=AXIS2_PLACEMENT_3D('',#31140,#19001,#19002);
#17073=AXIS2_PLACEMENT_3D('',#31142,#19004,#19005);
#17074=AXIS2_PLACEMENT_3D('',#31155,#19007,#19008);
#17075=AXIS2_PLACEMENT_3D('',#31170,#19011,#19012);
#17076=AXIS2_PLACEMENT_3D('',#31185,#19015,#19016);
#17077=AXIS2_PLACEMENT_3D('',#31187,#19017,#19018);
#17078=AXIS2_PLACEMENT_3D('',#31190,#19020,#19021);
#17079=AXIS2_PLACEMENT_3D('',#31191,#19022,#19023);
#17080=AXIS2_PLACEMENT_3D('',#31193,#19024,#19025);
#17081=AXIS2_PLACEMENT_3D('',#31194,#19026,#19027);
#17082=AXIS2_PLACEMENT_3D('',#31197,#19029,#19030);
#17083=AXIS2_PLACEMENT_3D('',#31198,#19031,#19032);
#17084=AXIS2_PLACEMENT_3D('',#31201,#19034,#19035);
#17085=AXIS2_PLACEMENT_3D('',#31202,#19036,#19037);
#17086=AXIS2_PLACEMENT_3D('',#31205,#19039,#19040);
#17087=AXIS2_PLACEMENT_3D('',#31206,#19041,#19042);
#17088=AXIS2_PLACEMENT_3D('',#31209,#19044,#19045);
#17089=AXIS2_PLACEMENT_3D('',#31210,#19046,#19047);
#17090=AXIS2_PLACEMENT_3D('',#31266,#19049,#19050);
#17091=AXIS2_PLACEMENT_3D('',#31298,#19051,#19052);
#17092=AXIS2_PLACEMENT_3D('',#31299,#19053,#19054);
#17093=AXIS2_PLACEMENT_3D('',#31300,#19055,#19056);
#17094=AXIS2_PLACEMENT_3D('',#31302,#19057,#19058);
#17095=AXIS2_PLACEMENT_3D('',#31305,#19060,#19061);
#17096=AXIS2_PLACEMENT_3D('',#31306,#19062,#19063);
#17097=AXIS2_PLACEMENT_3D('',#31309,#19065,#19066);
#17098=AXIS2_PLACEMENT_3D('',#31312,#19069,#19070);
#17099=AXIS2_PLACEMENT_3D('',#31313,#19071,#19072);
#17100=AXIS2_PLACEMENT_3D('',#31314,#19073,#19074);
#17101=AXIS2_PLACEMENT_3D('',#31317,#19076,#19077);
#17102=AXIS2_PLACEMENT_3D('',#31318,#19078,#19079);
#17103=AXIS2_PLACEMENT_3D('',#31320,#19080,#19081);
#17104=AXIS2_PLACEMENT_3D('',#31321,#19082,#19083);
#17105=AXIS2_PLACEMENT_3D('',#31323,#19085,#19086);
#17106=AXIS2_PLACEMENT_3D('',#31324,#19087,#19088);
#17107=AXIS2_PLACEMENT_3D('',#31325,#19089,#19090);
#17108=AXIS2_PLACEMENT_3D('',#31327,#19091,#19092);
#17109=AXIS2_PLACEMENT_3D('',#31328,#19093,#19094);
#17110=AXIS2_PLACEMENT_3D('',#31330,#19096,#19097);
#17111=AXIS2_PLACEMENT_3D('',#31332,#19099,#19100);
#17112=AXIS2_PLACEMENT_3D('',#31333,#19101,#19102);
#17113=AXIS2_PLACEMENT_3D('',#31335,#19103,#19104);
#17114=AXIS2_PLACEMENT_3D('',#31338,#19106,#19107);
#17115=AXIS2_PLACEMENT_3D('',#31339,#19108,#19109);
#17116=AXIS2_PLACEMENT_3D('',#31340,#19110,#19111);
#17117=AXIS2_PLACEMENT_3D('',#31342,#19112,#19113);
#17118=AXIS2_PLACEMENT_3D('',#31343,#19114,#19115);
#17119=AXIS2_PLACEMENT_3D('',#31345,#19116,#19117);
#17120=AXIS2_PLACEMENT_3D('',#31347,#19119,#19120);
#17121=AXIS2_PLACEMENT_3D('',#31349,#19121,#19122);
#17122=AXIS2_PLACEMENT_3D('',#31351,#19124,#19125);
#17123=AXIS2_PLACEMENT_3D('',#31353,#19126,#19127);
#17124=AXIS2_PLACEMENT_3D('',#31354,#19128,#19129);
#17125=AXIS2_PLACEMENT_3D('',#31356,#19130,#19131);
#17126=AXIS2_PLACEMENT_3D('',#31358,#19133,#19134);
#17127=AXIS2_PLACEMENT_3D('',#31360,#19135,#19136);
#17128=AXIS2_PLACEMENT_3D('',#31362,#19138,#19139);
#17129=AXIS2_PLACEMENT_3D('',#31364,#19140,#19141);
#17130=AXIS2_PLACEMENT_3D('',#31365,#19142,#19143);
#17131=AXIS2_PLACEMENT_3D('',#31367,#19144,#19145);
#17132=AXIS2_PLACEMENT_3D('',#31369,#19147,#19148);
#17133=AXIS2_PLACEMENT_3D('',#31371,#19149,#19150);
#17134=AXIS2_PLACEMENT_3D('',#31372,#19151,#19152);
#17135=AXIS2_PLACEMENT_3D('',#31374,#19153,#19154);
#17136=AXIS2_PLACEMENT_3D('',#31376,#19156,#19157);
#17137=AXIS2_PLACEMENT_3D('',#31378,#19158,#19159);
#17138=AXIS2_PLACEMENT_3D('',#31379,#19160,#19161);
#17139=AXIS2_PLACEMENT_3D('',#31381,#19162,#19163);
#17140=AXIS2_PLACEMENT_3D('',#31383,#19165,#19166);
#17141=AXIS2_PLACEMENT_3D('',#31385,#19167,#19168);
#17142=AXIS2_PLACEMENT_3D('',#31386,#19169,#19170);
#17143=AXIS2_PLACEMENT_3D('',#31388,#19171,#19172);
#17144=AXIS2_PLACEMENT_3D('',#31390,#19174,#19175);
#17145=AXIS2_PLACEMENT_3D('',#31392,#19176,#19177);
#17146=AXIS2_PLACEMENT_3D('',#31394,#19179,#19180);
#17147=AXIS2_PLACEMENT_3D('',#31395,#19181,#19182);
#17148=AXIS2_PLACEMENT_3D('',#32147,#19183,#19184);
#17149=AXIS2_PLACEMENT_3D('',#32224,#19185,#19186);
#17150=AXIS2_PLACEMENT_3D('',#32225,#19187,#19188);
#17151=AXIS2_PLACEMENT_3D('',#32226,#19189,#19190);
#17152=AXIS2_PLACEMENT_3D('',#32227,#19191,#19192);
#17153=AXIS2_PLACEMENT_3D('',#32228,#19193,#19194);
#17154=AXIS2_PLACEMENT_3D('',#32230,#19195,#19196);
#17155=AXIS2_PLACEMENT_3D('',#32231,#19197,#19198);
#17156=AXIS2_PLACEMENT_3D('',#32232,#19199,#19200);
#17157=AXIS2_PLACEMENT_3D('',#32233,#19201,#19202);
#17158=AXIS2_PLACEMENT_3D('',#32235,#19203,#19204);
#17159=AXIS2_PLACEMENT_3D('',#32238,#19206,#19207);
#17160=AXIS2_PLACEMENT_3D('',#32239,#19208,#19209);
#17161=AXIS2_PLACEMENT_3D('',#32241,#19210,#19211);
#17162=AXIS2_PLACEMENT_3D('',#32242,#19212,#19213);
#17163=AXIS2_PLACEMENT_3D('',#32244,#19214,#19215);
#17164=AXIS2_PLACEMENT_3D('',#32246,#19217,#19218);
#17165=AXIS2_PLACEMENT_3D('',#32247,#19219,#19220);
#17166=AXIS2_PLACEMENT_3D('',#32248,#19221,#19222);
#17167=AXIS2_PLACEMENT_3D('',#32250,#19223,#19224);
#17168=AXIS2_PLACEMENT_3D('',#32251,#19225,#19226);
#17169=AXIS2_PLACEMENT_3D('',#32253,#19227,#19228);
#17170=AXIS2_PLACEMENT_3D('',#32255,#19230,#19231);
#17171=AXIS2_PLACEMENT_3D('',#32257,#19232,#19233);
#17172=AXIS2_PLACEMENT_3D('',#32259,#19235,#19236);
#17173=AXIS2_PLACEMENT_3D('',#32261,#19237,#19238);
#17174=AXIS2_PLACEMENT_3D('',#32263,#19240,#19241);
#17175=AXIS2_PLACEMENT_3D('',#32264,#19242,#19243);
#17176=AXIS2_PLACEMENT_3D('',#32265,#19244,#19245);
#17177=AXIS2_PLACEMENT_3D('',#32274,#19250,#19251);
#17178=AXIS2_PLACEMENT_3D('',#32284,#19257,#19258);
#17179=AXIS2_PLACEMENT_3D('',#32288,#19261,#19262);
#17180=AXIS2_PLACEMENT_3D('',#32297,#19267,#19268);
#17181=AXIS2_PLACEMENT_3D('',#32303,#19272,#19273);
#17182=AXIS2_PLACEMENT_3D('',#32310,#19278,#19279);
#17183=AXIS2_PLACEMENT_3D('',#32323,#19286,#19287);
#17184=AXIS2_PLACEMENT_3D('',#32329,#19291,#19292);
#17185=AXIS2_PLACEMENT_3D('',#32337,#19297,#19298);
#17186=AXIS2_PLACEMENT_3D('',#32343,#19302,#19303);
#17187=AXIS2_PLACEMENT_3D('',#32354,#19309,#19310);
#17188=AXIS2_PLACEMENT_3D('',#32360,#19314,#19315);
#17189=AXIS2_PLACEMENT_3D('',#32365,#19319,#19320);
#17190=AXIS2_PLACEMENT_3D('',#32375,#19326,#19327);
#17191=AXIS2_PLACEMENT_3D('',#32383,#19332,#19333);
#17192=AXIS2_PLACEMENT_3D('',#32387,#19336,#19337);
#17193=AXIS2_PLACEMENT_3D('',#32396,#19342,#19343);
#17194=AXIS2_PLACEMENT_3D('',#32404,#19349,#19350);
#17195=AXIS2_PLACEMENT_3D('',#32408,#19353,#19354);
#17196=AXIS2_PLACEMENT_3D('',#32412,#19357,#19358);
#17197=AXIS2_PLACEMENT_3D('',#32414,#19360,#19361);
#17198=AXIS2_PLACEMENT_3D('',#32418,#19364,#19365);
#17199=AXIS2_PLACEMENT_3D('',#32420,#19367,#19368);
#17200=AXIS2_PLACEMENT_3D('',#32431,#19374,#19375);
#17201=AXIS2_PLACEMENT_3D('',#32434,#19378,#19379);
#17202=AXIS2_PLACEMENT_3D('',#32680,#19413,#19414);
#17203=AXIS2_PLACEMENT_3D('',#32688,#19419,#19420);
#17204=AXIS2_PLACEMENT_3D('',#32691,#19423,#19424);
#17205=AXIS2_PLACEMENT_3D('',#32693,#19426,#19427);
#17206=AXIS2_PLACEMENT_3D('',#32697,#19430,#19431);
#17207=AXIS2_PLACEMENT_3D('',#32700,#19434,#19435);
#17208=AXIS2_PLACEMENT_3D('',#32702,#19437,#19438);
#17209=AXIS2_PLACEMENT_3D('',#32727,#19442,#19443);
#17210=AXIS2_PLACEMENT_3D('',#32731,#19446,#19447);
#17211=AXIS2_PLACEMENT_3D('',#32735,#19450,#19451);
#17212=AXIS2_PLACEMENT_3D('',#32739,#19454,#19455);
#17213=AXIS2_PLACEMENT_3D('',#32743,#19458,#19459);
#17214=AXIS2_PLACEMENT_3D('',#32769,#19464,#19465);
#17215=AXIS2_PLACEMENT_3D('',#32773,#19468,#19469);
#17216=AXIS2_PLACEMENT_3D('',#32777,#19472,#19473);
#17217=AXIS2_PLACEMENT_3D('',#32803,#19478,#19479);
#17218=AXIS2_PLACEMENT_3D('',#32807,#19482,#19483);
#17219=AXIS2_PLACEMENT_3D('',#32811,#19486,#19487);
#17220=AXIS2_PLACEMENT_3D('',#32815,#19490,#19491);
#17221=AXIS2_PLACEMENT_3D('',#32819,#19494,#19495);
#17222=AXIS2_PLACEMENT_3D('',#32821,#19497,#19498);
#17223=AXIS2_PLACEMENT_3D('',#32822,#19499,#19500);
#17224=AXIS2_PLACEMENT_3D('',#32828,#19504,#19505);
#17225=AXIS2_PLACEMENT_3D('',#32832,#19508,#19509);
#17226=AXIS2_PLACEMENT_3D('',#32836,#19512,#19513);
#17227=AXIS2_PLACEMENT_3D('',#32840,#19516,#19517);
#17228=AXIS2_PLACEMENT_3D('',#32844,#19520,#19521);
#17229=AXIS2_PLACEMENT_3D('',#32848,#19524,#19525);
#17230=AXIS2_PLACEMENT_3D('',#32852,#19528,#19529);
#17231=AXIS2_PLACEMENT_3D('',#32854,#19531,#19532);
#17232=AXIS2_PLACEMENT_3D('',#32987,#19545,#19546);
#17233=AXIS2_PLACEMENT_3D('',#33012,#19550,#19551);
#17234=AXIS2_PLACEMENT_3D('',#33038,#19556,#19557);
#17235=AXIS2_PLACEMENT_3D('',#33042,#19560,#19561);
#17236=AXIS2_PLACEMENT_3D('',#33046,#19564,#19565);
#17237=AXIS2_PLACEMENT_3D('',#33050,#19568,#19569);
#17238=AXIS2_PLACEMENT_3D('',#33052,#19571,#19572);
#17239=AXIS2_PLACEMENT_3D('',#33187,#19586,#19587);
#17240=AXIS2_PLACEMENT_3D('',#33312,#19601,#19602);
#17241=AXIS2_PLACEMENT_3D('',#33316,#19605,#19606);
#17242=AXIS2_PLACEMENT_3D('',#33320,#19609,#19610);
#17243=AXIS2_PLACEMENT_3D('',#33324,#19613,#19614);
#17244=AXIS2_PLACEMENT_3D('',#33328,#19617,#19618);
#17245=AXIS2_PLACEMENT_3D('',#33330,#19620,#19621);
#17246=AXIS2_PLACEMENT_3D('',#33331,#19622,#19623);
#17247=AXIS2_PLACEMENT_3D('',#33334,#19626,#19627);
#17248=AXIS2_PLACEMENT_3D('',#33336,#19629,#19630);
#17249=AXIS2_PLACEMENT_3D('',#33337,#19631,#19632);
#17250=AXIS2_PLACEMENT_3D('',#33339,#19634,#19635);
#17251=AXIS2_PLACEMENT_3D('',#33340,#19636,#19637);
#17252=AXIS2_PLACEMENT_3D('',#33342,#19639,#19640);
#17253=AXIS2_PLACEMENT_3D('',#33343,#19641,#19642);
#17254=AXIS2_PLACEMENT_3D('',#33344,#19643,#19644);
#17255=AXIS2_PLACEMENT_3D('',#33346,#19645,#19646);
#17256=AXIS2_PLACEMENT_3D('',#33347,#19647,#19648);
#17257=AXIS2_PLACEMENT_3D('',#33349,#19649,#19650);
#17258=AXIS2_PLACEMENT_3D('',#33351,#19652,#19653);
#17259=AXIS2_PLACEMENT_3D('',#33353,#19654,#19655);
#17260=AXIS2_PLACEMENT_3D('',#33355,#19657,#19658);
#17261=AXIS2_PLACEMENT_3D('',#33357,#19659,#19660);
#17262=AXIS2_PLACEMENT_3D('',#33358,#19661,#19662);
#17263=AXIS2_PLACEMENT_3D('',#33360,#19663,#19664);
#17264=AXIS2_PLACEMENT_3D('',#33362,#19666,#19667);
#17265=AXIS2_PLACEMENT_3D('',#33364,#19668,#19669);
#17266=AXIS2_PLACEMENT_3D('',#33365,#19670,#19671);
#17267=AXIS2_PLACEMENT_3D('',#33367,#19672,#19673);
#17268=AXIS2_PLACEMENT_3D('',#33369,#19675,#19676);
#17269=AXIS2_PLACEMENT_3D('',#33371,#19677,#19678);
#17270=AXIS2_PLACEMENT_3D('',#33372,#19679,#19680);
#17271=AXIS2_PLACEMENT_3D('',#33374,#19681,#19682);
#17272=AXIS2_PLACEMENT_3D('',#33376,#19684,#19685);
#17273=AXIS2_PLACEMENT_3D('',#33378,#19686,#19687);
#17274=AXIS2_PLACEMENT_3D('',#33379,#19688,#19689);
#17275=AXIS2_PLACEMENT_3D('',#33381,#19690,#19691);
#17276=AXIS2_PLACEMENT_3D('',#33383,#19693,#19694);
#17277=AXIS2_PLACEMENT_3D('',#33385,#19695,#19696);
#17278=AXIS2_PLACEMENT_3D('',#33387,#19698,#19699);
#17279=AXIS2_PLACEMENT_3D('',#33388,#19700,#19701);
#17280=AXIS2_PLACEMENT_3D('',#33389,#19702,#19703);
#17281=AXIS2_PLACEMENT_3D('',#33411,#19705,#19706);
#17282=AXIS2_PLACEMENT_3D('',#33422,#19707,#19708);
#17283=AXIS2_PLACEMENT_3D('',#33506,#19710,#19711);
#17284=AXIS2_PLACEMENT_3D('',#33596,#19713,#19714);
#17285=AXIS2_PLACEMENT_3D('',#33686,#19716,#19717);
#17286=AXIS2_PLACEMENT_3D('',#33770,#19719,#19720);
#17287=AXIS2_PLACEMENT_3D('',#33860,#19722,#19723);
#17288=AXIS2_PLACEMENT_3D('',#33950,#19725,#19726);
#17289=AXIS2_PLACEMENT_3D('',#34034,#19728,#19729);
#17290=AXIS2_PLACEMENT_3D('',#34124,#19731,#19732);
#17291=AXIS2_PLACEMENT_3D('',#34214,#19734,#19735);
#17292=AXIS2_PLACEMENT_3D('',#34298,#19737,#19738);
#17293=AXIS2_PLACEMENT_3D('',#34388,#19740,#19741);
#17294=AXIS2_PLACEMENT_3D('',#34409,#19743,#19744);
#17295=AXIS2_PLACEMENT_3D('',#34422,#19745,#19746);
#17296=AXIS2_PLACEMENT_3D('',#34459,#19748,#19749);
#17297=AXIS2_PLACEMENT_3D('',#34496,#19751,#19752);
#17298=AXIS2_PLACEMENT_3D('',#34534,#19754,#19755);
#17299=AXIS2_PLACEMENT_3D('',#34571,#19757,#19758);
#17300=AXIS2_PLACEMENT_3D('',#34608,#19760,#19761);
#17301=AXIS2_PLACEMENT_3D('',#34646,#19763,#19764);
#17302=AXIS2_PLACEMENT_3D('',#34683,#19766,#19767);
#17303=AXIS2_PLACEMENT_3D('',#34720,#19769,#19770);
#17304=AXIS2_PLACEMENT_3D('',#34758,#19772,#19773);
#17305=AXIS2_PLACEMENT_3D('',#34795,#19775,#19776);
#17306=AXIS2_PLACEMENT_3D('',#34797,#19777,#19778);
#17307=AXIS2_PLACEMENT_3D('',#34801,#19780,#19781);
#17308=AXIS2_PLACEMENT_3D('',#34802,#19782,#19783);
#17309=AXIS2_PLACEMENT_3D('',#34803,#19784,#19785);
#17310=AXIS2_PLACEMENT_3D('',#34807,#19787,#19788);
#17311=AXIS2_PLACEMENT_3D('',#34808,#19789,#19790);
#17312=AXIS2_PLACEMENT_3D('',#34809,#19791,#19792);
#17313=AXIS2_PLACEMENT_3D('',#34942,#19793,#19794);
#17314=AXIS2_PLACEMENT_3D('',#35073,#19795,#19796);
#17315=AXIS2_PLACEMENT_3D('',#35077,#19798,#19799);
#17316=AXIS2_PLACEMENT_3D('',#35078,#19800,#19801);
#17317=AXIS2_PLACEMENT_3D('',#35079,#19802,#19803);
#17318=AXIS2_PLACEMENT_3D('',#35082,#19805,#19806);
#17319=AXIS2_PLACEMENT_3D('',#35083,#19807,#19808);
#17320=AXIS2_PLACEMENT_3D('',#35216,#19809,#19810);
#17321=AXIS2_PLACEMENT_3D('',#35218,#19811,#19812);
#17322=AXIS2_PLACEMENT_3D('',#35991,#19813,#19814);
#17323=AXIS2_PLACEMENT_3D('',#36626,#19815,#19816);
#17324=AXIS2_PLACEMENT_3D('',#36627,#19817,#19818);
#17325=AXIS2_PLACEMENT_3D('',#36628,#19819,#19820);
#17326=AXIS2_PLACEMENT_3D('',#36630,#19821,#19822);
#17327=AXIS2_PLACEMENT_3D('',#36633,#19824,#19825);
#17328=AXIS2_PLACEMENT_3D('',#36634,#19826,#19827);
#17329=AXIS2_PLACEMENT_3D('',#36636,#19828,#19829);
#17330=AXIS2_PLACEMENT_3D('',#36637,#19830,#19831);
#17331=AXIS2_PLACEMENT_3D('',#36639,#19833,#19834);
#17332=AXIS2_PLACEMENT_3D('',#36641,#19835,#19836);
#17333=AXIS2_PLACEMENT_3D('',#36643,#19838,#19839);
#17334=AXIS2_PLACEMENT_3D('',#36645,#19840,#19841);
#17335=AXIS2_PLACEMENT_3D('',#36646,#19842,#19843);
#17336=AXIS2_PLACEMENT_3D('',#36649,#19845,#19846);
#17337=AXIS2_PLACEMENT_3D('',#36650,#19847,#19848);
#17338=AXIS2_PLACEMENT_3D('',#36652,#19849,#19850);
#17339=AXIS2_PLACEMENT_3D('',#36653,#19851,#19852);
#17340=AXIS2_PLACEMENT_3D('',#36656,#19854,#19855);
#17341=AXIS2_PLACEMENT_3D('',#36657,#19856,#19857);
#17342=AXIS2_PLACEMENT_3D('',#36658,#19858,#19859);
#17343=AXIS2_PLACEMENT_3D('',#36659,#19860,#19861);
#17344=AXIS2_PLACEMENT_3D('',#36681,#19863,#19864);
#17345=AXIS2_PLACEMENT_3D('',#36692,#19865,#19866);
#17346=AXIS2_PLACEMENT_3D('',#36776,#19868,#19869);
#17347=AXIS2_PLACEMENT_3D('',#36866,#19871,#19872);
#17348=AXIS2_PLACEMENT_3D('',#36956,#19874,#19875);
#17349=AXIS2_PLACEMENT_3D('',#37040,#19877,#19878);
#17350=AXIS2_PLACEMENT_3D('',#37130,#19880,#19881);
#17351=AXIS2_PLACEMENT_3D('',#37217,#19883,#19884);
#17352=AXIS2_PLACEMENT_3D('',#37304,#19886,#19887);
#17353=AXIS2_PLACEMENT_3D('',#37394,#19889,#19890);
#17354=AXIS2_PLACEMENT_3D('',#37478,#19892,#19893);
#17355=AXIS2_PLACEMENT_3D('',#37568,#19895,#19896);
#17356=AXIS2_PLACEMENT_3D('',#37658,#19898,#19899);
#17357=AXIS2_PLACEMENT_3D('',#37742,#19901,#19902);
#17358=AXIS2_PLACEMENT_3D('',#37751,#19904,#19905);
#17359=AXIS2_PLACEMENT_3D('',#37752,#19906,#19907);
#17360=AXIS2_PLACEMENT_3D('',#37773,#19909,#19910);
#17361=AXIS2_PLACEMENT_3D('',#37788,#19911,#19912);
#17362=AXIS2_PLACEMENT_3D('',#37825,#19914,#19915);
#17363=AXIS2_PLACEMENT_3D('',#37863,#19917,#19918);
#17364=AXIS2_PLACEMENT_3D('',#37900,#19920,#19921);
#17365=AXIS2_PLACEMENT_3D('',#37937,#19923,#19924);
#17366=AXIS2_PLACEMENT_3D('',#37975,#19926,#19927);
#17367=AXIS2_PLACEMENT_3D('',#38011,#19929,#19930);
#17368=AXIS2_PLACEMENT_3D('',#38049,#19932,#19933);
#17369=AXIS2_PLACEMENT_3D('',#38086,#19935,#19936);
#17370=AXIS2_PLACEMENT_3D('',#38123,#19938,#19939);
#17371=AXIS2_PLACEMENT_3D('',#38161,#19941,#19942);
#17372=AXIS2_PLACEMENT_3D('',#38198,#19944,#19945);
#17373=AXIS2_PLACEMENT_3D('',#38211,#19947,#19948);
#17374=AXIS2_PLACEMENT_3D('',#38214,#19950,#19951);
#17375=AXIS2_PLACEMENT_3D('',#38215,#19952,#19953);
#17376=AXIS2_PLACEMENT_3D('',#38216,#19954,#19955);
#17377=AXIS2_PLACEMENT_3D('',#38217,#19956,#19957);
#17378=AXIS2_PLACEMENT_3D('',#38230,#19959,#19960);
#17379=AXIS2_PLACEMENT_3D('',#38233,#19962,#19963);
#17380=AXIS2_PLACEMENT_3D('',#38234,#19964,#19965);
#17381=AXIS2_PLACEMENT_3D('',#38235,#19966,#19967);
#17382=AXIS2_PLACEMENT_3D('',#38239,#19969,#19970);
#17383=AXIS2_PLACEMENT_3D('',#38243,#19972,#19973);
#17384=AXIS2_PLACEMENT_3D('',#38247,#19975,#19976);
#17385=AXIS2_PLACEMENT_3D('',#38250,#19978,#19979);
#17386=AXIS2_PLACEMENT_3D('',#38254,#19981,#19982);
#17387=AXIS2_PLACEMENT_3D('',#38258,#19984,#19985);
#17388=AXIS2_PLACEMENT_3D('',#38261,#19987,#19988);
#17389=AXIS2_PLACEMENT_3D('',#38263,#19989,#19990);
#17390=AXIS2_PLACEMENT_3D('',#38266,#19992,#19993);
#17391=AXIS2_PLACEMENT_3D('',#38267,#19994,#19995);
#17392=AXIS2_PLACEMENT_3D('',#38271,#19997,#19998);
#17393=AXIS2_PLACEMENT_3D('',#38275,#20000,#20001);
#17394=AXIS2_PLACEMENT_3D('',#38279,#20003,#20004);
#17395=AXIS2_PLACEMENT_3D('',#38285,#20007,#20008);
#17396=AXIS2_PLACEMENT_3D('',#38288,#20010,#20011);
#17397=AXIS2_PLACEMENT_3D('',#38293,#20013,#20014);
#17398=AXIS2_PLACEMENT_3D('',#38296,#20016,#20017);
#17399=AXIS2_PLACEMENT_3D('',#38301,#20019,#20020);
#17400=AXIS2_PLACEMENT_3D('',#38304,#20022,#20023);
#17401=AXIS2_PLACEMENT_3D('',#38309,#20025,#20026);
#17402=AXIS2_PLACEMENT_3D('',#38312,#20028,#20029);
#17403=AXIS2_PLACEMENT_3D('',#38317,#20031,#20032);
#17404=AXIS2_PLACEMENT_3D('',#38320,#20034,#20035);
#17405=AXIS2_PLACEMENT_3D('',#38325,#20037,#20038);
#17406=AXIS2_PLACEMENT_3D('',#38328,#20040,#20041);
#17407=AXIS2_PLACEMENT_3D('',#38333,#20043,#20044);
#17408=AXIS2_PLACEMENT_3D('',#38336,#20046,#20047);
#17409=AXIS2_PLACEMENT_3D('',#38341,#20049,#20050);
#17410=AXIS2_PLACEMENT_3D('',#38344,#20052,#20053);
#17411=AXIS2_PLACEMENT_3D('',#38349,#20055,#20056);
#17412=AXIS2_PLACEMENT_3D('',#38352,#20058,#20059);
#17413=AXIS2_PLACEMENT_3D('',#38357,#20061,#20062);
#17414=AXIS2_PLACEMENT_3D('',#38360,#20064,#20065);
#17415=AXIS2_PLACEMENT_3D('',#38365,#20067,#20068);
#17416=AXIS2_PLACEMENT_3D('',#38368,#20070,#20071);
#17417=AXIS2_PLACEMENT_3D('',#38373,#20073,#20074);
#17418=AXIS2_PLACEMENT_3D('',#38376,#20076,#20077);
#17419=AXIS2_PLACEMENT_3D('',#38381,#20079,#20080);
#17420=AXIS2_PLACEMENT_3D('',#38384,#20082,#20083);
#17421=AXIS2_PLACEMENT_3D('',#38389,#20085,#20086);
#17422=AXIS2_PLACEMENT_3D('',#38392,#20088,#20089);
#17423=AXIS2_PLACEMENT_3D('',#38397,#20091,#20092);
#17424=AXIS2_PLACEMENT_3D('',#38400,#20094,#20095);
#17425=AXIS2_PLACEMENT_3D('',#38405,#20097,#20098);
#17426=AXIS2_PLACEMENT_3D('',#38408,#20100,#20101);
#17427=AXIS2_PLACEMENT_3D('',#38413,#20103,#20104);
#17428=AXIS2_PLACEMENT_3D('',#38416,#20106,#20107);
#17429=AXIS2_PLACEMENT_3D('',#38421,#20109,#20110);
#17430=AXIS2_PLACEMENT_3D('',#38424,#20112,#20113);
#17431=AXIS2_PLACEMENT_3D('',#38429,#20115,#20116);
#17432=AXIS2_PLACEMENT_3D('',#38432,#20118,#20119);
#17433=AXIS2_PLACEMENT_3D('',#38437,#20121,#20122);
#17434=AXIS2_PLACEMENT_3D('',#38440,#20124,#20125);
#17435=AXIS2_PLACEMENT_3D('',#38445,#20127,#20128);
#17436=AXIS2_PLACEMENT_3D('',#38448,#20130,#20131);
#17437=AXIS2_PLACEMENT_3D('',#38449,#20132,#20133);
#17438=AXIS2_PLACEMENT_3D('',#38450,#20134,#20135);
#17439=AXIS2_PLACEMENT_3D('',#38451,#20136,#20137);
#17440=AXIS2_PLACEMENT_3D('',#39361,#20138,#20139);
#17441=AXIS2_PLACEMENT_3D('',#39363,#20140,#20141);
#17442=AXIS2_PLACEMENT_3D('',#39364,#20142,#20143);
#17443=AXIS2_PLACEMENT_3D('',#39466,#20144,#20145);
#17444=AXIS2_PLACEMENT_3D('',#39467,#20146,#20147);
#17445=AXIS2_PLACEMENT_3D('',#40268,#20148,#20149);
#17446=AXIS2_PLACEMENT_3D('',#40270,#20151,#20152);
#17447=AXIS2_PLACEMENT_3D('',#40278,#20158,#20159);
#17448=AXIS2_PLACEMENT_3D('',#40279,#20160,#20161);
#17449=AXIS2_PLACEMENT_3D('',#40283,#20164,#20165);
#17450=AXIS2_PLACEMENT_3D('',#40289,#20169,#20170);
#17451=AXIS2_PLACEMENT_3D('',#40291,#20172,#20173);
#17452=AXIS2_PLACEMENT_3D('',#40293,#20175,#20176);
#17453=AXIS2_PLACEMENT_3D('',#40294,#20177,#20178);
#17454=AXIS2_PLACEMENT_3D('',#40300,#20182,#20183);
#17455=AXIS2_PLACEMENT_3D('',#40302,#20185,#20186);
#17456=AXIS2_PLACEMENT_3D('',#40304,#20188,#20189);
#17457=AXIS2_PLACEMENT_3D('',#40305,#20190,#20191);
#17458=AXIS2_PLACEMENT_3D('',#40311,#20195,#20196);
#17459=AXIS2_PLACEMENT_3D('',#40313,#20198,#20199);
#17460=AXIS2_PLACEMENT_3D('',#40315,#20201,#20202);
#17461=AXIS2_PLACEMENT_3D('',#40316,#20203,#20204);
#17462=AXIS2_PLACEMENT_3D('',#40322,#20208,#20209);
#17463=AXIS2_PLACEMENT_3D('',#40324,#20211,#20212);
#17464=AXIS2_PLACEMENT_3D('',#40326,#20214,#20215);
#17465=AXIS2_PLACEMENT_3D('',#40327,#20216,#20217);
#17466=AXIS2_PLACEMENT_3D('',#40333,#20221,#20222);
#17467=AXIS2_PLACEMENT_3D('',#40335,#20224,#20225);
#17468=AXIS2_PLACEMENT_3D('',#40337,#20227,#20228);
#17469=AXIS2_PLACEMENT_3D('',#40338,#20229,#20230);
#17470=AXIS2_PLACEMENT_3D('',#40340,#20232,#20233);
#17471=AXIS2_PLACEMENT_3D('',#40341,#20234,#20235);
#17472=AXIS2_PLACEMENT_3D('',#40347,#20239,#20240);
#17473=AXIS2_PLACEMENT_3D('',#40349,#20242,#20243);
#17474=AXIS2_PLACEMENT_3D('',#40351,#20245,#20246);
#17475=AXIS2_PLACEMENT_3D('',#40352,#20247,#20248);
#17476=AXIS2_PLACEMENT_3D('',#40358,#20252,#20253);
#17477=AXIS2_PLACEMENT_3D('',#40360,#20255,#20256);
#17478=AXIS2_PLACEMENT_3D('',#40362,#20258,#20259);
#17479=AXIS2_PLACEMENT_3D('',#40363,#20260,#20261);
#17480=AXIS2_PLACEMENT_3D('',#40369,#20265,#20266);
#17481=AXIS2_PLACEMENT_3D('',#40371,#20268,#20269);
#17482=AXIS2_PLACEMENT_3D('',#40373,#20271,#20272);
#17483=AXIS2_PLACEMENT_3D('',#40374,#20273,#20274);
#17484=AXIS2_PLACEMENT_3D('',#40380,#20278,#20279);
#17485=AXIS2_PLACEMENT_3D('',#40382,#20281,#20282);
#17486=AXIS2_PLACEMENT_3D('',#40384,#20284,#20285);
#17487=AXIS2_PLACEMENT_3D('',#40385,#20286,#20287);
#17488=AXIS2_PLACEMENT_3D('',#40391,#20291,#20292);
#17489=AXIS2_PLACEMENT_3D('',#40393,#20294,#20295);
#17490=AXIS2_PLACEMENT_3D('',#40395,#20297,#20298);
#17491=AXIS2_PLACEMENT_3D('',#40396,#20299,#20300);
#17492=AXIS2_PLACEMENT_3D('',#40402,#20304,#20305);
#17493=AXIS2_PLACEMENT_3D('',#40404,#20307,#20308);
#17494=AXIS2_PLACEMENT_3D('',#40406,#20310,#20311);
#17495=AXIS2_PLACEMENT_3D('',#40407,#20312,#20313);
#17496=AXIS2_PLACEMENT_3D('',#40413,#20317,#20318);
#17497=AXIS2_PLACEMENT_3D('',#40415,#20320,#20321);
#17498=AXIS2_PLACEMENT_3D('',#40417,#20323,#20324);
#17499=AXIS2_PLACEMENT_3D('',#40418,#20325,#20326);
#17500=AXIS2_PLACEMENT_3D('',#40424,#20330,#20331);
#17501=AXIS2_PLACEMENT_3D('',#40426,#20333,#20334);
#17502=AXIS2_PLACEMENT_3D('',#40428,#20336,#20337);
#17503=AXIS2_PLACEMENT_3D('',#40429,#20338,#20339);
#17504=AXIS2_PLACEMENT_3D('',#40435,#20343,#20344);
#17505=AXIS2_PLACEMENT_3D('',#40437,#20346,#20347);
#17506=AXIS2_PLACEMENT_3D('',#40439,#20349,#20350);
#17507=AXIS2_PLACEMENT_3D('',#40440,#20351,#20352);
#17508=AXIS2_PLACEMENT_3D('',#40446,#20356,#20357);
#17509=AXIS2_PLACEMENT_3D('',#40448,#20359,#20360);
#17510=AXIS2_PLACEMENT_3D('',#40450,#20362,#20363);
#17511=AXIS2_PLACEMENT_3D('',#40451,#20364,#20365);
#17512=AXIS2_PLACEMENT_3D('',#40457,#20369,#20370);
#17513=AXIS2_PLACEMENT_3D('',#40459,#20372,#20373);
#17514=AXIS2_PLACEMENT_3D('',#40461,#20375,#20376);
#17515=AXIS2_PLACEMENT_3D('',#40462,#20377,#20378);
#17516=AXIS2_PLACEMENT_3D('',#40466,#20381,#20382);
#17517=AXIS2_PLACEMENT_3D('',#40468,#20384,#20385);
#17518=AXIS2_PLACEMENT_3D('',#40469,#20386,#20387);
#17519=AXIS2_PLACEMENT_3D('',#40475,#20391,#20392);
#17520=AXIS2_PLACEMENT_3D('',#40477,#20394,#20395);
#17521=AXIS2_PLACEMENT_3D('',#40479,#20397,#20398);
#17522=AXIS2_PLACEMENT_3D('',#40480,#20399,#20400);
#17523=AXIS2_PLACEMENT_3D('',#40486,#20404,#20405);
#17524=AXIS2_PLACEMENT_3D('',#40488,#20407,#20408);
#17525=AXIS2_PLACEMENT_3D('',#40490,#20410,#20411);
#17526=AXIS2_PLACEMENT_3D('',#40491,#20412,#20413);
#17527=AXIS2_PLACEMENT_3D('',#40497,#20417,#20418);
#17528=AXIS2_PLACEMENT_3D('',#40499,#20420,#20421);
#17529=AXIS2_PLACEMENT_3D('',#40501,#20423,#20424);
#17530=AXIS2_PLACEMENT_3D('',#40502,#20425,#20426);
#17531=AXIS2_PLACEMENT_3D('',#40508,#20430,#20431);
#17532=AXIS2_PLACEMENT_3D('',#40510,#20433,#20434);
#17533=AXIS2_PLACEMENT_3D('',#40512,#20436,#20437);
#17534=AXIS2_PLACEMENT_3D('',#40513,#20438,#20439);
#17535=AXIS2_PLACEMENT_3D('',#40519,#20443,#20444);
#17536=AXIS2_PLACEMENT_3D('',#40521,#20446,#20447);
#17537=AXIS2_PLACEMENT_3D('',#40523,#20449,#20450);
#17538=AXIS2_PLACEMENT_3D('',#40524,#20451,#20452);
#17539=AXIS2_PLACEMENT_3D('',#40530,#20456,#20457);
#17540=AXIS2_PLACEMENT_3D('',#40532,#20459,#20460);
#17541=AXIS2_PLACEMENT_3D('',#40534,#20462,#20463);
#17542=AXIS2_PLACEMENT_3D('',#40535,#20464,#20465);
#17543=AXIS2_PLACEMENT_3D('',#40537,#20466,#20467);
#17544=AXIS2_PLACEMENT_3D('',#40538,#20468,#20469);
#17545=AXIS2_PLACEMENT_3D('',#40540,#20471,#20472);
#17546=AXIS2_PLACEMENT_3D('',#40541,#20473,#20474);
#17547=AXIS2_PLACEMENT_3D('',#40542,#20475,#20476);
#17548=AXIS2_PLACEMENT_3D('',#40544,#20477,#20478);
#17549=AXIS2_PLACEMENT_3D('',#40545,#20479,#20480);
#17550=AXIS2_PLACEMENT_3D('',#40547,#20482,#20483);
#17551=AXIS2_PLACEMENT_3D('',#40548,#20484,#20485);
#17552=AXIS2_PLACEMENT_3D('',#40549,#20486,#20487);
#17553=AXIS2_PLACEMENT_3D('',#40551,#20488,#20489);
#17554=AXIS2_PLACEMENT_3D('',#40555,#20491,#20492);
#17555=AXIS2_PLACEMENT_3D('',#40556,#20493,#20494);
#17556=AXIS2_PLACEMENT_3D('',#40557,#20495,#20496);
#17557=AXIS2_PLACEMENT_3D('',#40559,#20497,#20498);
#17558=AXIS2_PLACEMENT_3D('',#40561,#20500,#20501);
#17559=AXIS2_PLACEMENT_3D('',#40563,#20502,#20503);
#17560=AXIS2_PLACEMENT_3D('',#40564,#20504,#20505);
#17561=AXIS2_PLACEMENT_3D('',#40567,#20507,#20508);
#17562=AXIS2_PLACEMENT_3D('',#40568,#20509,#20510);
#17563=AXIS2_PLACEMENT_3D('',#40570,#20511,#20512);
#17564=AXIS2_PLACEMENT_3D('',#40571,#20513,#20514);
#17565=AXIS2_PLACEMENT_3D('',#40573,#20515,#20516);
#17566=AXIS2_PLACEMENT_3D('',#40575,#20518,#20519);
#17567=AXIS2_PLACEMENT_3D('',#40577,#20520,#20521);
#17568=AXIS2_PLACEMENT_3D('',#40579,#20523,#20524);
#17569=AXIS2_PLACEMENT_3D('',#40581,#20525,#20526);
#17570=AXIS2_PLACEMENT_3D('',#40583,#20528,#20529);
#17571=AXIS2_PLACEMENT_3D('',#40584,#20530,#20531);
#17572=AXIS2_PLACEMENT_3D('',#40585,#20532,#20533);
#17573=AXIS2_PLACEMENT_3D('',#40586,#20534,#20535);
#17574=AXIS2_PLACEMENT_3D('',#40588,#20536,#20537);
#17575=AXIS2_PLACEMENT_3D('',#40592,#20539,#20540);
#17576=AXIS2_PLACEMENT_3D('',#40593,#20541,#20542);
#17577=AXIS2_PLACEMENT_3D('',#40594,#20543,#20544);
#17578=AXIS2_PLACEMENT_3D('',#40598,#20546,#20547);
#17579=AXIS2_PLACEMENT_3D('',#40599,#20548,#20549);
#17580=AXIS2_PLACEMENT_3D('',#40600,#20550,#20551);
#17581=AXIS2_PLACEMENT_3D('',#40601,#20552,#20553);
#17582=AXIS2_PLACEMENT_3D('',#40605,#20555,#20556);
#17583=AXIS2_PLACEMENT_3D('',#40606,#20557,#20558);
#17584=AXIS2_PLACEMENT_3D('',#40607,#20559,#20560);
#17585=AXIS2_PLACEMENT_3D('',#40611,#20562,#20563);
#17586=AXIS2_PLACEMENT_3D('',#40612,#20564,#20565);
#17587=AXIS2_PLACEMENT_3D('',#40613,#20566,#20567);
#17588=AXIS2_PLACEMENT_3D('',#40617,#20569,#20570);
#17589=AXIS2_PLACEMENT_3D('',#40618,#20571,#20572);
#17590=AXIS2_PLACEMENT_3D('',#40619,#20573,#20574);
#17591=AXIS2_PLACEMENT_3D('',#40622,#20576,#20577);
#17592=AXIS2_PLACEMENT_3D('',#40623,#20578,#20579);
#17593=AXIS2_PLACEMENT_3D('',#40625,#20580,#20581);
#17594=AXIS2_PLACEMENT_3D('',#40628,#20583,#20584);
#17595=AXIS2_PLACEMENT_3D('',#40629,#20585,#20586);
#17596=AXIS2_PLACEMENT_3D('',#40631,#20587,#20588);
#17597=AXIS2_PLACEMENT_3D('',#40632,#20589,#20590);
#17598=AXIS2_PLACEMENT_3D('',#40634,#20592,#20593);
#17599=AXIS2_PLACEMENT_3D('',#40636,#20594,#20595);
#17600=AXIS2_PLACEMENT_3D('',#40637,#20596,#20597);
#17601=AXIS2_PLACEMENT_3D('',#40639,#20599,#20600);
#17602=AXIS2_PLACEMENT_3D('',#40640,#20601,#20602);
#17603=AXIS2_PLACEMENT_3D('',#40656,#20604,#20605);
#17604=AXIS2_PLACEMENT_3D('',#40667,#20606,#20607);
#17605=AXIS2_PLACEMENT_3D('',#40715,#20609,#20610);
#17606=AXIS2_PLACEMENT_3D('',#40763,#20612,#20613);
#17607=AXIS2_PLACEMENT_3D('',#40811,#20615,#20616);
#17608=AXIS2_PLACEMENT_3D('',#40865,#20618,#20619);
#17609=AXIS2_PLACEMENT_3D('',#40913,#20621,#20622);
#17610=AXIS2_PLACEMENT_3D('',#40961,#20624,#20625);
#17611=AXIS2_PLACEMENT_3D('',#41015,#20627,#20628);
#17612=AXIS2_PLACEMENT_3D('',#41063,#20630,#20631);
#17613=AXIS2_PLACEMENT_3D('',#41111,#20633,#20634);
#17614=AXIS2_PLACEMENT_3D('',#41159,#20636,#20637);
#17615=AXIS2_PLACEMENT_3D('',#41213,#20639,#20640);
#17616=AXIS2_PLACEMENT_3D('',#41261,#20642,#20643);
#17617=AXIS2_PLACEMENT_3D('',#41276,#20645,#20646);
#17618=AXIS2_PLACEMENT_3D('',#41286,#20647,#20648);
#17619=AXIS2_PLACEMENT_3D('',#41311,#20650,#20651);
#17620=AXIS2_PLACEMENT_3D('',#41336,#20653,#20654);
#17621=AXIS2_PLACEMENT_3D('',#41360,#20656,#20657);
#17622=AXIS2_PLACEMENT_3D('',#41384,#20659,#20660);
#17623=AXIS2_PLACEMENT_3D('',#41409,#20662,#20663);
#17624=AXIS2_PLACEMENT_3D('',#41434,#20665,#20666);
#17625=AXIS2_PLACEMENT_3D('',#41458,#20668,#20669);
#17626=AXIS2_PLACEMENT_3D('',#41483,#20671,#20672);
#17627=AXIS2_PLACEMENT_3D('',#41508,#20674,#20675);
#17628=AXIS2_PLACEMENT_3D('',#41532,#20677,#20678);
#17629=AXIS2_PLACEMENT_3D('',#42133,#20680,#20681);
#17630=AXIS2_PLACEMENT_3D('',#42135,#20682,#20683);
#17631=AXIS2_PLACEMENT_3D('',#42136,#20684,#20685);
#17632=AXIS2_PLACEMENT_3D('',#42250,#20686,#20687);
#17633=AXIS2_PLACEMENT_3D('',#42251,#20688,#20689);
#17634=AXIS2_PLACEMENT_3D('',#42725,#20690,#20691);
#17635=AXIS2_PLACEMENT_3D('',#42726,#20692,#20693);
#17636=AXIS2_PLACEMENT_3D('',#42728,#20694,#20695);
#17637=AXIS2_PLACEMENT_3D('',#42894,#20707,#20708);
#17638=AXIS2_PLACEMENT_3D('',#42895,#20709,#20710);
#17639=AXIS2_PLACEMENT_3D('',#42904,#20715,#20716);
#17640=AXIS2_PLACEMENT_3D('',#42910,#20720,#20721);
#17641=AXIS2_PLACEMENT_3D('',#42916,#20725,#20726);
#17642=AXIS2_PLACEMENT_3D('',#42922,#20730,#20731);
#17643=AXIS2_PLACEMENT_3D('',#42928,#20735,#20736);
#17644=AXIS2_PLACEMENT_3D('',#42934,#20740,#20741);
#17645=AXIS2_PLACEMENT_3D('',#42940,#20745,#20746);
#17646=AXIS2_PLACEMENT_3D('',#42946,#20750,#20751);
#17647=AXIS2_PLACEMENT_3D('',#42952,#20755,#20756);
#17648=AXIS2_PLACEMENT_3D('',#42955,#20759,#20760);
#17649=AXIS2_PLACEMENT_3D('',#43121,#20772,#20773);
#17650=AXIS2_PLACEMENT_3D('',#43122,#20774,#20775);
#17651=AXIS2_PLACEMENT_3D('',#43131,#20780,#20781);
#17652=AXIS2_PLACEMENT_3D('',#43137,#20785,#20786);
#17653=AXIS2_PLACEMENT_3D('',#43143,#20790,#20791);
#17654=AXIS2_PLACEMENT_3D('',#43149,#20795,#20796);
#17655=AXIS2_PLACEMENT_3D('',#43155,#20800,#20801);
#17656=AXIS2_PLACEMENT_3D('',#43161,#20805,#20806);
#17657=AXIS2_PLACEMENT_3D('',#43167,#20810,#20811);
#17658=AXIS2_PLACEMENT_3D('',#43173,#20815,#20816);
#17659=AXIS2_PLACEMENT_3D('',#43179,#20820,#20821);
#17660=AXIS2_PLACEMENT_3D('',#43182,#20824,#20825);
#17661=AXIS2_PLACEMENT_3D('',#43183,#20826,#20827);
#17662=AXIS2_PLACEMENT_3D('',#43192,#20832,#20833);
#17663=AXIS2_PLACEMENT_3D('',#43198,#20837,#20838);
#17664=AXIS2_PLACEMENT_3D('',#43204,#20842,#20843);
#17665=AXIS2_PLACEMENT_3D('',#43210,#20847,#20848);
#17666=AXIS2_PLACEMENT_3D('',#43216,#20852,#20853);
#17667=AXIS2_PLACEMENT_3D('',#43222,#20857,#20858);
#17668=AXIS2_PLACEMENT_3D('',#43228,#20862,#20863);
#17669=AXIS2_PLACEMENT_3D('',#43234,#20867,#20868);
#17670=AXIS2_PLACEMENT_3D('',#43240,#20872,#20873);
#17671=AXIS2_PLACEMENT_3D('',#43243,#20876,#20877);
#17672=AXIS2_PLACEMENT_3D('',#43244,#20878,#20879);
#17673=AXIS2_PLACEMENT_3D('',#43246,#20880,#20881);
#17674=AXIS2_PLACEMENT_3D('',#43248,#20882,#20883);
#17675=AXIS2_PLACEMENT_3D('',#43249,#20884,#20885);
#17676=AXIS2_PLACEMENT_3D('',#43252,#20887,#20888);
#17677=AXIS2_PLACEMENT_3D('',#43253,#20889,#20890);
#17678=AXIS2_PLACEMENT_3D('',#43256,#20892,#20893);
#17679=AXIS2_PLACEMENT_3D('',#43257,#20894,#20895);
#17680=AXIS2_PLACEMENT_3D('',#43258,#20896,#20897);
#17681=AXIS2_PLACEMENT_3D('',#43267,#20902,#20903);
#17682=AXIS2_PLACEMENT_3D('',#43269,#20904,#20905);
#17683=AXIS2_PLACEMENT_3D('',#43271,#20907,#20908);
#17684=AXIS2_PLACEMENT_3D('',#43275,#20911,#20912);
#17685=AXIS2_PLACEMENT_3D('',#43276,#20913,#20914);
#17686=AXIS2_PLACEMENT_3D('',#43277,#20915,#20916);
#17687=AXIS2_PLACEMENT_3D('',#43286,#20921,#20922);
#17688=AXIS2_PLACEMENT_3D('',#43288,#20923,#20924);
#17689=AXIS2_PLACEMENT_3D('',#43290,#20926,#20927);
#17690=AXIS2_PLACEMENT_3D('',#43294,#20930,#20931);
#17691=AXIS2_PLACEMENT_3D('',#43295,#20932,#20933);
#17692=AXIS2_PLACEMENT_3D('',#43296,#20934,#20935);
#17693=AXIS2_PLACEMENT_3D('',#43305,#20940,#20941);
#17694=AXIS2_PLACEMENT_3D('',#43307,#20942,#20943);
#17695=AXIS2_PLACEMENT_3D('',#43309,#20945,#20946);
#17696=AXIS2_PLACEMENT_3D('',#43313,#20949,#20950);
#17697=AXIS2_PLACEMENT_3D('',#43314,#20951,#20952);
#17698=AXIS2_PLACEMENT_3D('',#43315,#20953,#20954);
#17699=AXIS2_PLACEMENT_3D('',#43324,#20959,#20960);
#17700=AXIS2_PLACEMENT_3D('',#43326,#20961,#20962);
#17701=AXIS2_PLACEMENT_3D('',#43328,#20964,#20965);
#17702=AXIS2_PLACEMENT_3D('',#43332,#20968,#20969);
#17703=AXIS2_PLACEMENT_3D('',#43333,#20970,#20971);
#17704=AXIS2_PLACEMENT_3D('',#43334,#20972,#20973);
#17705=AXIS2_PLACEMENT_3D('',#43343,#20978,#20979);
#17706=AXIS2_PLACEMENT_3D('',#43345,#20980,#20981);
#17707=AXIS2_PLACEMENT_3D('',#43347,#20983,#20984);
#17708=AXIS2_PLACEMENT_3D('',#43351,#20987,#20988);
#17709=AXIS2_PLACEMENT_3D('',#43352,#20989,#20990);
#17710=AXIS2_PLACEMENT_3D('',#43353,#20991,#20992);
#17711=AXIS2_PLACEMENT_3D('',#43362,#20997,#20998);
#17712=AXIS2_PLACEMENT_3D('',#43364,#20999,#21000);
#17713=AXIS2_PLACEMENT_3D('',#43366,#21002,#21003);
#17714=AXIS2_PLACEMENT_3D('',#43370,#21006,#21007);
#17715=AXIS2_PLACEMENT_3D('',#43371,#21008,#21009);
#17716=AXIS2_PLACEMENT_3D('',#43372,#21010,#21011);
#17717=AXIS2_PLACEMENT_3D('',#43381,#21016,#21017);
#17718=AXIS2_PLACEMENT_3D('',#43383,#21018,#21019);
#17719=AXIS2_PLACEMENT_3D('',#43385,#21021,#21022);
#17720=AXIS2_PLACEMENT_3D('',#43389,#21025,#21026);
#17721=AXIS2_PLACEMENT_3D('',#43390,#21027,#21028);
#17722=AXIS2_PLACEMENT_3D('',#43391,#21029,#21030);
#17723=AXIS2_PLACEMENT_3D('',#43400,#21035,#21036);
#17724=AXIS2_PLACEMENT_3D('',#43402,#21037,#21038);
#17725=AXIS2_PLACEMENT_3D('',#43404,#21040,#21041);
#17726=AXIS2_PLACEMENT_3D('',#43408,#21044,#21045);
#17727=AXIS2_PLACEMENT_3D('',#43409,#21046,#21047);
#17728=AXIS2_PLACEMENT_3D('',#43410,#21048,#21049);
#17729=AXIS2_PLACEMENT_3D('',#43419,#21054,#21055);
#17730=AXIS2_PLACEMENT_3D('',#43421,#21056,#21057);
#17731=AXIS2_PLACEMENT_3D('',#43423,#21059,#21060);
#17732=AXIS2_PLACEMENT_3D('',#43427,#21063,#21064);
#17733=AXIS2_PLACEMENT_3D('',#43428,#21065,#21066);
#17734=AXIS2_PLACEMENT_3D('',#43429,#21067,#21068);
#17735=AXIS2_PLACEMENT_3D('',#43438,#21073,#21074);
#17736=AXIS2_PLACEMENT_3D('',#43440,#21075,#21076);
#17737=AXIS2_PLACEMENT_3D('',#43442,#21078,#21079);
#17738=AXIS2_PLACEMENT_3D('',#43446,#21082,#21083);
#17739=AXIS2_PLACEMENT_3D('',#43447,#21084,#21085);
#17740=AXIS2_PLACEMENT_3D('',#43448,#21086,#21087);
#17741=AXIS2_PLACEMENT_3D('',#43457,#21092,#21093);
#17742=AXIS2_PLACEMENT_3D('',#43459,#21094,#21095);
#17743=AXIS2_PLACEMENT_3D('',#43461,#21097,#21098);
#17744=AXIS2_PLACEMENT_3D('',#43465,#21101,#21102);
#17745=AXIS2_PLACEMENT_3D('',#43466,#21103,#21104);
#17746=AXIS2_PLACEMENT_3D('',#43467,#21105,#21106);
#17747=AXIS2_PLACEMENT_3D('',#43476,#21111,#21112);
#17748=AXIS2_PLACEMENT_3D('',#43478,#21113,#21114);
#17749=AXIS2_PLACEMENT_3D('',#43480,#21116,#21117);
#17750=AXIS2_PLACEMENT_3D('',#43484,#21120,#21121);
#17751=AXIS2_PLACEMENT_3D('',#43485,#21122,#21123);
#17752=AXIS2_PLACEMENT_3D('',#43486,#21124,#21125);
#17753=AXIS2_PLACEMENT_3D('',#43495,#21130,#21131);
#17754=AXIS2_PLACEMENT_3D('',#43497,#21132,#21133);
#17755=AXIS2_PLACEMENT_3D('',#43499,#21135,#21136);
#17756=AXIS2_PLACEMENT_3D('',#43503,#21139,#21140);
#17757=AXIS2_PLACEMENT_3D('',#43504,#21141,#21142);
#17758=AXIS2_PLACEMENT_3D('',#43505,#21143,#21144);
#17759=AXIS2_PLACEMENT_3D('',#43514,#21149,#21150);
#17760=AXIS2_PLACEMENT_3D('',#43516,#21151,#21152);
#17761=AXIS2_PLACEMENT_3D('',#43518,#21154,#21155);
#17762=AXIS2_PLACEMENT_3D('',#43522,#21158,#21159);
#17763=AXIS2_PLACEMENT_3D('',#43523,#21160,#21161);
#17764=AXIS2_PLACEMENT_3D('',#43524,#21162,#21163);
#17765=AXIS2_PLACEMENT_3D('',#43533,#21168,#21169);
#17766=AXIS2_PLACEMENT_3D('',#43535,#21170,#21171);
#17767=AXIS2_PLACEMENT_3D('',#43538,#21173,#21174);
#17768=AXIS2_PLACEMENT_3D('',#43539,#21175,#21176);
#17769=AXIS2_PLACEMENT_3D('',#43543,#21179,#21180);
#17770=AXIS2_PLACEMENT_3D('',#43545,#21181,#21182);
#17771=AXIS2_PLACEMENT_3D('',#43546,#21183,#21184);
#17772=AXIS2_PLACEMENT_3D('',#43547,#21185,#21186);
#17773=AXIS2_PLACEMENT_3D('',#43556,#21191,#21192);
#17774=AXIS2_PLACEMENT_3D('',#43558,#21193,#21194);
#17775=AXIS2_PLACEMENT_3D('',#43560,#21196,#21197);
#17776=AXIS2_PLACEMENT_3D('',#43564,#21200,#21201);
#17777=AXIS2_PLACEMENT_3D('',#43565,#21202,#21203);
#17778=AXIS2_PLACEMENT_3D('',#43566,#21204,#21205);
#17779=AXIS2_PLACEMENT_3D('',#43575,#21210,#21211);
#17780=AXIS2_PLACEMENT_3D('',#43577,#21212,#21213);
#17781=AXIS2_PLACEMENT_3D('',#43579,#21215,#21216);
#17782=AXIS2_PLACEMENT_3D('',#43583,#21219,#21220);
#17783=AXIS2_PLACEMENT_3D('',#43584,#21221,#21222);
#17784=AXIS2_PLACEMENT_3D('',#43585,#21223,#21224);
#17785=AXIS2_PLACEMENT_3D('',#43594,#21229,#21230);
#17786=AXIS2_PLACEMENT_3D('',#43596,#21231,#21232);
#17787=AXIS2_PLACEMENT_3D('',#43598,#21234,#21235);
#17788=AXIS2_PLACEMENT_3D('',#43602,#21238,#21239);
#17789=AXIS2_PLACEMENT_3D('',#43603,#21240,#21241);
#17790=AXIS2_PLACEMENT_3D('',#43604,#21242,#21243);
#17791=AXIS2_PLACEMENT_3D('',#43613,#21248,#21249);
#17792=AXIS2_PLACEMENT_3D('',#43615,#21250,#21251);
#17793=AXIS2_PLACEMENT_3D('',#43617,#21253,#21254);
#17794=AXIS2_PLACEMENT_3D('',#43621,#21257,#21258);
#17795=AXIS2_PLACEMENT_3D('',#43622,#21259,#21260);
#17796=AXIS2_PLACEMENT_3D('',#43623,#21261,#21262);
#17797=AXIS2_PLACEMENT_3D('',#43632,#21267,#21268);
#17798=AXIS2_PLACEMENT_3D('',#43634,#21269,#21270);
#17799=AXIS2_PLACEMENT_3D('',#43636,#21272,#21273);
#17800=AXIS2_PLACEMENT_3D('',#43640,#21276,#21277);
#17801=AXIS2_PLACEMENT_3D('',#43641,#21278,#21279);
#17802=AXIS2_PLACEMENT_3D('',#43642,#21280,#21281);
#17803=AXIS2_PLACEMENT_3D('',#43651,#21286,#21287);
#17804=AXIS2_PLACEMENT_3D('',#43653,#21288,#21289);
#17805=AXIS2_PLACEMENT_3D('',#43655,#21291,#21292);
#17806=AXIS2_PLACEMENT_3D('',#43659,#21295,#21296);
#17807=AXIS2_PLACEMENT_3D('',#43660,#21297,#21298);
#17808=AXIS2_PLACEMENT_3D('',#43661,#21299,#21300);
#17809=AXIS2_PLACEMENT_3D('',#43670,#21305,#21306);
#17810=AXIS2_PLACEMENT_3D('',#43672,#21307,#21308);
#17811=AXIS2_PLACEMENT_3D('',#43674,#21310,#21311);
#17812=AXIS2_PLACEMENT_3D('',#43678,#21314,#21315);
#17813=AXIS2_PLACEMENT_3D('',#43679,#21316,#21317);
#17814=AXIS2_PLACEMENT_3D('',#43680,#21318,#21319);
#17815=AXIS2_PLACEMENT_3D('',#43689,#21324,#21325);
#17816=AXIS2_PLACEMENT_3D('',#43691,#21326,#21327);
#17817=AXIS2_PLACEMENT_3D('',#43693,#21329,#21330);
#17818=AXIS2_PLACEMENT_3D('',#43697,#21333,#21334);
#17819=AXIS2_PLACEMENT_3D('',#43698,#21335,#21336);
#17820=AXIS2_PLACEMENT_3D('',#43699,#21337,#21338);
#17821=AXIS2_PLACEMENT_3D('',#43708,#21343,#21344);
#17822=AXIS2_PLACEMENT_3D('',#43710,#21345,#21346);
#17823=AXIS2_PLACEMENT_3D('',#43712,#21348,#21349);
#17824=AXIS2_PLACEMENT_3D('',#43716,#21352,#21353);
#17825=AXIS2_PLACEMENT_3D('',#43717,#21354,#21355);
#17826=AXIS2_PLACEMENT_3D('',#43718,#21356,#21357);
#17827=AXIS2_PLACEMENT_3D('',#43727,#21362,#21363);
#17828=AXIS2_PLACEMENT_3D('',#43729,#21364,#21365);
#17829=AXIS2_PLACEMENT_3D('',#43731,#21367,#21368);
#17830=AXIS2_PLACEMENT_3D('',#43735,#21371,#21372);
#17831=AXIS2_PLACEMENT_3D('',#43736,#21373,#21374);
#17832=AXIS2_PLACEMENT_3D('',#43737,#21375,#21376);
#17833=AXIS2_PLACEMENT_3D('',#43746,#21381,#21382);
#17834=AXIS2_PLACEMENT_3D('',#43748,#21383,#21384);
#17835=AXIS2_PLACEMENT_3D('',#43750,#21386,#21387);
#17836=AXIS2_PLACEMENT_3D('',#43754,#21390,#21391);
#17837=AXIS2_PLACEMENT_3D('',#43755,#21392,#21393);
#17838=AXIS2_PLACEMENT_3D('',#43756,#21394,#21395);
#17839=AXIS2_PLACEMENT_3D('',#43765,#21400,#21401);
#17840=AXIS2_PLACEMENT_3D('',#43767,#21402,#21403);
#17841=AXIS2_PLACEMENT_3D('',#43769,#21405,#21406);
#17842=AXIS2_PLACEMENT_3D('',#43773,#21409,#21410);
#17843=AXIS2_PLACEMENT_3D('',#43774,#21411,#21412);
#17844=AXIS2_PLACEMENT_3D('',#43775,#21413,#21414);
#17845=AXIS2_PLACEMENT_3D('',#43784,#21419,#21420);
#17846=AXIS2_PLACEMENT_3D('',#43786,#21421,#21422);
#17847=AXIS2_PLACEMENT_3D('',#43788,#21424,#21425);
#17848=AXIS2_PLACEMENT_3D('',#43792,#21428,#21429);
#17849=AXIS2_PLACEMENT_3D('',#43793,#21430,#21431);
#17850=AXIS2_PLACEMENT_3D('',#43794,#21432,#21433);
#17851=AXIS2_PLACEMENT_3D('',#43803,#21438,#21439);
#17852=AXIS2_PLACEMENT_3D('',#43805,#21440,#21441);
#17853=AXIS2_PLACEMENT_3D('',#43807,#21443,#21444);
#17854=AXIS2_PLACEMENT_3D('',#43811,#21447,#21448);
#17855=AXIS2_PLACEMENT_3D('',#43812,#21449,#21450);
#17856=AXIS2_PLACEMENT_3D('',#43813,#21451,#21452);
#17857=AXIS2_PLACEMENT_3D('',#43822,#21457,#21458);
#17858=AXIS2_PLACEMENT_3D('',#43824,#21459,#21460);
#17859=AXIS2_PLACEMENT_3D('',#43826,#21462,#21463);
#17860=AXIS2_PLACEMENT_3D('',#43830,#21466,#21467);
#17861=AXIS2_PLACEMENT_3D('',#43831,#21468,#21469);
#17862=AXIS2_PLACEMENT_3D('',#43832,#21470,#21471);
#17863=AXIS2_PLACEMENT_3D('',#43834,#21472,#21473);
#17864=AXIS2_PLACEMENT_3D('',#43835,#21474,#21475);
#17865=AXIS2_PLACEMENT_3D('',#43837,#21476,#21477);
#17866=AXIS2_PLACEMENT_3D('',#43839,#21479,#21480);
#17867=AXIS2_PLACEMENT_3D('',#43841,#21482,#21483);
#17868=AXIS2_PLACEMENT_3D('',#43842,#21484,#21485);
#17869=AXIS2_PLACEMENT_3D('',#43844,#21486,#21487);
#17870=AXIS2_PLACEMENT_3D('',#43846,#21489,#21490);
#17871=AXIS2_PLACEMENT_3D('',#43848,#21491,#21492);
#17872=AXIS2_PLACEMENT_3D('',#43849,#21493,#21494);
#17873=AXIS2_PLACEMENT_3D('',#43851,#21495,#21496);
#17874=AXIS2_PLACEMENT_3D('',#43853,#21498,#21499);
#17875=AXIS2_PLACEMENT_3D('',#43855,#21500,#21501);
#17876=AXIS2_PLACEMENT_3D('',#43858,#21504,#21505);
#17877=AXIS2_PLACEMENT_3D('',#43860,#21506,#21507);
#17878=AXIS2_PLACEMENT_3D('',#43862,#21509,#21510);
#17879=AXIS2_PLACEMENT_3D('',#43863,#21511,#21512);
#17880=AXIS2_PLACEMENT_3D('',#43864,#21513,#21514);
#17881=AXIS2_PLACEMENT_3D('',#43873,#21519,#21520);
#17882=AXIS2_PLACEMENT_3D('',#43879,#21524,#21525);
#17883=AXIS2_PLACEMENT_3D('',#43888,#21530,#21531);
#17884=AXIS2_PLACEMENT_3D('',#43894,#21535,#21536);
#17885=AXIS2_PLACEMENT_3D('',#43905,#21542,#21543);
#17886=AXIS2_PLACEMENT_3D('',#43911,#21547,#21548);
#17887=AXIS2_PLACEMENT_3D('',#43914,#21550,#21551);
#17888=AXIS2_PLACEMENT_3D('',#43915,#21552,#21553);
#17889=AXIS2_PLACEMENT_3D('',#43916,#21554,#21555);
#17890=AXIS2_PLACEMENT_3D('',#43920,#21558,#21559);
#17891=AXIS2_PLACEMENT_3D('',#43924,#21562,#21563);
#17892=AXIS2_PLACEMENT_3D('',#43926,#21564,#21565);
#17893=AXIS2_PLACEMENT_3D('',#43927,#21566,#21567);
#17894=AXIS2_PLACEMENT_3D('',#43938,#21573,#21574);
#17895=AXIS2_PLACEMENT_3D('',#43944,#21578,#21579);
#17896=AXIS2_PLACEMENT_3D('',#43946,#21580,#21581);
#17897=AXIS2_PLACEMENT_3D('',#43949,#21583,#21584);
#17898=AXIS2_PLACEMENT_3D('',#43950,#21585,#21586);
#17899=AXIS2_PLACEMENT_3D('',#43953,#21589,#21590);
#17900=AXIS2_PLACEMENT_3D('',#43962,#21595,#21596);
#17901=AXIS2_PLACEMENT_3D('',#43963,#21597,#21598);
#17902=AXIS2_PLACEMENT_3D('',#43967,#21601,#21602);
#17903=AXIS2_PLACEMENT_3D('',#43971,#21605,#21606);
#17904=AXIS2_PLACEMENT_3D('',#43974,#21608,#21609);
#17905=AXIS2_PLACEMENT_3D('',#43975,#21610,#21611);
#17906=AXIS2_PLACEMENT_3D('',#43984,#21617,#21618);
#17907=AXIS2_PLACEMENT_3D('',#44175,#21621,#21622);
#17908=AXIS2_PLACEMENT_3D('',#44179,#21624,#21625);
#17909=AXIS2_PLACEMENT_3D('',#44182,#21628,#21629);
#17910=AXIS2_PLACEMENT_3D('',#44190,#21633,#21634);
#17911=AXIS2_PLACEMENT_3D('',#44195,#21637,#21638);
#17912=AXIS2_PLACEMENT_3D('',#44197,#21639,#21640);
#17913=AXIS2_PLACEMENT_3D('',#44198,#21641,#21642);
#17914=AXIS2_PLACEMENT_3D('',#44264,#21644,#21645);
#17915=AXIS2_PLACEMENT_3D('',#44266,#21646,#21647);
#17916=AXIS2_PLACEMENT_3D('',#44267,#21648,#21649);
#17917=AXIS2_PLACEMENT_3D('',#44458,#21653,#21654);
#17918=AXIS2_PLACEMENT_3D('',#44460,#21655,#21656);
#17919=AXIS2_PLACEMENT_3D('',#44462,#21658,#21659);
#17920=AXIS2_PLACEMENT_3D('',#44466,#21662,#21663);
#17921=AXIS2_PLACEMENT_3D('',#44468,#21664,#21665);
#17922=AXIS2_PLACEMENT_3D('',#44469,#21666,#21667);
#17923=AXIS2_PLACEMENT_3D('',#44761,#21673,#21674);
#17924=AXIS2_PLACEMENT_3D('',#44798,#21676,#21677);
#17925=AXIS2_PLACEMENT_3D('',#44799,#21678,#21679);
#17926=AXIS2_PLACEMENT_3D('',#44800,#21680,#21681);
#17927=AXIS2_PLACEMENT_3D('',#44803,#21683,#21684);
#17928=AXIS2_PLACEMENT_3D('',#44804,#21685,#21686);
#17929=AXIS2_PLACEMENT_3D('',#44806,#21688,#21689);
#17930=AXIS2_PLACEMENT_3D('',#44808,#21690,#21691);
#17931=AXIS2_PLACEMENT_3D('',#44810,#21693,#21694);
#17932=AXIS2_PLACEMENT_3D('',#44811,#21695,#21696);
#17933=AXIS2_PLACEMENT_3D('',#44812,#21697,#21698);
#17934=AXIS2_PLACEMENT_3D('',#44814,#21699,#21700);
#17935=AXIS2_PLACEMENT_3D('',#44816,#21701,#21702);
#17936=AXIS2_PLACEMENT_3D('',#44817,#21703,#21704);
#17937=AXIS2_PLACEMENT_3D('',#44819,#21705,#21706);
#17938=AXIS2_PLACEMENT_3D('',#44821,#21708,#21709);
#17939=AXIS2_PLACEMENT_3D('',#44823,#21710,#21711);
#17940=AXIS2_PLACEMENT_3D('',#44824,#21712,#21713);
#17941=AXIS2_PLACEMENT_3D('',#44825,#21714,#21715);
#17942=AXIS2_PLACEMENT_3D('',#44827,#21717,#21718);
#17943=AXIS2_PLACEMENT_3D('',#44830,#21721,#21722);
#17944=AXIS2_PLACEMENT_3D('',#44831,#21723,#21724);
#17945=AXIS2_PLACEMENT_3D('',#44833,#21726,#21727);
#17946=AXIS2_PLACEMENT_3D('',#44835,#21729,#21730);
#17947=AXIS2_PLACEMENT_3D('',#44837,#21732,#21733);
#17948=AXIS2_PLACEMENT_3D('',#44839,#21735,#21736);
#17949=AXIS2_PLACEMENT_3D('',#44841,#21737,#21738);
#17950=AXIS2_PLACEMENT_3D('',#44843,#21740,#21741);
#17951=AXIS2_PLACEMENT_3D('',#44844,#21742,#21743);
#17952=AXIS2_PLACEMENT_3D('',#44846,#21744,#21745);
#17953=AXIS2_PLACEMENT_3D('',#44847,#21746,#21747);
#17954=AXIS2_PLACEMENT_3D('',#44848,#21748,#21749);
#17955=AXIS2_PLACEMENT_3D('',#44849,#21750,#21751);
#17956=AXIS2_PLACEMENT_3D('',#44850,#21752,#21753);
#17957=AXIS2_PLACEMENT_3D('',#44851,#21754,#21755);
#17958=AXIS2_PLACEMENT_3D('',#44852,#21756,#21757);
#17959=AXIS2_PLACEMENT_3D('',#44853,#21758,#21759);
#17960=AXIS2_PLACEMENT_3D('',#44855,#21760,#21761);
#17961=AXIS2_PLACEMENT_3D('',#44858,#21763,#21764);
#17962=AXIS2_PLACEMENT_3D('',#44859,#21765,#21766);
#17963=AXIS2_PLACEMENT_3D('',#44862,#21768,#21769);
#17964=AXIS2_PLACEMENT_3D('',#44863,#21770,#21771);
#17965=AXIS2_PLACEMENT_3D('',#44865,#21772,#21773);
#17966=AXIS2_PLACEMENT_3D('',#44867,#21775,#21776);
#17967=AXIS2_PLACEMENT_3D('',#44870,#21778,#21779);
#17968=AXIS2_PLACEMENT_3D('',#44871,#21780,#21781);
#17969=AXIS2_PLACEMENT_3D('',#44873,#21782,#21783);
#17970=AXIS2_PLACEMENT_3D('',#44874,#21784,#21785);
#17971=AXIS2_PLACEMENT_3D('',#44876,#21786,#21787);
#17972=AXIS2_PLACEMENT_3D('',#44878,#21788,#21789);
#17973=AXIS2_PLACEMENT_3D('',#44880,#21790,#21791);
#17974=AXIS2_PLACEMENT_3D('',#44881,#21792,#21793);
#17975=AXIS2_PLACEMENT_3D('',#44882,#21794,#21795);
#17976=AXIS2_PLACEMENT_3D('',#44886,#21797,#21798);
#17977=AXIS2_PLACEMENT_3D('',#44887,#21799,#21800);
#17978=AXIS2_PLACEMENT_3D('',#44888,#21801,#21802);
#17979=AXIS2_PLACEMENT_3D('',#44889,#21803,#21804);
#17980=AXIS2_PLACEMENT_3D('',#44891,#21805,#21806);
#17981=AXIS2_PLACEMENT_3D('',#44892,#21807,#21808);
#17982=AXIS2_PLACEMENT_3D('',#44894,#21809,#21810);
#17983=AXIS2_PLACEMENT_3D('',#44895,#21811,#21812);
#17984=AXIS2_PLACEMENT_3D('',#44896,#21813,#21814);
#17985=AXIS2_PLACEMENT_3D('',#44898,#21816,#21817);
#17986=AXIS2_PLACEMENT_3D('',#44899,#21818,#21819);
#17987=AXIS2_PLACEMENT_3D('',#44900,#21820,#21821);
#17988=AXIS2_PLACEMENT_3D('',#44901,#21822,#21823);
#17989=AXIS2_PLACEMENT_3D('',#44906,#21825,#21826);
#17990=AXIS2_PLACEMENT_3D('',#44909,#21828,#21829);
#17991=AXIS2_PLACEMENT_3D('',#44910,#21830,#21831);
#17992=AXIS2_PLACEMENT_3D('',#44916,#21835,#21836);
#17993=AXIS2_PLACEMENT_3D('',#44920,#21838,#21839);
#17994=AXIS2_PLACEMENT_3D('',#44921,#21840,#21841);
#17995=AXIS2_PLACEMENT_3D('',#44922,#21842,#21843);
#17996=AXIS2_PLACEMENT_3D('',#44925,#21846,#21847);
#17997=AXIS2_PLACEMENT_3D('',#44931,#21851,#21852);
#17998=AXIS2_PLACEMENT_3D('',#44934,#21854,#21855);
#17999=AXIS2_PLACEMENT_3D('',#44935,#21856,#21857);
#18000=AXIS2_PLACEMENT_3D('',#44937,#21858,#21859);
#18001=AXIS2_PLACEMENT_3D('',#44939,#21860,#21861);
#18002=AXIS2_PLACEMENT_3D('',#44940,#21862,#21863);
#18003=AXIS2_PLACEMENT_3D('',#44946,#21867,#21868);
#18004=AXIS2_PLACEMENT_3D('',#44949,#21870,#21871);
#18005=AXIS2_PLACEMENT_3D('',#44950,#21872,#21873);
#18006=AXIS2_PLACEMENT_3D('',#44956,#21877,#21878);
#18007=AXIS2_PLACEMENT_3D('',#44957,#21879,#21880);
#18008=AXIS2_PLACEMENT_3D('',#44958,#21881,#21882);
#18009=AXIS2_PLACEMENT_3D('',#44959,#21883,#21884);
#18010=AXIS2_PLACEMENT_3D('',#44963,#21886,#21887);
#18011=AXIS2_PLACEMENT_3D('',#44965,#21889,#21890);
#18012=AXIS2_PLACEMENT_3D('',#44969,#21893,#21894);
#18013=AXIS2_PLACEMENT_3D('',#44975,#21898,#21899);
#18014=AXIS2_PLACEMENT_3D('',#44978,#21901,#21902);
#18015=AXIS2_PLACEMENT_3D('',#44979,#21903,#21904);
#18016=AXIS2_PLACEMENT_3D('',#44985,#21908,#21909);
#18017=AXIS2_PLACEMENT_3D('',#44986,#21910,#21911);
#18018=AXIS2_PLACEMENT_3D('',#44987,#21912,#21913);
#18019=AXIS2_PLACEMENT_3D('',#44988,#21914,#21915);
#18020=AXIS2_PLACEMENT_3D('',#44990,#21917,#21918);
#18021=AXIS2_PLACEMENT_3D('',#44992,#21919,#21920);
#18022=AXIS2_PLACEMENT_3D('',#44994,#21921,#21922);
#18023=AXIS2_PLACEMENT_3D('',#44995,#21923,#21924);
#18024=AXIS2_PLACEMENT_3D('',#44996,#21925,#21926);
#18025=AXIS2_PLACEMENT_3D('',#44998,#21928,#21929);
#18026=AXIS2_PLACEMENT_3D('',#45000,#21931,#21932);
#18027=AXIS2_PLACEMENT_3D('',#45002,#21934,#21935);
#18028=AXIS2_PLACEMENT_3D('',#45003,#21936,#21937);
#18029=AXIS2_PLACEMENT_3D('',#45004,#21938,#21939);
#18030=AXIS2_PLACEMENT_3D('',#45006,#21940,#21941);
#18031=AXIS2_PLACEMENT_3D('',#45007,#21942,#21943);
#18032=AXIS2_PLACEMENT_3D('',#45009,#21944,#21945);
#18033=AXIS2_PLACEMENT_3D('',#45011,#21947,#21948);
#18034=AXIS2_PLACEMENT_3D('',#45013,#21949,#21950);
#18035=AXIS2_PLACEMENT_3D('',#45015,#21952,#21953);
#18036=AXIS2_PLACEMENT_3D('',#45017,#21954,#21955);
#18037=AXIS2_PLACEMENT_3D('',#45018,#21956,#21957);
#18038=AXIS2_PLACEMENT_3D('',#45020,#21958,#21959);
#18039=AXIS2_PLACEMENT_3D('',#45022,#21961,#21962);
#18040=AXIS2_PLACEMENT_3D('',#45024,#21963,#21964);
#18041=AXIS2_PLACEMENT_3D('',#45025,#21965,#21966);
#18042=AXIS2_PLACEMENT_3D('',#45027,#21967,#21968);
#18043=AXIS2_PLACEMENT_3D('',#45029,#21970,#21971);
#18044=AXIS2_PLACEMENT_3D('',#45031,#21972,#21973);
#18045=AXIS2_PLACEMENT_3D('',#45032,#21974,#21975);
#18046=AXIS2_PLACEMENT_3D('',#45034,#21976,#21977);
#18047=AXIS2_PLACEMENT_3D('',#45036,#21979,#21980);
#18048=AXIS2_PLACEMENT_3D('',#45038,#21981,#21982);
#18049=AXIS2_PLACEMENT_3D('',#45039,#21983,#21984);
#18050=AXIS2_PLACEMENT_3D('',#45041,#21985,#21986);
#18051=AXIS2_PLACEMENT_3D('',#45043,#21988,#21989);
#18052=AXIS2_PLACEMENT_3D('',#45045,#21990,#21991);
#18053=AXIS2_PLACEMENT_3D('',#45047,#21993,#21994);
#18054=AXIS2_PLACEMENT_3D('',#45048,#21995,#21996);
#18055=AXIS2_PLACEMENT_3D('',#45049,#21997,#21998);
#18056=AXIS2_PLACEMENT_3D('',#45052,#21999,#22000);
#18057=AXIS2_PLACEMENT_3D('',#45059,#22001,#22002);
#18058=AXIS2_PLACEMENT_3D('',#45064,#22003,#22004);
#18059=AXIS2_PLACEMENT_3D('',#45070,#22008,#22009);
#18060=AXIS2_PLACEMENT_3D('',#45076,#22013,#22014);
#18061=AXIS2_PLACEMENT_3D('',#45079,#22017,#22018);
#18062=AXIS2_PLACEMENT_3D('',#45085,#22022,#22023);
#18063=AXIS2_PLACEMENT_3D('',#45088,#22025,#22026);
#18064=AXIS2_PLACEMENT_3D('',#45089,#22027,#22028);
#18065=AXIS2_PLACEMENT_3D('',#45091,#22029,#22030);
#18066=AXIS2_PLACEMENT_3D('',#45092,#22031,#22032);
#18067=AXIS2_PLACEMENT_3D('',#45099,#22033,#22034);
#18068=AXIS2_PLACEMENT_3D('',#45104,#22035,#22036);
#18069=AXIS2_PLACEMENT_3D('',#45108,#22039,#22040);
#18070=AXIS2_PLACEMENT_3D('',#45114,#22044,#22045);
#18071=AXIS2_PLACEMENT_3D('',#45117,#22048,#22049);
#18072=AXIS2_PLACEMENT_3D('',#45119,#22051,#22052);
#18073=AXIS2_PLACEMENT_3D('',#45121,#22053,#22054);
#18074=AXIS2_PLACEMENT_3D('',#45122,#22055,#22056);
#18075=AXIS2_PLACEMENT_3D('',#45124,#22058,#22059);
#18076=AXIS2_PLACEMENT_3D('',#45126,#22060,#22061);
#18077=AXIS2_PLACEMENT_3D('',#45127,#22062,#22063);
#18078=AXIS2_PLACEMENT_3D('',#45129,#22064,#22065);
#18079=AXIS2_PLACEMENT_3D('',#45130,#22066,#22067);
#18080=AXIS2_PLACEMENT_3D('',#45132,#22068,#22069);
#18081=AXIS2_PLACEMENT_3D('',#45134,#22071,#22072);
#18082=AXIS2_PLACEMENT_3D('',#45136,#22074,#22075);
#18083=AXIS2_PLACEMENT_3D('',#45137,#22076,#22077);
#18084=AXIS2_PLACEMENT_3D('',#45140,#22078,#22079);
#18085=AXIS2_PLACEMENT_3D('',#45144,#22081,#22082);
#18086=AXIS2_PLACEMENT_3D('',#45146,#22084,#22085);
#18087=AXIS2_PLACEMENT_3D('',#45152,#22089,#22090);
#18088=AXIS2_PLACEMENT_3D('',#45154,#22091,#22092);
#18089=AXIS2_PLACEMENT_3D('',#45156,#22093,#22094);
#18090=AXIS2_PLACEMENT_3D('',#45158,#22096,#22097);
#18091=AXIS2_PLACEMENT_3D('',#45161,#22100,#22101);
#18092=AXIS2_PLACEMENT_3D('',#45162,#22102,#22103);
#18093=AXIS2_PLACEMENT_3D('',#45163,#22104,#22105);
#18094=AXIS2_PLACEMENT_3D('',#45164,#22106,#22107);
#18095=AXIS2_PLACEMENT_3D('',#45165,#22108,#22109);
#18096=AXIS2_PLACEMENT_3D('',#45166,#22110,#22111);
#18097=AXIS2_PLACEMENT_3D('',#45167,#22112,#22113);
#18098=AXIS2_PLACEMENT_3D('',#45168,#22114,#22115);
#18099=AXIS2_PLACEMENT_3D('',#45169,#22116,#22117);
#18100=AXIS2_PLACEMENT_3D('',#45170,#22118,#22119);
#18101=AXIS2_PLACEMENT_3D('',#45171,#22120,#22121);
#18102=AXIS2_PLACEMENT_3D('',#45172,#22122,#22123);
#18103=AXIS2_PLACEMENT_3D('',#45173,#22124,#22125);
#18104=AXIS2_PLACEMENT_3D('',#45174,#22126,#22127);
#18105=AXIS2_PLACEMENT_3D('',#45175,#22128,#22129);
#18106=AXIS2_PLACEMENT_3D('',#45176,#22130,#22131);
#18107=AXIS2_PLACEMENT_3D('',#45177,#22132,#22133);
#18108=AXIS2_PLACEMENT_3D('',#45178,#22134,#22135);
#18109=AXIS2_PLACEMENT_3D('',#45179,#22136,#22137);
#18110=AXIS2_PLACEMENT_3D('',#45180,#22138,#22139);
#18111=AXIS2_PLACEMENT_3D('',#45181,#22140,#22141);
#18112=AXIS2_PLACEMENT_3D('',#45182,#22142,#22143);
#18113=AXIS2_PLACEMENT_3D('',#45183,#22144,#22145);
#18114=AXIS2_PLACEMENT_3D('',#45184,#22146,#22147);
#18115=AXIS2_PLACEMENT_3D('',#45185,#22148,#22149);
#18116=AXIS2_PLACEMENT_3D('',#45186,#22150,#22151);
#18117=AXIS2_PLACEMENT_3D('',#45187,#22152,#22153);
#18118=AXIS2_PLACEMENT_3D('',#45188,#22154,#22155);
#18119=AXIS2_PLACEMENT_3D('',#45189,#22156,#22157);
#18120=AXIS2_PLACEMENT_3D('',#45190,#22158,#22159);
#18121=AXIS2_PLACEMENT_3D('',#45191,#22160,#22161);
#18122=AXIS2_PLACEMENT_3D('',#45192,#22162,#22163);
#18123=DIRECTION('axis',(0.,0.,1.));
#18124=DIRECTION('refdir',(1.,0.,0.));
#18125=DIRECTION('axis',(0.,0.,1.));
#18126=DIRECTION('refdir',(1.,0.,0.));
#18127=DIRECTION('center_axis',(1.,0.,0.));
#18128=DIRECTION('ref_axis',(0.,-1.,0.));
#18129=DIRECTION('center_axis',(-1.,0.,0.));
#18130=DIRECTION('ref_axis',(0.,-1.,0.));
#18131=DIRECTION('center_axis',(-1.,0.,0.));
#18132=DIRECTION('ref_axis',(0.,-1.,0.));
#18133=DIRECTION('',(0.707106781186546,0.707106781186549,-8.65956056235495E-17));
#18134=DIRECTION('center_axis',(1.,0.,0.));
#18135=DIRECTION('ref_axis',(0.,-1.,0.));
#18136=DIRECTION('center_axis',(1.,0.,0.));
#18137=DIRECTION('ref_axis',(0.,1.,0.));
#18138=DIRECTION('center_axis',(1.,0.,0.));
#18139=DIRECTION('ref_axis',(0.,1.,0.));
#18140=DIRECTION('',(1.,0.,0.));
#18141=DIRECTION('center_axis',(-1.,0.,0.));
#18142=DIRECTION('ref_axis',(0.,0.,1.));
#18143=DIRECTION('center_axis',(1.,0.,0.));
#18144=DIRECTION('ref_axis',(0.,0.,-1.));
#18145=DIRECTION('center_axis',(-1.,0.,0.));
#18146=DIRECTION('ref_axis',(0.,1.,0.));
#18147=DIRECTION('center_axis',(-1.,0.,0.));
#18148=DIRECTION('ref_axis',(0.,1.,0.));
#18149=DIRECTION('',(0.707106781186546,0.707106781186549,-8.65956056235495E-17));
#18150=DIRECTION('center_axis',(1.,0.,0.));
#18151=DIRECTION('ref_axis',(0.,0.,-1.));
#18152=DIRECTION('center_axis',(1.,0.,0.));
#18153=DIRECTION('ref_axis',(0.,-1.,1.83697019872103E-16));
#18154=DIRECTION('',(0.,0.,-1.));
#18155=DIRECTION('',(0.,-1.,0.));
#18156=DIRECTION('',(0.,0.,1.));
#18157=DIRECTION('center_axis',(1.,0.,0.));
#18158=DIRECTION('ref_axis',(0.,1.,-6.12323399573677E-17));
#18159=DIRECTION('',(0.,0.,1.));
#18160=DIRECTION('',(0.,1.,0.));
#18161=DIRECTION('center_axis',(1.,0.,0.));
#18162=DIRECTION('ref_axis',(0.,-2.44929359829471E-16,-1.));
#18163=DIRECTION('',(0.,1.,0.));
#18164=DIRECTION('',(0.,0.,-1.));
#18165=DIRECTION('',(0.457581580857944,0.,-0.889167642719608));
#18166=DIRECTION('',(-0.457581580857943,0.,0.889167642719609));
#18167=DIRECTION('center_axis',(0.889167642719609,0.,0.457581580857943));
#18168=DIRECTION('ref_axis',(0.457581580857943,0.,-0.889167642719609));
#18169=DIRECTION('center_axis',(0.889167642719609,0.,0.457581580857943));
#18170=DIRECTION('ref_axis',(-0.457581580857943,0.,0.889167642719609));
#18171=DIRECTION('',(0.,-1.,0.));
#18172=DIRECTION('',(0.,1.,0.));
#18173=DIRECTION('center_axis',(0.,1.,0.));
#18174=DIRECTION('ref_axis',(1.,0.,0.));
#18175=DIRECTION('',(0.813733471206735,0.,-0.581238193719096));
#18176=DIRECTION('',(1.,0.,0.));
#18177=DIRECTION('',(0.707106781186547,0.,0.707106781186548));
#18178=DIRECTION('',(0.,0.,1.));
#18179=DIRECTION('',(-0.707106781186548,0.,0.707106781186547));
#18180=DIRECTION('',(-1.,0.,0.));
#18181=DIRECTION('',(0.,0.,-1.));
#18182=DIRECTION('center_axis',(0.,-1.,0.));
#18183=DIRECTION('ref_axis',(-0.707106781186548,0.,0.707106781186548));
#18184=DIRECTION('',(-1.,0.,0.));
#18185=DIRECTION('center_axis',(0.,-1.,0.));
#18186=DIRECTION('ref_axis',(0.707106781186548,0.,0.707106781186547));
#18187=DIRECTION('',(0.,0.,1.));
#18188=DIRECTION('',(1.,0.,0.));
#18189=DIRECTION('',(0.,0.,-1.));
#18190=DIRECTION('center_axis',(-0.813733471206735,0.,0.581238193719096));
#18191=DIRECTION('ref_axis',(0.410997468263393,-0.707106781186548,0.575396455568749));
#18192=DIRECTION('',(-0.813733471206735,0.,0.581238193719096));
#18193=DIRECTION('center_axis',(-0.813733471206735,0.,0.581238193719096));
#18194=DIRECTION('ref_axis',(0.410997468263392,-0.707106781186551,0.575396455568747));
#18195=DIRECTION('center_axis',(0.581238193719096,0.,0.813733471206735));
#18196=DIRECTION('ref_axis',(0.813733471206735,0.,-0.581238193719096));
#18197=DIRECTION('center_axis',(-0.581238193719096,0.,-0.813733471206735));
#18198=DIRECTION('ref_axis',(-0.813733471206735,0.,0.581238193719096));
#18199=DIRECTION('',(0.,-1.,0.));
#18200=DIRECTION('',(0.813733471206735,0.,-0.581238193719096));
#18201=DIRECTION('',(0.,1.,0.));
#18202=DIRECTION('',(-0.707106781186548,-0.707106781186548,0.));
#18203=DIRECTION('',(0.,0.707106781186546,0.707106781186549));
#18204=DIRECTION('',(1.08368419587492E-12,-0.707106781186914,-0.707106781186181));
#18205=DIRECTION('',(-0.392473756018299,-0.725569174564963,-0.565255450002923));
#18206=DIRECTION('',(0.0228311464870028,0.69541471336182,0.718245859848831));
#18207=DIRECTION('center_axis',(-0.500000000000002,0.707106781186544,-0.500000000000003));
#18208=DIRECTION('ref_axis',(-0.707106781186548,0.,0.707106781186547));
#18209=DIRECTION('',(0.499999999999997,0.707106781186549,0.500000000000002));
#18210=DIRECTION('',(0.707106781186548,0.,-0.707106781186547));
#18211=DIRECTION('',(-0.499999999999998,-0.707106781186551,-0.499999999999997));
#18212=DIRECTION('',(-0.707106781186548,0.,0.707106781186547));
#18213=DIRECTION('',(0.565255450002919,0.725569174564966,0.392473756018301));
#18214=DIRECTION('',(-0.718245859848833,-0.695414713361818,-0.022831146487005));
#18215=DIRECTION('',(0.707106781186178,0.707106781186917,-1.08089518879373E-12));
#18216=DIRECTION('center_axis',(0.,0.,1.));
#18217=DIRECTION('ref_axis',(-0.707106781186546,0.707106781186549,0.));
#18218=DIRECTION('',(0.,0.,1.));
#18219=DIRECTION('center_axis',(0.,0.,1.));
#18220=DIRECTION('ref_axis',(-1.,0.,0.));
#18221=DIRECTION('',(0.,0.,-1.));
#18222=DIRECTION('center_axis',(-1.,0.,0.));
#18223=DIRECTION('ref_axis',(0.,0.,1.));
#18224=DIRECTION('',(0.,1.,0.));
#18225=DIRECTION('',(0.,0.,-1.));
#18226=DIRECTION('',(0.,-1.,0.));
#18227=DIRECTION('center_axis',(0.,1.,0.));
#18228=DIRECTION('ref_axis',(-0.923879532511287,0.,-0.382683432365089));
#18229=DIRECTION('',(0.,-1.,0.));
#18230=DIRECTION('center_axis',(0.,1.,0.));
#18231=DIRECTION('ref_axis',(-0.707106781186548,0.,-0.707106781186547));
#18232=DIRECTION('center_axis',(-0.707106781186547,0.,-0.707106781186548));
#18233=DIRECTION('ref_axis',(-0.707106781186548,0.,0.707106781186547));
#18234=DIRECTION('',(0.,1.,0.));
#18235=DIRECTION('',(0.707106781186548,0.,-0.707106781186547));
#18236=DIRECTION('center_axis',(1.,0.,0.));
#18237=DIRECTION('ref_axis',(0.,-0.70710678118655,-0.707106781186545));
#18238=DIRECTION('center_axis',(1.,0.,0.));
#18239=DIRECTION('ref_axis',(0.,-1.,-2.96059473233374E-15));
#18240=DIRECTION('',(1.,0.,0.));
#18241=DIRECTION('center_axis',(-1.,0.,0.));
#18242=DIRECTION('ref_axis',(0.,0.,-1.));
#18243=DIRECTION('',(-1.,0.,0.));
#18244=DIRECTION('center_axis',(-0.816496580927727,-0.408248290463863,-0.408248290463861));
#18245=DIRECTION('ref_axis',(0.577350269189624,-0.577350269189629,-0.577350269189624));
#18246=DIRECTION('center_axis',(0.,-1.,0.));
#18247=DIRECTION('ref_axis',(0.70710678118655,0.,-0.707106781186545));
#18248=DIRECTION('center_axis',(0.,0.,-1.));
#18249=DIRECTION('ref_axis',(0.707106781186546,-0.707106781186549,0.));
#18250=DIRECTION('center_axis',(0.40824829046386,-0.816496580927727,0.408248290463865));
#18251=DIRECTION('ref_axis',(-0.577350269189623,-0.577350269189626,-0.577350269189628));
#18252=DIRECTION('center_axis',(0.,0.,-1.));
#18253=DIRECTION('ref_axis',(-0.707106781186546,-0.707106781186549,0.));
#18254=DIRECTION('center_axis',(0.,-1.,0.));
#18255=DIRECTION('ref_axis',(-0.707106781186546,0.,-0.707106781186549));
#18256=DIRECTION('center_axis',(0.,0.,1.));
#18257=DIRECTION('ref_axis',(0.707106781186548,-0.707106781186548,0.));
#18258=DIRECTION('',(0.,0.,1.));
#18259=DIRECTION('',(0.,0.,-1.));
#18260=DIRECTION('center_axis',(0.,1.,0.));
#18261=DIRECTION('ref_axis',(0.70710678118655,0.,-0.707106781186545));
#18262=DIRECTION('',(0.,1.,0.));
#18263=DIRECTION('',(0.,-1.,0.));
#18264=DIRECTION('center_axis',(0.,0.,-1.));
#18265=DIRECTION('ref_axis',(-1.,0.,0.));
#18266=DIRECTION('',(0.,-1.,0.));
#18267=DIRECTION('',(1.,0.,0.));
#18268=DIRECTION('center_axis',(0.,0.,1.));
#18269=DIRECTION('ref_axis',(1.,0.,0.));
#18270=DIRECTION('center_axis',(0.813733471206734,-1.72081073455594E-15,
-0.581238193719098));
#18271=DIRECTION('ref_axis',(0.581238193719098,0.,0.813733471206734));
#18272=DIRECTION('center_axis',(0.,1.,0.));
#18273=DIRECTION('ref_axis',(1.,0.,0.));
#18274=DIRECTION('center_axis',(0.,0.,1.));
#18275=DIRECTION('ref_axis',(0.,1.,0.));
#18276=DIRECTION('center_axis',(0.,1.,0.));
#18277=DIRECTION('ref_axis',(0.889167642719608,0.,0.457581580857944));
#18278=DIRECTION('',(0.,1.,0.));
#18279=DIRECTION('center_axis',(0.,0.,-1.));
#18280=DIRECTION('ref_axis',(0.707106781186543,0.707106781186552,0.));
#18281=DIRECTION('',(0.,0.,1.));
#18282=DIRECTION('',(0.,0.,-1.));
#18283=DIRECTION('center_axis',(0.141866792680437,-0.885380737596912,0.442690368798457));
#18284=DIRECTION('ref_axis',(0.27019821896378,0.464866593220407,0.843144099769698));
#18285=DIRECTION('center_axis',(1.,0.,0.));
#18286=DIRECTION('ref_axis',(0.,0.,1.));
#18287=DIRECTION('center_axis',(0.,1.,0.));
#18288=DIRECTION('ref_axis',(0.581238193719098,0.,0.813733471206734));
#18289=DIRECTION('center_axis',(-0.813733471206734,0.,0.581238193719098));
#18290=DIRECTION('ref_axis',(0.,1.,0.));
#18291=DIRECTION('center_axis',(-0.141866792680436,-0.885380737596912,-0.442690368798456));
#18292=DIRECTION('ref_axis',(0.27019821896378,-0.464866593220407,0.843144099769698));
#18293=DIRECTION('center_axis',(0.,-1.,0.));
#18294=DIRECTION('ref_axis',(0.581238193719094,0.,0.813733471206737));
#18295=DIRECTION('center_axis',(1.,0.,0.));
#18296=DIRECTION('ref_axis',(0.,-0.707106781186549,0.707106781186546));
#18297=DIRECTION('center_axis',(0.,1.,0.));
#18298=DIRECTION('ref_axis',(0.305177431007984,0.,0.952295508549404));
#18299=DIRECTION('',(0.,-1.,0.));
#18300=DIRECTION('center_axis',(0.813733471206735,0.,-0.581238193719096));
#18301=DIRECTION('ref_axis',(0.410997468263393,0.707106781186548,0.575396455568749));
#18302=DIRECTION('',(-0.813733471206735,0.,0.581238193719096));
#18303=DIRECTION('center_axis',(-0.182143211721526,-0.879465224064609,0.439732612032305));
#18304=DIRECTION('ref_axis',(-0.336556770590777,0.475963149477969,0.812519920068745));
#18305=DIRECTION('center_axis',(0.707106781186549,1.57009245868377E-15,
0.707106781186546));
#18306=DIRECTION('ref_axis',(-0.707106781186546,0.,0.707106781186549));
#18307=DIRECTION('center_axis',(0.,1.,0.));
#18308=DIRECTION('ref_axis',(0.,0.,1.));
#18309=DIRECTION('center_axis',(-1.,0.,1.48029736616687E-15));
#18310=DIRECTION('ref_axis',(0.,1.,0.));
#18311=DIRECTION('center_axis',(0.182143211721527,-0.879465224064609,-0.439732612032306));
#18312=DIRECTION('ref_axis',(-0.336556770590777,-0.475963149477967,0.812519920068746));
#18313=DIRECTION('center_axis',(0.,-1.,0.));
#18314=DIRECTION('ref_axis',(0.,0.,1.));
#18315=DIRECTION('center_axis',(0.707106781186547,0.,0.707106781186548));
#18316=DIRECTION('ref_axis',(-0.5,-0.707106781186548,0.5));
#18317=DIRECTION('center_axis',(-1.,0.,0.));
#18318=DIRECTION('ref_axis',(0.,-0.707106781186549,0.707106781186546));
#18319=DIRECTION('center_axis',(0.,1.,0.));
#18320=DIRECTION('ref_axis',(-0.382683432365088,0.,0.923879532511287));
#18321=DIRECTION('',(0.,1.,0.));
#18322=DIRECTION('',(0.,-1.,0.));
#18323=DIRECTION('center_axis',(1.,0.,0.));
#18324=DIRECTION('ref_axis',(0.,0.707106781186548,0.707106781186548));
#18325=DIRECTION('',(-1.,0.,0.));
#18326=DIRECTION('',(1.,0.,0.));
#18327=DIRECTION('center_axis',(0.,0.,1.));
#18328=DIRECTION('ref_axis',(1.,0.,0.));
#18329=DIRECTION('center_axis',(0.,1.,0.));
#18330=DIRECTION('ref_axis',(-0.707106781186548,0.,0.707106781186547));
#18331=DIRECTION('center_axis',(-0.707106781186548,0.,-0.707106781186548));
#18332=DIRECTION('ref_axis',(0.,1.,0.));
#18333=DIRECTION('center_axis',(0.,0.,1.));
#18334=DIRECTION('ref_axis',(1.,0.,0.));
#18335=DIRECTION('center_axis',(0.,-1.,0.));
#18336=DIRECTION('ref_axis',(-0.707106781186547,0.,0.707106781186548));
#18337=DIRECTION('center_axis',(0.,0.,1.));
#18338=DIRECTION('ref_axis',(-0.707106781186546,-0.707106781186549,0.));
#18339=DIRECTION('center_axis',(-0.707106781186547,0.,-0.707106781186548));
#18340=DIRECTION('ref_axis',(-0.499999999999999,-0.707106781186549,0.499999999999998));
#18341=DIRECTION('center_axis',(0.,1.,0.));
#18342=DIRECTION('ref_axis',(-0.923879532511287,0.,0.382683432365089));
#18343=DIRECTION('',(0.,1.,0.));
#18344=DIRECTION('center_axis',(0.707106781186547,0.,0.707106781186548));
#18345=DIRECTION('ref_axis',(-0.500000000000001,0.707106781186548,0.499999999999998));
#18346=DIRECTION('',(-0.707106781186547,0.,-0.707106781186548));
#18347=DIRECTION('',(0.707106781186547,0.,0.707106781186548));
#18348=DIRECTION('center_axis',(0.182143211721528,-0.879465224064609,0.439732612032306));
#18349=DIRECTION('ref_axis',(-0.336556770590778,-0.475963149477968,-0.812519920068745));
#18350=DIRECTION('center_axis',(0.,-1.,0.));
#18351=DIRECTION('ref_axis',(0.,0.,-1.));
#18352=DIRECTION('center_axis',(-1.,0.,0.));
#18353=DIRECTION('ref_axis',(0.,-1.,0.));
#18354=DIRECTION('center_axis',(0.707106781186548,5.23364152894591E-16,
-0.707106781186547));
#18355=DIRECTION('ref_axis',(-0.707106781186547,0.,-0.707106781186548));
#18356=DIRECTION('center_axis',(1.,0.,0.));
#18357=DIRECTION('ref_axis',(0.,-0.70710678118655,-0.707106781186545));
#18358=DIRECTION('center_axis',(-1.,-2.96059473233374E-15,-2.96059473233375E-15));
#18359=DIRECTION('ref_axis',(2.96059473233375E-15,0.,-1.));
#18360=DIRECTION('',(1.,0.,0.));
#18361=DIRECTION('center_axis',(-0.816496580927726,-0.408248290463864,-0.408248290463862));
#18362=DIRECTION('ref_axis',(0.577350269189625,-0.577350269189627,-0.577350269189625));
#18363=DIRECTION('center_axis',(0.,-1.,0.));
#18364=DIRECTION('ref_axis',(0.707106781186549,0.,-0.707106781186546));
#18365=DIRECTION('center_axis',(0.,0.,-1.));
#18366=DIRECTION('ref_axis',(0.707106781186546,-0.707106781186549,0.));
#18367=DIRECTION('center_axis',(0.707106781186548,0.,-0.707106781186547));
#18368=DIRECTION('ref_axis',(-0.500000000000001,-0.707106781186548,-0.499999999999998));
#18369=DIRECTION('center_axis',(0.707106781186548,0.,-0.707106781186547));
#18370=DIRECTION('ref_axis',(0.,-1.,0.));
#18371=DIRECTION('center_axis',(0.,1.,0.));
#18372=DIRECTION('ref_axis',(-0.38268343236509,0.,-0.923879532511287));
#18373=DIRECTION('',(0.,-1.,0.));
#18374=DIRECTION('center_axis',(-0.816496580927726,0.408248290463864,-0.408248290463862));
#18375=DIRECTION('ref_axis',(0.577350269189625,0.577350269189627,-0.577350269189625));
#18376=DIRECTION('center_axis',(1.,0.,0.));
#18377=DIRECTION('ref_axis',(0.,0.,-1.));
#18378=DIRECTION('center_axis',(0.,0.,-1.));
#18379=DIRECTION('ref_axis',(0.707106781186546,0.707106781186549,0.));
#18380=DIRECTION('center_axis',(0.,1.,0.));
#18381=DIRECTION('ref_axis',(0.707106781186549,0.,-0.707106781186546));
#18382=DIRECTION('center_axis',(-1.,0.,0.));
#18383=DIRECTION('ref_axis',(0.,0.70710678118655,-0.707106781186545));
#18384=DIRECTION('',(1.,0.,0.));
#18385=DIRECTION('',(-1.,0.,0.));
#18386=DIRECTION('center_axis',(0.,0.,1.));
#18387=DIRECTION('ref_axis',(1.,0.,0.));
#18388=DIRECTION('center_axis',(0.,0.,-1.));
#18389=DIRECTION('ref_axis',(-0.707106781186546,-0.707106781186549,0.));
#18390=DIRECTION('center_axis',(0.,0.,1.));
#18391=DIRECTION('ref_axis',(1.,0.,0.));
#18392=DIRECTION('',(-1.,0.,0.));
#18393=DIRECTION('',(-1.,0.,0.));
#18394=DIRECTION('',(0.,-1.,0.));
#18395=DIRECTION('',(-1.,0.,0.));
#18396=DIRECTION('',(0.,1.,0.));
#18397=DIRECTION('',(-1.,0.,0.));
#18398=DIRECTION('',(0.,1.,0.));
#18399=DIRECTION('',(1.,0.,0.));
#18400=DIRECTION('',(0.,-1.,0.));
#18401=DIRECTION('',(-0.555699076657711,0.831383507294779,0.));
#18402=DIRECTION('',(0.,-1.,0.));
#18403=DIRECTION('',(-1.,0.,0.));
#18404=DIRECTION('',(0.,1.,0.));
#18405=DIRECTION('',(1.,0.,0.));
#18406=DIRECTION('',(0.556032582744129,-0.831160494084562,0.));
#18407=DIRECTION('',(0.,1.,0.));
#18408=DIRECTION('',(1.,0.,0.));
#18409=DIRECTION('',(0.,-1.,0.));
#18410=DIRECTION('',(-1.,0.,0.));
#18411=DIRECTION('center_axis',(-0.707106781186548,0.,0.707106781186547));
#18412=DIRECTION('ref_axis',(0.707106781186547,0.,0.707106781186548));
#18413=DIRECTION('',(-0.707106781186547,0.,-0.707106781186548));
#18414=DIRECTION('center_axis',(-0.707106781186547,0.,-0.707106781186548));
#18415=DIRECTION('ref_axis',(-0.500000000000001,-0.707106781186548,0.499999999999998));
#18416=DIRECTION('center_axis',(0.,0.,-1.));
#18417=DIRECTION('ref_axis',(-0.707106781186546,-0.707106781186549,0.));
#18418=DIRECTION('center_axis',(0.,0.,1.));
#18419=DIRECTION('ref_axis',(0.707106781186546,-0.707106781186549,0.));
#18420=DIRECTION('',(0.,0.,1.));
#18421=DIRECTION('center_axis',(0.,0.,1.));
#18422=DIRECTION('ref_axis',(0.,-1.,0.));
#18423=DIRECTION('center_axis',(0.,0.,-1.));
#18424=DIRECTION('ref_axis',(-1.,0.,0.));
#18425=DIRECTION('',(0.,1.,0.));
#18426=DIRECTION('center_axis',(0.,-1.,0.));
#18427=DIRECTION('ref_axis',(0.707106781186548,0.,-0.707106781186547));
#18428=DIRECTION('',(0.,-1.,0.));
#18429=DIRECTION('center_axis',(0.,0.,-1.));
#18430=DIRECTION('ref_axis',(0.707106781186546,0.707106781186549,0.));
#18431=DIRECTION('',(0.,0.,1.));
#18432=DIRECTION('center_axis',(0.,0.,1.));
#18433=DIRECTION('ref_axis',(1.,0.,0.));
#18434=DIRECTION('',(0.,0.,-1.));
#18435=DIRECTION('center_axis',(-1.,0.,0.));
#18436=DIRECTION('ref_axis',(0.,-0.707106781186548,0.707106781186548));
#18437=DIRECTION('center_axis',(0.,0.,1.));
#18438=DIRECTION('ref_axis',(0.707106781186543,-0.707106781186552,0.));
#18439=DIRECTION('',(0.,0.,1.));
#18440=DIRECTION('center_axis',(1.,0.,0.));
#18441=DIRECTION('ref_axis',(0.,0.,-1.));
#18442=DIRECTION('center_axis',(-1.,0.,0.));
#18443=DIRECTION('ref_axis',(0.,1.,0.));
#18444=DIRECTION('center_axis',(1.,0.,0.));
#18445=DIRECTION('ref_axis',(0.,0.,-1.));
#18446=DIRECTION('center_axis',(-1.,0.,0.));
#18447=DIRECTION('ref_axis',(0.,1.,0.));
#18448=DIRECTION('center_axis',(0.,0.,-1.));
#18449=DIRECTION('ref_axis',(-0.707106781186548,-0.707106781186548,0.));
#18450=DIRECTION('',(0.,0.,1.));
#18451=DIRECTION('center_axis',(0.,1.,0.));
#18452=DIRECTION('ref_axis',(-0.707106781186548,0.,-0.707106781186548));
#18453=DIRECTION('center_axis',(0.,1.,0.));
#18454=DIRECTION('ref_axis',(1.,0.,0.));
#18455=DIRECTION('',(-1.,0.,0.));
#18456=DIRECTION('center_axis',(-0.408248290463863,-0.816496580927726,-0.408248290463863));
#18457=DIRECTION('ref_axis',(-0.577350269189626,0.577350269189626,-0.577350269189626));
#18458=DIRECTION('center_axis',(-1.,0.,0.));
#18459=DIRECTION('ref_axis',(0.,0.,-1.));
#18460=DIRECTION('center_axis',(0.,1.,0.));
#18461=DIRECTION('ref_axis',(-1.,0.,0.));
#18462=DIRECTION('center_axis',(-5.92118946466749E-15,0.,-1.));
#18463=DIRECTION('ref_axis',(0.,1.,0.));
#18464=DIRECTION('center_axis',(0.,1.,0.));
#18465=DIRECTION('ref_axis',(-0.707106781186548,0.,-0.707106781186548));
#18466=DIRECTION('',(0.,-1.,0.));
#18467=DIRECTION('center_axis',(0.,0.,1.));
#18468=DIRECTION('ref_axis',(-0.707106781186548,0.707106781186548,0.));
#18469=DIRECTION('',(0.,0.,-1.));
#18470=DIRECTION('center_axis',(-0.816496580927726,0.408248290463865,-0.408248290463861));
#18471=DIRECTION('ref_axis',(0.577350269189631,0.577350269189626,-0.577350269189621));
#18472=DIRECTION('center_axis',(1.,0.,0.));
#18473=DIRECTION('ref_axis',(0.,0.,-1.));
#18474=DIRECTION('center_axis',(0.,0.,-1.));
#18475=DIRECTION('ref_axis',(0.707106781186546,0.707106781186549,0.));
#18476=DIRECTION('center_axis',(0.,1.,0.));
#18477=DIRECTION('ref_axis',(0.70710678118655,0.,-0.707106781186545));
#18478=DIRECTION('center_axis',(-1.,0.,0.));
#18479=DIRECTION('ref_axis',(0.,0.70710678118655,-0.707106781186545));
#18480=DIRECTION('',(-1.,0.,0.));
#18481=DIRECTION('',(1.,0.,0.));
#18482=DIRECTION('center_axis',(0.,0.,-1.));
#18483=DIRECTION('ref_axis',(-1.,0.,0.));
#18484=DIRECTION('',(0.,1.,0.));
#18485=DIRECTION('',(-1.,0.,0.));
#18486=DIRECTION('center_axis',(0.,1.,0.));
#18487=DIRECTION('ref_axis',(0.70710678118655,0.,-0.707106781186545));
#18488=DIRECTION('',(0.,-1.,0.));
#18489=DIRECTION('center_axis',(0.,0.,-1.));
#18490=DIRECTION('ref_axis',(0.707106781186548,0.707106781186548,0.));
#18491=DIRECTION('',(0.,0.,1.));
#18492=DIRECTION('',(0.,0.,-1.));
#18493=DIRECTION('center_axis',(1.,0.,0.));
#18494=DIRECTION('ref_axis',(0.,0.,-1.));
#18495=DIRECTION('center_axis',(-1.,0.,0.));
#18496=DIRECTION('ref_axis',(0.,1.,0.));
#18497=DIRECTION('center_axis',(1.,0.,0.));
#18498=DIRECTION('ref_axis',(0.,0.,-1.));
#18499=DIRECTION('center_axis',(-1.,0.,0.));
#18500=DIRECTION('ref_axis',(0.,-1.,1.83697019872103E-16));
#18501=DIRECTION('center_axis',(0.,-1.,-1.22464679914735E-16));
#18502=DIRECTION('ref_axis',(0.,-1.22464679914735E-16,1.));
#18503=DIRECTION('center_axis',(1.,0.,0.));
#18504=DIRECTION('ref_axis',(0.,-1.,3.06161699786838E-17));
#18505=DIRECTION('center_axis',(1.,0.,0.));
#18506=DIRECTION('ref_axis',(0.,-1.,3.06161699786838E-17));
#18507=DIRECTION('center_axis',(-1.,0.,0.));
#18508=DIRECTION('ref_axis',(0.,1.,0.));
#18509=DIRECTION('',(-0.707106781186546,-0.707106781186549,-8.65956056235495E-17));
#18510=DIRECTION('center_axis',(-1.,0.,0.));
#18511=DIRECTION('ref_axis',(0.,-1.,3.06161699786838E-17));
#18512=DIRECTION('center_axis',(-1.,0.,0.));
#18513=DIRECTION('ref_axis',(0.,-1.,3.06161699786838E-17));
#18514=DIRECTION('center_axis',(1.,0.,0.));
#18515=DIRECTION('ref_axis',(0.,0.,-1.));
#18516=DIRECTION('center_axis',(-1.,0.,0.));
#18517=DIRECTION('ref_axis',(0.,1.,0.));
#18518=DIRECTION('center_axis',(1.,0.,0.));
#18519=DIRECTION('ref_axis',(0.,0.,-1.));
#18520=DIRECTION('center_axis',(0.,-1.,-1.22464679914735E-16));
#18521=DIRECTION('ref_axis',(0.,-1.22464679914735E-16,1.));
#18522=DIRECTION('center_axis',(1.,0.,0.));
#18523=DIRECTION('ref_axis',(0.,-1.,1.83697019872103E-16));
#18524=DIRECTION('center_axis',(1.,0.,0.));
#18525=DIRECTION('ref_axis',(0.,-1.,1.83697019872103E-16));
#18526=DIRECTION('center_axis',(1.,0.,0.));
#18527=DIRECTION('ref_axis',(0.,1.,0.));
#18528=DIRECTION('',(-1.,0.,0.));
#18529=DIRECTION('center_axis',(-1.,0.,0.));
#18530=DIRECTION('ref_axis',(0.,-1.,1.83697019872103E-16));
#18531=DIRECTION('center_axis',(-1.,0.,0.));
#18532=DIRECTION('ref_axis',(0.,-2.44929359829471E-16,-1.));
#18533=DIRECTION('',(1.,0.,0.));
#18534=DIRECTION('center_axis',(-1.,0.,0.));
#18535=DIRECTION('ref_axis',(0.,1.,-6.12323399573677E-17));
#18536=DIRECTION('',(-1.,0.,0.));
#18537=DIRECTION('center_axis',(-1.,0.,0.));
#18538=DIRECTION('ref_axis',(0.,1.,0.));
#18539=DIRECTION('center_axis',(-1.,0.,0.));
#18540=DIRECTION('ref_axis',(0.,-1.,1.83697019872103E-16));
#18541=DIRECTION('center_axis',(1.,0.,0.));
#18542=DIRECTION('ref_axis',(0.,0.,-1.));
#18543=DIRECTION('center_axis',(-1.,0.,0.));
#18544=DIRECTION('ref_axis',(0.,0.707106781186548,-0.707106781186548));
#18545=DIRECTION('center_axis',(-1.,0.,0.));
#18546=DIRECTION('ref_axis',(0.,1.,0.));
#18547=DIRECTION('',(-1.,0.,0.));
#18548=DIRECTION('center_axis',(1.,0.,0.));
#18549=DIRECTION('ref_axis',(0.,0.,-1.));
#18550=DIRECTION('',(1.,0.,0.));
#18551=DIRECTION('center_axis',(0.,1.,0.));
#18552=DIRECTION('ref_axis',(0.,0.,1.));
#18553=DIRECTION('center_axis',(0.,1.,0.));
#18554=DIRECTION('ref_axis',(-0.707106781186548,0.,0.707106781186548));
#18555=DIRECTION('center_axis',(0.,-1.,0.));
#18556=DIRECTION('ref_axis',(-0.707106781186547,0.,0.707106781186547));
#18557=DIRECTION('center_axis',(1.,0.,0.));
#18558=DIRECTION('ref_axis',(0.,-0.707106781186548,-0.707106781186548));
#18559=DIRECTION('center_axis',(1.,0.,0.));
#18560=DIRECTION('ref_axis',(0.,-1.,0.));
#18561=DIRECTION('',(1.,0.,0.));
#18562=DIRECTION('center_axis',(-1.,0.,0.));
#18563=DIRECTION('ref_axis',(0.,0.,-1.));
#18564=DIRECTION('center_axis',(0.,-1.,0.));
#18565=DIRECTION('ref_axis',(0.,0.,-1.));
#18566=DIRECTION('center_axis',(1.48029736616687E-15,0.,1.));
#18567=DIRECTION('ref_axis',(-1.,0.,1.48029736616687E-15));
#18568=DIRECTION('center_axis',(0.,1.,0.));
#18569=DIRECTION('ref_axis',(0.707106781186548,0.,0.707106781186547));
#18570=DIRECTION('center_axis',(0.,0.,-1.));
#18571=DIRECTION('ref_axis',(-0.707106781186548,-0.707106781186548,0.));
#18572=DIRECTION('center_axis',(0.,-1.,0.));
#18573=DIRECTION('ref_axis',(0.,0.,-1.));
#18574=DIRECTION('center_axis',(0.,1.,0.));
#18575=DIRECTION('ref_axis',(-0.707106781186547,0.,0.707106781186547));
#18576=DIRECTION('center_axis',(1.,0.,0.));
#18577=DIRECTION('ref_axis',(0.,0.,-1.));
#18578=DIRECTION('center_axis',(0.,1.,0.));
#18579=DIRECTION('ref_axis',(0.,0.,1.));
#18580=DIRECTION('center_axis',(1.48029736616687E-15,0.,1.));
#18581=DIRECTION('ref_axis',(0.,1.,0.));
#18582=DIRECTION('center_axis',(0.,-1.,0.));
#18583=DIRECTION('ref_axis',(0.707106781186548,0.,0.707106781186547));
#18584=DIRECTION('center_axis',(0.,1.,0.));
#18585=DIRECTION('ref_axis',(0.707106781186548,0.,0.707106781186547));
#18586=DIRECTION('center_axis',(0.,0.,1.));
#18587=DIRECTION('ref_axis',(-0.707106781186548,0.707106781186548,0.));
#18588=DIRECTION('',(0.,0.,-1.));
#18589=DIRECTION('center_axis',(1.,0.,0.));
#18590=DIRECTION('ref_axis',(0.,0.,-1.));
#18591=DIRECTION('center_axis',(-1.,0.,0.));
#18592=DIRECTION('ref_axis',(0.,0.,1.));
#18593=DIRECTION('',(0.,1.,0.));
#18594=DIRECTION('center_axis',(-1.,0.,0.));
#18595=DIRECTION('ref_axis',(0.,0.,-1.));
#18596=DIRECTION('center_axis',(0.,1.,0.));
#18597=DIRECTION('ref_axis',(-0.707106781186548,0.,0.707106781186547));
#18598=DIRECTION('',(0.,-1.,0.));
#18599=DIRECTION('center_axis',(0.,0.,1.));
#18600=DIRECTION('ref_axis',(1.,0.,0.));
#18601=DIRECTION('',(0.,1.,0.));
#18602=DIRECTION('center_axis',(0.,1.,0.));
#18603=DIRECTION('ref_axis',(0.707106781186546,0.,0.707106781186549));
#18604=DIRECTION('',(0.,0.,-1.));
#18605=DIRECTION('',(0.,0.,-1.));
#18606=DIRECTION('',(0.,0.,-1.));
#18607=DIRECTION('',(0.,0.,-1.));
#18608=DIRECTION('',(0.,0.,-1.));
#18609=DIRECTION('',(0.,0.,-1.));
#18610=DIRECTION('',(0.,0.,-1.));
#18611=DIRECTION('',(0.,0.,-1.));
#18612=DIRECTION('',(0.,0.,-1.));
#18613=DIRECTION('',(0.,0.,-1.));
#18614=DIRECTION('',(0.,0.,-1.));
#18615=DIRECTION('center_axis',(0.,0.,1.));
#18616=DIRECTION('ref_axis',(1.,0.,0.));
#18617=DIRECTION('center_axis',(0.,-1.,0.));
#18618=DIRECTION('ref_axis',(-1.,0.,0.));
#18619=DIRECTION('',(0.,0.,-1.));
#18620=DIRECTION('',(-1.,0.,0.));
#18621=DIRECTION('',(0.,0.,-1.));
#18622=DIRECTION('center_axis',(1.,0.,0.));
#18623=DIRECTION('ref_axis',(0.,-1.,0.));
#18624=DIRECTION('',(0.,0.,-1.));
#18625=DIRECTION('',(0.,-1.,0.));
#18626=DIRECTION('center_axis',(0.,1.,0.));
#18627=DIRECTION('ref_axis',(1.,0.,0.));
#18628=DIRECTION('',(0.,0.,-1.));
#18629=DIRECTION('',(1.,0.,0.));
#18630=DIRECTION('center_axis',(-1.,0.,0.));
#18631=DIRECTION('ref_axis',(0.,1.,0.));
#18632=DIRECTION('',(0.,0.,-1.));
#18633=DIRECTION('',(0.,1.,0.));
#18634=DIRECTION('center_axis',(0.,-1.,0.));
#18635=DIRECTION('ref_axis',(-1.,0.,0.));
#18636=DIRECTION('',(0.,0.,-1.));
#18637=DIRECTION('',(-1.,0.,0.));
#18638=DIRECTION('center_axis',(-1.,0.,0.));
#18639=DIRECTION('ref_axis',(0.,1.,0.));
#18640=DIRECTION('',(0.,0.,-1.));
#18641=DIRECTION('',(0.,1.,0.));
#18642=DIRECTION('center_axis',(0.,-1.,0.));
#18643=DIRECTION('ref_axis',(-1.,0.,0.));
#18644=DIRECTION('',(0.,0.,-1.));
#18645=DIRECTION('',(-1.,0.,0.));
#18646=DIRECTION('center_axis',(1.,0.,0.));
#18647=DIRECTION('ref_axis',(0.,-1.,0.));
#18648=DIRECTION('',(0.,-1.,0.));
#18649=DIRECTION('center_axis',(0.,0.,-1.));
#18650=DIRECTION('ref_axis',(-1.,0.,0.));
#18651=DIRECTION('',(0.,0.,-1.));
#18652=DIRECTION('',(0.,0.,-1.));
#18653=DIRECTION('',(0.,0.,-1.));
#18654=DIRECTION('',(0.,0.,-1.));
#18655=DIRECTION('',(0.,0.,-1.));
#18656=DIRECTION('',(0.,0.,-1.));
#18657=DIRECTION('',(0.,0.,-1.));
#18658=DIRECTION('',(0.,0.,-1.));
#18659=DIRECTION('',(0.,0.,-1.));
#18660=DIRECTION('',(0.,0.,-1.));
#18661=DIRECTION('',(0.,0.,-1.));
#18662=DIRECTION('',(0.,0.,-1.));
#18663=DIRECTION('',(0.,0.,-1.));
#18664=DIRECTION('',(0.,0.,-1.));
#18665=DIRECTION('',(0.,0.,-1.));
#18666=DIRECTION('',(0.,0.,-1.));
#18667=DIRECTION('center_axis',(0.,0.,1.));
#18668=DIRECTION('ref_axis',(1.,0.,0.));
#18669=DIRECTION('center_axis',(-0.831383507294779,-0.555699076657711,0.));
#18670=DIRECTION('ref_axis',(-0.555699076657711,0.831383507294779,0.));
#18671=DIRECTION('',(0.,0.,-1.));
#18672=DIRECTION('',(-0.555699076657711,0.831383507294779,0.));
#18673=DIRECTION('',(0.,0.,-1.));
#18674=DIRECTION('center_axis',(0.,-1.,0.));
#18675=DIRECTION('ref_axis',(-1.,0.,0.));
#18676=DIRECTION('',(0.,0.,-1.));
#18677=DIRECTION('',(-1.,0.,0.));
#18678=DIRECTION('center_axis',(1.,0.,0.));
#18679=DIRECTION('ref_axis',(0.,-1.,0.));
#18680=DIRECTION('',(0.,0.,-1.));
#18681=DIRECTION('',(0.,-1.,0.));
#18682=DIRECTION('center_axis',(0.,1.,0.));
#18683=DIRECTION('ref_axis',(1.,0.,0.));
#18684=DIRECTION('',(0.,0.,-1.));
#18685=DIRECTION('',(1.,0.,0.));
#18686=DIRECTION('center_axis',(-1.,0.,0.));
#18687=DIRECTION('ref_axis',(0.,1.,0.));
#18688=DIRECTION('',(0.,0.,-1.));
#18689=DIRECTION('',(0.,1.,0.));
#18690=DIRECTION('center_axis',(0.831160494084562,0.556032582744129,0.));
#18691=DIRECTION('ref_axis',(0.556032582744129,-0.831160494084562,0.));
#18692=DIRECTION('',(0.,0.,-1.));
#18693=DIRECTION('',(0.556032582744129,-0.831160494084562,0.));
#18694=DIRECTION('center_axis',(0.,1.,0.));
#18695=DIRECTION('ref_axis',(1.,0.,0.));
#18696=DIRECTION('',(0.,0.,-1.));
#18697=DIRECTION('',(1.,0.,0.));
#18698=DIRECTION('center_axis',(-1.,0.,0.));
#18699=DIRECTION('ref_axis',(0.,1.,0.));
#18700=DIRECTION('',(0.,0.,-1.));
#18701=DIRECTION('',(0.,1.,0.));
#18702=DIRECTION('center_axis',(0.,-1.,0.));
#18703=DIRECTION('ref_axis',(-1.,0.,0.));
#18704=DIRECTION('',(0.,0.,-1.));
#18705=DIRECTION('',(-1.,0.,0.));
#18706=DIRECTION('center_axis',(1.,0.,0.));
#18707=DIRECTION('ref_axis',(0.,-1.,0.));
#18708=DIRECTION('',(0.,-1.,0.));
#18709=DIRECTION('center_axis',(0.,0.,-1.));
#18710=DIRECTION('ref_axis',(-1.,0.,0.));
#18711=DIRECTION('center_axis',(-1.,0.,0.));
#18712=DIRECTION('ref_axis',(0.,0.,-1.));
#18713=DIRECTION('',(-1.,0.,0.));
#18714=DIRECTION('center_axis',(-1.,0.,0.));
#18715=DIRECTION('ref_axis',(0.,0.,-1.));
#18716=DIRECTION('center_axis',(1.,0.,0.));
#18717=DIRECTION('ref_axis',(0.,0.,-1.));
#18718=DIRECTION('center_axis',(1.,0.,0.));
#18719=DIRECTION('ref_axis',(0.,1.,0.));
#18720=DIRECTION('center_axis',(1.,0.,0.));
#18721=DIRECTION('ref_axis',(0.,1.,0.));
#18722=DIRECTION('',(0.724999433594412,-0.688749461914695,-8.43474823948293E-17));
#18723=DIRECTION('center_axis',(1.,0.,0.));
#18724=DIRECTION('ref_axis',(0.,1.,0.));
#18725=DIRECTION('',(1.,0.,0.));
#18726=DIRECTION('center_axis',(0.,1.,0.));
#18727=DIRECTION('ref_axis',(0.,0.,1.));
#18728=DIRECTION('center_axis',(1.,0.,0.));
#18729=DIRECTION('ref_axis',(0.,0.,-1.));
#18730=DIRECTION('center_axis',(0.,1.,0.));
#18731=DIRECTION('ref_axis',(0.,0.,1.));
#18732=DIRECTION('axis',(0.,0.,1.));
#18733=DIRECTION('refdir',(1.,0.,0.));
#18734=DIRECTION('center_axis',(1.,0.,0.));
#18735=DIRECTION('ref_axis',(0.,1.,0.));
#18736=DIRECTION('',(-1.,0.,0.));
#18737=DIRECTION('center_axis',(1.,0.,0.));
#18738=DIRECTION('ref_axis',(0.,1.,0.));
#18739=DIRECTION('center_axis',(1.,0.,0.));
#18740=DIRECTION('ref_axis',(0.,1.,0.));
#18741=DIRECTION('',(-1.,0.,0.));
#18742=DIRECTION('center_axis',(1.,0.,0.));
#18743=DIRECTION('ref_axis',(0.,1.,0.));
#18744=DIRECTION('',(-1.,0.,0.));
#18745=DIRECTION('center_axis',(1.,0.,0.));
#18746=DIRECTION('ref_axis',(0.,1.,0.));
#18747=DIRECTION('',(-1.,0.,0.));
#18748=DIRECTION('center_axis',(1.,0.,0.));
#18749=DIRECTION('ref_axis',(0.,1.,0.));
#18750=DIRECTION('',(-1.,0.,0.));
#18751=DIRECTION('center_axis',(1.,0.,0.));
#18752=DIRECTION('ref_axis',(0.,1.,0.));
#18753=DIRECTION('',(-1.,0.,0.));
#18754=DIRECTION('center_axis',(1.,0.,0.));
#18755=DIRECTION('ref_axis',(0.,1.,0.));
#18756=DIRECTION('',(-1.,0.,0.));
#18757=DIRECTION('center_axis',(1.,0.,0.));
#18758=DIRECTION('ref_axis',(0.,1.,0.));
#18759=DIRECTION('',(-1.,0.,0.));
#18760=DIRECTION('center_axis',(1.,0.,0.));
#18761=DIRECTION('ref_axis',(0.,1.,0.));
#18762=DIRECTION('',(-1.,0.,0.));
#18763=DIRECTION('center_axis',(1.,0.,0.));
#18764=DIRECTION('ref_axis',(0.,1.,0.));
#18765=DIRECTION('',(-1.,0.,0.));
#18766=DIRECTION('center_axis',(1.,0.,0.));
#18767=DIRECTION('ref_axis',(0.,1.,0.));
#18768=DIRECTION('',(-1.,0.,0.));
#18769=DIRECTION('center_axis',(1.,0.,0.));
#18770=DIRECTION('ref_axis',(0.,1.,0.));
#18771=DIRECTION('',(-1.,0.,0.));
#18772=DIRECTION('center_axis',(1.,0.,0.));
#18773=DIRECTION('ref_axis',(0.,1.,0.));
#18774=DIRECTION('',(-1.,0.,0.));
#18775=DIRECTION('center_axis',(1.,0.,0.));
#18776=DIRECTION('ref_axis',(0.,1.,0.));
#18777=DIRECTION('',(-1.,0.,0.));
#18778=DIRECTION('center_axis',(1.,0.,0.));
#18779=DIRECTION('ref_axis',(0.,1.,0.));
#18780=DIRECTION('',(-1.,0.,0.));
#18781=DIRECTION('center_axis',(1.,0.,0.));
#18782=DIRECTION('ref_axis',(0.,1.,0.));
#18783=DIRECTION('',(-1.,0.,0.));
#18784=DIRECTION('center_axis',(1.,0.,0.));
#18785=DIRECTION('ref_axis',(0.,1.,7.24992115782204E-14));
#18786=DIRECTION('',(1.,0.,0.));
#18787=DIRECTION('center_axis',(1.,0.,0.));
#18788=DIRECTION('ref_axis',(0.,1.,7.24992115782204E-14));
#18789=DIRECTION('center_axis',(1.,0.,0.));
#18790=DIRECTION('ref_axis',(0.,1.,7.24992115782204E-14));
#18791=DIRECTION('',(1.,0.,0.));
#18792=DIRECTION('center_axis',(1.,0.,0.));
#18793=DIRECTION('ref_axis',(0.,1.,7.24992115782204E-14));
#18794=DIRECTION('',(1.,0.,0.));
#18795=DIRECTION('center_axis',(1.,0.,0.));
#18796=DIRECTION('ref_axis',(0.,1.,7.24992115782204E-14));
#18797=DIRECTION('',(1.,0.,0.));
#18798=DIRECTION('center_axis',(1.,0.,0.));
#18799=DIRECTION('ref_axis',(0.,1.,7.24992115782204E-14));
#18800=DIRECTION('',(1.,0.,0.));
#18801=DIRECTION('center_axis',(1.,0.,0.));
#18802=DIRECTION('ref_axis',(0.,1.,7.24992115782204E-14));
#18803=DIRECTION('',(1.,0.,0.));
#18804=DIRECTION('center_axis',(1.,0.,0.));
#18805=DIRECTION('ref_axis',(0.,1.,7.24992115782204E-14));
#18806=DIRECTION('',(1.,0.,0.));
#18807=DIRECTION('center_axis',(1.,0.,0.));
#18808=DIRECTION('ref_axis',(0.,1.,7.24992115782204E-14));
#18809=DIRECTION('',(1.,0.,0.));
#18810=DIRECTION('center_axis',(1.,0.,0.));
#18811=DIRECTION('ref_axis',(0.,1.,7.24992115782204E-14));
#18812=DIRECTION('',(1.,0.,0.));
#18813=DIRECTION('center_axis',(1.,0.,0.));
#18814=DIRECTION('ref_axis',(0.,1.,7.24992115782204E-14));
#18815=DIRECTION('',(1.,0.,0.));
#18816=DIRECTION('center_axis',(1.,0.,0.));
#18817=DIRECTION('ref_axis',(0.,1.,7.24992115782204E-14));
#18818=DIRECTION('',(1.,0.,0.));
#18819=DIRECTION('center_axis',(1.,0.,0.));
#18820=DIRECTION('ref_axis',(0.,1.,7.24992115782204E-14));
#18821=DIRECTION('',(1.,0.,0.));
#18822=DIRECTION('center_axis',(1.,0.,0.));
#18823=DIRECTION('ref_axis',(0.,1.,7.24992115782204E-14));
#18824=DIRECTION('',(1.,0.,0.));
#18825=DIRECTION('center_axis',(1.,0.,0.));
#18826=DIRECTION('ref_axis',(0.,1.,7.24992115782204E-14));
#18827=DIRECTION('',(1.,0.,0.));
#18828=DIRECTION('center_axis',(1.,0.,0.));
#18829=DIRECTION('ref_axis',(0.,1.,7.24992115782204E-14));
#18830=DIRECTION('',(1.,0.,0.));
#18831=DIRECTION('center_axis',(1.,0.,0.));
#18832=DIRECTION('ref_axis',(0.,1.,0.));
#18833=DIRECTION('',(-1.,0.,0.));
#18834=DIRECTION('center_axis',(-1.,0.,0.));
#18835=DIRECTION('ref_axis',(0.,1.,0.));
#18836=DIRECTION('center_axis',(1.,0.,0.));
#18837=DIRECTION('ref_axis',(0.,1.,0.));
#18838=DIRECTION('',(-1.,0.,0.));
#18839=DIRECTION('center_axis',(1.,0.,0.));
#18840=DIRECTION('ref_axis',(0.,1.,0.));
#18841=DIRECTION('',(-1.,0.,0.));
#18842=DIRECTION('center_axis',(1.,0.,0.));
#18843=DIRECTION('ref_axis',(0.,1.,0.));
#18844=DIRECTION('',(-1.,0.,0.));
#18845=DIRECTION('center_axis',(1.,0.,0.));
#18846=DIRECTION('ref_axis',(0.,1.,0.));
#18847=DIRECTION('',(-1.,0.,0.));
#18848=DIRECTION('center_axis',(1.,0.,0.));
#18849=DIRECTION('ref_axis',(0.,1.,0.));
#18850=DIRECTION('',(-1.,0.,0.));
#18851=DIRECTION('center_axis',(1.,0.,0.));
#18852=DIRECTION('ref_axis',(0.,1.,0.));
#18853=DIRECTION('',(-1.,0.,0.));
#18854=DIRECTION('center_axis',(1.,0.,0.));
#18855=DIRECTION('ref_axis',(0.,1.,0.));
#18856=DIRECTION('',(-1.,0.,0.));
#18857=DIRECTION('center_axis',(1.,0.,0.));
#18858=DIRECTION('ref_axis',(0.,1.,0.));
#18859=DIRECTION('',(-1.,0.,0.));
#18860=DIRECTION('center_axis',(1.,0.,0.));
#18861=DIRECTION('ref_axis',(0.,1.,0.));
#18862=DIRECTION('',(-1.,0.,0.));
#18863=DIRECTION('center_axis',(1.,0.,0.));
#18864=DIRECTION('ref_axis',(0.,1.,0.));
#18865=DIRECTION('',(-1.,0.,0.));
#18866=DIRECTION('center_axis',(-1.,0.,0.));
#18867=DIRECTION('ref_axis',(0.,1.,0.));
#18868=DIRECTION('center_axis',(1.,0.,0.));
#18869=DIRECTION('ref_axis',(0.,0.100102849209394,-0.994977095002775));
#18870=DIRECTION('',(1.,0.,0.));
#18871=DIRECTION('center_axis',(1.,0.,0.));
#18872=DIRECTION('ref_axis',(0.,1.,4.89925865752541E-14));
#18873=DIRECTION('center_axis',(1.,0.,0.));
#18874=DIRECTION('ref_axis',(0.,1.,4.89925865752541E-14));
#18875=DIRECTION('',(1.,0.,0.));
#18876=DIRECTION('center_axis',(1.,0.,0.));
#18877=DIRECTION('ref_axis',(0.,1.,4.89925865752541E-14));
#18878=DIRECTION('',(1.,0.,0.));
#18879=DIRECTION('center_axis',(1.,0.,0.));
#18880=DIRECTION('ref_axis',(0.,1.,4.89925865752541E-14));
#18881=DIRECTION('',(1.,0.,0.));
#18882=DIRECTION('center_axis',(1.,0.,0.));
#18883=DIRECTION('ref_axis',(0.,1.,4.89925865752541E-14));
#18884=DIRECTION('',(1.,0.,0.));
#18885=DIRECTION('center_axis',(1.,0.,0.));
#18886=DIRECTION('ref_axis',(0.,1.,4.89925865752541E-14));
#18887=DIRECTION('',(1.,0.,0.));
#18888=DIRECTION('center_axis',(1.,0.,0.));
#18889=DIRECTION('ref_axis',(0.,1.,4.89925865752541E-14));
#18890=DIRECTION('',(1.,0.,0.));
#18891=DIRECTION('center_axis',(1.,0.,0.));
#18892=DIRECTION('ref_axis',(0.,1.,4.89925865752541E-14));
#18893=DIRECTION('',(1.,0.,0.));
#18894=DIRECTION('center_axis',(1.,0.,0.));
#18895=DIRECTION('ref_axis',(0.,1.,4.89925865752541E-14));
#18896=DIRECTION('',(1.,0.,0.));
#18897=DIRECTION('center_axis',(1.,0.,0.));
#18898=DIRECTION('ref_axis',(0.,1.,4.89925865752541E-14));
#18899=DIRECTION('',(1.,0.,0.));
#18900=DIRECTION('center_axis',(-1.,0.,0.));
#18901=DIRECTION('ref_axis',(0.,-1.,0.));
#18902=DIRECTION('center_axis',(-1.,0.,0.));
#18903=DIRECTION('ref_axis',(0.,-1.,0.));
#18904=DIRECTION('',(0.707106781186553,-0.707106781186542,8.65956056235487E-17));
#18905=DIRECTION('center_axis',(1.,0.,0.));
#18906=DIRECTION('ref_axis',(0.,-1.,0.));
#18907=DIRECTION('center_axis',(1.,0.,0.));
#18908=DIRECTION('ref_axis',(0.,-1.,0.));
#18909=DIRECTION('center_axis',(1.,0.,0.));
#18910=DIRECTION('ref_axis',(0.,1.,0.));
#18911=DIRECTION('center_axis',(-1.,0.,0.));
#18912=DIRECTION('ref_axis',(0.,-1.,0.));
#18913=DIRECTION('center_axis',(-1.,0.,0.));
#18914=DIRECTION('ref_axis',(0.,-1.,0.));
#18915=DIRECTION('',(-1.,0.,0.));
#18916=DIRECTION('center_axis',(-1.,0.,0.));
#18917=DIRECTION('ref_axis',(0.,0.,1.));
#18918=DIRECTION('center_axis',(1.,0.,0.));
#18919=DIRECTION('ref_axis',(0.,0.,-1.));
#18920=DIRECTION('center_axis',(1.,0.,0.));
#18921=DIRECTION('ref_axis',(0.,-1.,0.));
#18922=DIRECTION('',(0.707106781186553,0.707106781186542,-8.65956056235487E-17));
#18923=DIRECTION('center_axis',(1.,0.,0.));
#18924=DIRECTION('ref_axis',(0.,-1.,0.));
#18925=DIRECTION('center_axis',(1.,0.,0.));
#18926=DIRECTION('ref_axis',(0.,0.,-1.));
#18927=DIRECTION('center_axis',(1.,0.,0.));
#18928=DIRECTION('ref_axis',(0.,0.,-1.));
#18929=DIRECTION('center_axis',(-1.,0.,-4.39101262113484E-15));
#18930=DIRECTION('ref_axis',(0.,-1.,-3.11403559978336E-17));
#18931=DIRECTION('center_axis',(-1.,0.,0.));
#18932=DIRECTION('ref_axis',(0.,-1.,0.));
#18933=DIRECTION('',(-0.382683432365094,0.923879532511285,-1.53845523264404E-15));
#18934=DIRECTION('center_axis',(1.,0.,0.));
#18935=DIRECTION('ref_axis',(0.,-1.,-6.12323399573677E-17));
#18936=DIRECTION('center_axis',(1.,0.,0.));
#18937=DIRECTION('ref_axis',(0.,-1.,-6.12323399573677E-17));
#18938=DIRECTION('center_axis',(-1.,0.,0.));
#18939=DIRECTION('ref_axis',(0.,1.,0.));
#18940=DIRECTION('',(-0.707106781186546,-0.707106781186549,-8.65956056235495E-17));
#18941=DIRECTION('center_axis',(1.,0.,0.));
#18942=DIRECTION('ref_axis',(0.,0.,-1.));
#18943=DIRECTION('center_axis',(1.,0.,0.));
#18944=DIRECTION('ref_axis',(0.,0.,-1.));
#18945=DIRECTION('center_axis',(-1.,0.,0.));
#18946=DIRECTION('ref_axis',(0.,1.,4.89925865752541E-14));
#18947=DIRECTION('center_axis',(0.,6.92018220157551E-16,-1.));
#18948=DIRECTION('ref_axis',(1.,3.00652077147108E-17,0.));
#18949=DIRECTION('center_axis',(-5.63785247977654E-32,9.20731182852366E-16,
-1.));
#18950=DIRECTION('ref_axis',(1.,6.12323399573677E-17,0.));
#18951=DIRECTION('',(-0.382683432365095,5.80970808792151E-16,-0.923879532511284));
#18952=DIRECTION('center_axis',(0.,0.,1.));
#18953=DIRECTION('ref_axis',(1.,0.,0.));
#18954=DIRECTION('center_axis',(0.,0.,-1.));
#18955=DIRECTION('ref_axis',(1.,0.,0.));
#18956=DIRECTION('center_axis',(-2.84633584564593E-32,4.64841919748234E-16,
1.));
#18957=DIRECTION('ref_axis',(1.,6.12323399573677E-17,0.));
#18958=DIRECTION('',(-0.707106781186547,-8.65956056235493E-17,-0.707106781186547));
#18959=DIRECTION('center_axis',(0.,-1.65459148343064E-15,-1.));
#18960=DIRECTION('ref_axis',(1.,3.20478109930714E-17,0.));
#18961=DIRECTION('',(0.923879532511284,5.49650453450813E-16,0.382683432365097));
#18962=DIRECTION('center_axis',(0.,0.,-1.));
#18963=DIRECTION('ref_axis',(1.,0.,0.));
#18964=DIRECTION('center_axis',(0.,0.,1.));
#18965=DIRECTION('ref_axis',(1.,0.,0.));
#18966=DIRECTION('center_axis',(0.,0.,1.));
#18967=DIRECTION('ref_axis',(1.,0.,0.));
#18968=DIRECTION('center_axis',(1.,0.,0.));
#18969=DIRECTION('ref_axis',(0.,0.,-1.));
#18970=DIRECTION('center_axis',(-1.,0.,0.));
#18971=DIRECTION('ref_axis',(0.,1.,0.));
#18972=DIRECTION('center_axis',(1.,0.,0.));
#18973=DIRECTION('ref_axis',(0.,1.,4.89925865752541E-14));
#18974=DIRECTION('center_axis',(1.,0.,0.));
#18975=DIRECTION('ref_axis',(0.,1.,0.));
#18976=DIRECTION('center_axis',(-1.,0.,0.));
#18977=DIRECTION('ref_axis',(0.,1.,0.));
#18978=DIRECTION('center_axis',(1.,0.,0.));
#18979=DIRECTION('ref_axis',(0.,0.,-1.));
#18980=DIRECTION('center_axis',(1.,0.,0.));
#18981=DIRECTION('ref_axis',(0.,1.,0.));
#18982=DIRECTION('center_axis',(1.,0.,0.));
#18983=DIRECTION('ref_axis',(0.,1.,0.));
#18984=DIRECTION('center_axis',(-1.,0.,0.));
#18985=DIRECTION('ref_axis',(0.,1.,7.24992115782204E-14));
#18986=DIRECTION('center_axis',(1.,0.,0.));
#18987=DIRECTION('ref_axis',(0.,0.888973712533679,0.45795822781569));
#18988=DIRECTION('center_axis',(0.,0.,1.));
#18989=DIRECTION('ref_axis',(-0.707106781186561,0.707106781186534,0.));
#18990=DIRECTION('',(0.,0.,-1.));
#18991=DIRECTION('',(0.,0.,1.));
#18992=DIRECTION('center_axis',(0.,1.,0.));
#18993=DIRECTION('ref_axis',(-1.,0.,6.34413156928661E-16));
#18994=DIRECTION('',(0.,1.,0.));
#18995=DIRECTION('center_axis',(0.,1.,0.));
#18996=DIRECTION('ref_axis',(-1.,0.,6.34413156928661E-16));
#18997=DIRECTION('center_axis',(0.,1.,0.));
#18998=DIRECTION('ref_axis',(-1.,0.,6.34413156928661E-16));
#18999=DIRECTION('center_axis',(-1.,0.,0.));
#19000=DIRECTION('ref_axis',(0.,0.,1.));
#19001=DIRECTION('center_axis',(-1.,0.,0.));
#19002=DIRECTION('ref_axis',(0.,1.,0.));
#19003=DIRECTION('',(0.,0.,-1.));
#19004=DIRECTION('center_axis',(0.,0.,-1.));
#19005=DIRECTION('ref_axis',(-0.707106781186561,-0.707106781186534,0.));
#19006=DIRECTION('',(0.,0.,1.));
#19007=DIRECTION('center_axis',(0.,0.,1.));
#19008=DIRECTION('ref_axis',(0.995170161956952,0.0981649059011095,0.));
#19009=DIRECTION('',(0.,0.,1.));
#19010=DIRECTION('',(0.,0.,-1.));
#19011=DIRECTION('center_axis',(0.,0.,-1.));
#19012=DIRECTION('ref_axis',(0.995170161956952,-0.0981649059011095,0.));
#19013=DIRECTION('',(0.,0.,-1.));
#19014=DIRECTION('',(0.,0.,1.));
#19015=DIRECTION('center_axis',(0.,-1.,0.));
#19016=DIRECTION('ref_axis',(1.,0.,0.));
#19017=DIRECTION('center_axis',(0.,-1.,0.));
#19018=DIRECTION('ref_axis',(1.,0.,0.));
#19019=DIRECTION('',(0.70710678118654,0.707106781186555,8.65956056235484E-17));
#19020=DIRECTION('center_axis',(0.,1.,0.));
#19021=DIRECTION('ref_axis',(1.,0.,0.));
#19022=DIRECTION('center_axis',(0.,1.,0.));
#19023=DIRECTION('ref_axis',(1.,0.,0.));
#19024=DIRECTION('center_axis',(0.,1.,0.));
#19025=DIRECTION('ref_axis',(1.,0.,0.));
#19026=DIRECTION('center_axis',(0.,1.,0.));
#19027=DIRECTION('ref_axis',(1.,0.,0.));
#19028=DIRECTION('',(0.,1.,0.));
#19029=DIRECTION('center_axis',(0.,1.,0.));
#19030=DIRECTION('ref_axis',(1.,0.,0.));
#19031=DIRECTION('center_axis',(0.,0.,1.));
#19032=DIRECTION('ref_axis',(1.,0.,0.));
#19033=DIRECTION('',(0.70710678118654,8.65956056235484E-17,-0.707106781186555));
#19034=DIRECTION('center_axis',(0.,0.,-1.));
#19035=DIRECTION('ref_axis',(1.,0.,0.));
#19036=DIRECTION('center_axis',(0.,0.,-1.));
#19037=DIRECTION('ref_axis',(1.,0.,0.));
#19038=DIRECTION('',(0.,0.,-1.));
#19039=DIRECTION('center_axis',(0.,0.,-1.));
#19040=DIRECTION('ref_axis',(1.,0.,0.));
#19041=DIRECTION('center_axis',(0.,1.,0.));
#19042=DIRECTION('ref_axis',(1.,0.,0.));
#19043=DIRECTION('',(-0.707106781186548,0.707106781186548,-8.65956056235493E-17));
#19044=DIRECTION('center_axis',(0.,-1.,0.));
#19045=DIRECTION('ref_axis',(1.,0.,0.));
#19046=DIRECTION('center_axis',(0.,-1.,0.));
#19047=DIRECTION('ref_axis',(1.,0.,0.));
#19048=DIRECTION('',(0.,1.,0.));
#19049=DIRECTION('center_axis',(0.,0.,1.));
#19050=DIRECTION('ref_axis',(1.,0.,0.));
#19051=DIRECTION('center_axis',(0.,1.,0.));
#19052=DIRECTION('ref_axis',(1.,0.,0.));
#19053=DIRECTION('center_axis',(0.,0.,1.));
#19054=DIRECTION('ref_axis',(1.,0.,0.));
#19055=DIRECTION('center_axis',(0.,1.,0.));
#19056=DIRECTION('ref_axis',(1.,0.,0.));
#19057=DIRECTION('center_axis',(0.,1.,0.));
#19058=DIRECTION('ref_axis',(1.,0.,0.));
#19059=DIRECTION('',(0.,1.,0.));
#19060=DIRECTION('center_axis',(0.,-1.,0.));
#19061=DIRECTION('ref_axis',(1.,0.,0.));
#19062=DIRECTION('center_axis',(1.,0.,0.));
#19063=DIRECTION('ref_axis',(0.,1.,0.));
#19064=DIRECTION('',(-1.,0.,0.));
#19065=DIRECTION('center_axis',(1.,0.,0.));
#19066=DIRECTION('ref_axis',(0.,0.,-1.));
#19067=DIRECTION('',(-1.,0.,0.));
#19068=DIRECTION('',(1.,0.,0.));
#19069=DIRECTION('center_axis',(0.,1.,0.));
#19070=DIRECTION('ref_axis',(1.,0.,0.));
#19071=DIRECTION('center_axis',(0.,1.,0.));
#19072=DIRECTION('ref_axis',(1.,0.,0.));
#19073=DIRECTION('center_axis',(1.,0.,0.));
#19074=DIRECTION('ref_axis',(0.,1.,0.));
#19075=DIRECTION('',(-1.,0.,0.));
#19076=DIRECTION('center_axis',(1.,0.,0.));
#19077=DIRECTION('ref_axis',(0.,0.,-1.));
#19078=DIRECTION('center_axis',(-1.,0.,0.));
#19079=DIRECTION('ref_axis',(0.,0.,1.));
#19080=DIRECTION('center_axis',(1.,0.,0.));
#19081=DIRECTION('ref_axis',(0.,0.,-1.));
#19082=DIRECTION('center_axis',(1.,0.,0.));
#19083=DIRECTION('ref_axis',(0.,1.,0.));
#19084=DIRECTION('',(-0.707106781186548,0.707106781186548,8.65956056235493E-17));
#19085=DIRECTION('center_axis',(1.,0.,0.));
#19086=DIRECTION('ref_axis',(0.,-0.488782589557792,-0.872405628217276));
#19087=DIRECTION('center_axis',(1.,0.,0.));
#19088=DIRECTION('ref_axis',(0.,1.,0.));
#19089=DIRECTION('center_axis',(-1.,0.,0.));
#19090=DIRECTION('ref_axis',(0.,0.,1.));
#19091=DIRECTION('center_axis',(1.,0.,0.));
#19092=DIRECTION('ref_axis',(0.,0.,-1.));
#19093=DIRECTION('center_axis',(1.,0.,0.));
#19094=DIRECTION('ref_axis',(0.,1.,0.));
#19095=DIRECTION('',(-0.707106781186552,0.707106781186543,8.65956056235488E-17));
#19096=DIRECTION('center_axis',(-1.,0.,0.));
#19097=DIRECTION('ref_axis',(0.,1.,0.));
#19098=DIRECTION('',(-0.707106781186555,-0.70710678118654,-8.65956056235484E-17));
#19099=DIRECTION('axis',(0.,0.,1.));
#19100=DIRECTION('refdir',(1.,0.,0.));
#19101=DIRECTION('center_axis',(1.,0.,0.));
#19102=DIRECTION('ref_axis',(0.,0.,-1.));
#19103=DIRECTION('center_axis',(1.,0.,0.));
#19104=DIRECTION('ref_axis',(0.,0.,-1.));
#19105=DIRECTION('',(1.,0.,0.));
#19106=DIRECTION('center_axis',(1.,0.,0.));
#19107=DIRECTION('ref_axis',(0.,0.,-1.));
#19108=DIRECTION('center_axis',(1.,0.,0.));
#19109=DIRECTION('ref_axis',(0.,0.,-1.));
#19110=DIRECTION('center_axis',(-1.,0.,0.));
#19111=DIRECTION('ref_axis',(0.,0.,1.));
#19112=DIRECTION('center_axis',(1.,0.,0.));
#19113=DIRECTION('ref_axis',(0.,0.,-1.));
#19114=DIRECTION('center_axis',(1.,0.,0.));
#19115=DIRECTION('ref_axis',(0.,1.,0.));
#19116=DIRECTION('center_axis',(1.,0.,0.));
#19117=DIRECTION('ref_axis',(0.,0.,-1.));
#19118=DIRECTION('',(-0.707106781186544,0.707106781186551,8.65956056235498E-17));
#19119=DIRECTION('center_axis',(1.,0.,0.));
#19120=DIRECTION('ref_axis',(0.,1.,0.));
#19121=DIRECTION('center_axis',(1.,0.,0.));
#19122=DIRECTION('ref_axis',(0.,0.,-1.));
#19123=DIRECTION('',(-1.,0.,0.));
#19124=DIRECTION('center_axis',(-1.,0.,0.));
#19125=DIRECTION('ref_axis',(0.,0.,1.));
#19126=DIRECTION('center_axis',(1.,0.,0.));
#19127=DIRECTION('ref_axis',(0.,0.,-1.));
#19128=DIRECTION('center_axis',(1.,0.,0.));
#19129=DIRECTION('ref_axis',(0.,1.,0.));
#19130=DIRECTION('center_axis',(1.,0.,0.));
#19131=DIRECTION('ref_axis',(0.,0.,-1.));
#19132=DIRECTION('',(-0.707106781186552,0.707106781186543,8.65956056235487E-17));
#19133=DIRECTION('center_axis',(1.,0.,0.));
#19134=DIRECTION('ref_axis',(0.,1.,0.));
#19135=DIRECTION('center_axis',(1.,0.,0.));
#19136=DIRECTION('ref_axis',(0.,0.,-1.));
#19137=DIRECTION('',(-1.,0.,0.));
#19138=DIRECTION('center_axis',(1.,0.,0.));
#19139=DIRECTION('ref_axis',(0.,0.,-1.));
#19140=DIRECTION('center_axis',(1.,0.,0.));
#19141=DIRECTION('ref_axis',(0.,0.,-1.));
#19142=DIRECTION('center_axis',(1.,0.,0.));
#19143=DIRECTION('ref_axis',(0.,1.,0.));
#19144=DIRECTION('center_axis',(1.,0.,0.));
#19145=DIRECTION('ref_axis',(0.,0.,-1.));
#19146=DIRECTION('',(-1.,0.,0.));
#19147=DIRECTION('center_axis',(-1.,0.,0.));
#19148=DIRECTION('ref_axis',(0.,0.,1.));
#19149=DIRECTION('center_axis',(1.,0.,0.));
#19150=DIRECTION('ref_axis',(0.,0.,-1.));
#19151=DIRECTION('center_axis',(1.,0.,0.));
#19152=DIRECTION('ref_axis',(0.,1.,0.));
#19153=DIRECTION('center_axis',(1.,0.,0.));
#19154=DIRECTION('ref_axis',(0.,0.,-1.));
#19155=DIRECTION('',(-1.,0.,0.));
#19156=DIRECTION('center_axis',(1.,0.,0.));
#19157=DIRECTION('ref_axis',(0.,0.,-1.));
#19158=DIRECTION('center_axis',(1.,0.,0.));
#19159=DIRECTION('ref_axis',(0.,0.,-1.));
#19160=DIRECTION('center_axis',(1.,0.,0.));
#19161=DIRECTION('ref_axis',(0.,1.,0.));
#19162=DIRECTION('center_axis',(1.,0.,0.));
#19163=DIRECTION('ref_axis',(0.,0.,-1.));
#19164=DIRECTION('',(-1.,0.,0.));
#19165=DIRECTION('center_axis',(-1.,0.,0.));
#19166=DIRECTION('ref_axis',(0.,0.,1.));
#19167=DIRECTION('center_axis',(1.,0.,0.));
#19168=DIRECTION('ref_axis',(0.,0.,-1.));
#19169=DIRECTION('center_axis',(1.,0.,0.));
#19170=DIRECTION('ref_axis',(0.,1.,0.));
#19171=DIRECTION('center_axis',(1.,0.,0.));
#19172=DIRECTION('ref_axis',(0.,0.,-1.));
#19173=DIRECTION('',(-1.,0.,0.));
#19174=DIRECTION('center_axis',(-1.,0.,0.));
#19175=DIRECTION('ref_axis',(0.,1.,0.));
#19176=DIRECTION('center_axis',(1.,0.,0.));
#19177=DIRECTION('ref_axis',(0.,0.,-1.));
#19178=DIRECTION('',(-0.70710678118654,-0.707106781186555,-8.65956056235503E-17));
#19179=DIRECTION('center_axis',(1.,0.,0.));
#19180=DIRECTION('ref_axis',(0.,0.,-1.));
#19181=DIRECTION('axis',(0.,0.,1.));
#19182=DIRECTION('refdir',(1.,0.,0.));
#19183=DIRECTION('center_axis',(0.0385833407296796,-0.00185275719821836,
0.99925366804876));
#19184=DIRECTION('ref_axis',(-0.998103575378143,0.0479285502208167,0.0386277994596909));
#19185=DIRECTION('center_axis',(0.0385833409756958,0.0018527571775933,0.999253668039299));
#19186=DIRECTION('ref_axis',(-0.285673463027164,0.95828233937443,0.00925367846524069));
#19187=DIRECTION('center_axis',(0.0385833409756958,0.0018527571775933,0.999253668039299));
#19188=DIRECTION('ref_axis',(-0.285673463027164,0.95828233937443,0.00925367846524068));
#19189=DIRECTION('center_axis',(0.0385833407296796,-0.00185275719821836,
0.99925366804876));
#19190=DIRECTION('ref_axis',(-0.998103575378143,0.0479285502208167,0.0386277994596909));
#19191=DIRECTION('axis',(0.,0.,1.));
#19192=DIRECTION('refdir',(1.,0.,0.));
#19193=DIRECTION('center_axis',(1.,0.,0.));
#19194=DIRECTION('ref_axis',(0.,0.,-1.));
#19195=DIRECTION('center_axis',(0.,-1.,-1.22464679914735E-16));
#19196=DIRECTION('ref_axis',(0.,-1.22464679914735E-16,1.));
#19197=DIRECTION('center_axis',(-1.,0.,0.));
#19198=DIRECTION('ref_axis',(0.,0.,-1.));
#19199=DIRECTION('axis',(0.,0.,1.));
#19200=DIRECTION('refdir',(1.,0.,0.));
#19201=DIRECTION('center_axis',(1.,0.,0.));
#19202=DIRECTION('ref_axis',(0.,1.,0.));
#19203=DIRECTION('center_axis',(1.,0.,0.));
#19204=DIRECTION('ref_axis',(0.,0.,-1.));
#19205=DIRECTION('',(-1.,0.,0.));
#19206=DIRECTION('center_axis',(1.,0.,0.));
#19207=DIRECTION('ref_axis',(0.,0.,-1.));
#19208=DIRECTION('center_axis',(-1.,0.,0.));
#19209=DIRECTION('ref_axis',(0.,0.,1.));
#19210=DIRECTION('center_axis',(1.,0.,0.));
#19211=DIRECTION('ref_axis',(0.,0.,-1.));
#19212=DIRECTION('center_axis',(1.,0.,0.));
#19213=DIRECTION('ref_axis',(0.,1.,0.));
#19214=DIRECTION('center_axis',(1.,0.,0.));
#19215=DIRECTION('ref_axis',(0.,0.,-1.));
#19216=DIRECTION('',(-1.,0.,0.));
#19217=DIRECTION('center_axis',(1.,0.,0.));
#19218=DIRECTION('ref_axis',(0.,0.,-1.));
#19219=DIRECTION('axis',(0.,0.,1.));
#19220=DIRECTION('refdir',(1.,0.,0.));
#19221=DIRECTION('center_axis',(-1.,0.,0.));
#19222=DIRECTION('ref_axis',(0.,0.,1.));
#19223=DIRECTION('center_axis',(1.,0.,0.));
#19224=DIRECTION('ref_axis',(0.,0.,-1.));
#19225=DIRECTION('center_axis',(1.,0.,0.));
#19226=DIRECTION('ref_axis',(0.,1.,0.));
#19227=DIRECTION('center_axis',(1.,0.,0.));
#19228=DIRECTION('ref_axis',(0.,0.,-1.));
#19229=DIRECTION('',(-0.707106781186547,0.707106781186548,8.65956056235494E-17));
#19230=DIRECTION('center_axis',(1.,0.,0.));
#19231=DIRECTION('ref_axis',(0.,1.,0.));
#19232=DIRECTION('center_axis',(1.,0.,0.));
#19233=DIRECTION('ref_axis',(0.,0.,-1.));
#19234=DIRECTION('',(-1.,0.,0.));
#19235=DIRECTION('center_axis',(-1.,0.,0.));
#19236=DIRECTION('ref_axis',(0.,1.,0.));
#19237=DIRECTION('center_axis',(1.,0.,0.));
#19238=DIRECTION('ref_axis',(0.,0.,-1.));
#19239=DIRECTION('',(-0.707106781186548,-0.707106781186548,-8.65956056235493E-17));
#19240=DIRECTION('center_axis',(1.,0.,0.));
#19241=DIRECTION('ref_axis',(0.,0.,-1.));
#19242=DIRECTION('axis',(0.,0.,1.));
#19243=DIRECTION('refdir',(1.,0.,0.));
#19244=DIRECTION('center_axis',(-0.923879532511287,0.,0.38268343236509));
#19245=DIRECTION('ref_axis',(0.38268343236509,0.,0.923879532511287));
#19246=DIRECTION('',(0.357406744336594,-0.357406744336592,0.862856209461017));
#19247=DIRECTION('',(0.,1.,0.));
#19248=DIRECTION('',(-0.357406744336594,-0.357406744336592,-0.862856209461017));
#19249=DIRECTION('',(0.,-1.,0.));
#19250=DIRECTION('center_axis',(-0.707106781186546,-0.707106781186549,0.));
#19251=DIRECTION('ref_axis',(0.,0.,1.));
#19252=DIRECTION('',(0.,0.,-1.));
#19253=DIRECTION('',(-0.357406744336591,0.357406744336589,0.86285620946102));
#19254=DIRECTION('',(0.577350269189627,-0.577350269189624,-0.577350269189627));
#19255=DIRECTION('',(0.,0.,1.));
#19256=DIRECTION('',(-0.577350269189627,0.577350269189624,-0.577350269189627));
#19257=DIRECTION('center_axis',(-1.,0.,0.));
#19258=DIRECTION('ref_axis',(0.,0.,1.));
#19259=DIRECTION('',(0.,0.,1.));
#19260=DIRECTION('',(0.,1.,0.));
#19261=DIRECTION('center_axis',(-0.382683432365086,0.,0.923879532511288));
#19262=DIRECTION('ref_axis',(0.923879532511288,0.,0.382683432365086));
#19263=DIRECTION('',(-0.86285620946102,0.357406744336589,-0.357406744336591));
#19264=DIRECTION('',(0.,-1.,0.));
#19265=DIRECTION('',(0.86285620946102,0.357406744336589,0.357406744336591));
#19266=DIRECTION('',(0.,1.,0.));
#19267=DIRECTION('center_axis',(0.,0.,1.));
#19268=DIRECTION('ref_axis',(1.,0.,0.));
#19269=DIRECTION('',(-1.,0.,0.));
#19270=DIRECTION('',(0.,-1.,0.));
#19271=DIRECTION('',(1.,0.,0.));
#19272=DIRECTION('center_axis',(0.,-0.707106781186549,0.707106781186546));
#19273=DIRECTION('ref_axis',(1.,0.,0.));
#19274=DIRECTION('',(-0.577350269189627,-0.577350269189624,-0.577350269189627));
#19275=DIRECTION('',(1.,0.,0.));
#19276=DIRECTION('',(-0.577350269189627,0.577350269189624,0.577350269189627));
#19277=DIRECTION('',(0.862856209461016,-0.357406744336594,-0.357406744336595));
#19278=DIRECTION('center_axis',(0.86602540378444,0.,0.499999999999998));
#19279=DIRECTION('ref_axis',(0.499999999999998,0.,-0.86602540378444));
#19280=DIRECTION('',(0.447213595499956,0.447213595499956,-0.774596669241485));
#19281=DIRECTION('',(0.,1.,0.));
#19282=DIRECTION('',(-0.447213595499956,0.447213595499956,0.774596669241485));
#19283=DIRECTION('',(-0.447213595499955,-0.447213595499961,0.774596669241483));
#19284=DIRECTION('',(0.,-1.,0.));
#19285=DIRECTION('',(0.447213595499955,-0.447213595499961,-0.774596669241483));
#19286=DIRECTION('center_axis',(1.,0.,0.));
#19287=DIRECTION('ref_axis',(0.,0.,-1.));
#19288=DIRECTION('',(0.,0.,1.));
#19289=DIRECTION('',(0.,-1.,0.));
#19290=DIRECTION('',(0.,0.,-1.));
#19291=DIRECTION('center_axis',(0.707106781186548,-0.707106781186548,0.));
#19292=DIRECTION('ref_axis',(0.,0.,-1.));
#19293=DIRECTION('',(0.654653670707978,0.654653670707978,0.377964473009226));
#19294=DIRECTION('',(0.,0.,-1.));
#19295=DIRECTION('',(0.577350269189626,0.577350269189626,0.577350269189626));
#19296=DIRECTION('',(-0.357406744336597,-0.357406744336597,-0.862856209461014));
#19297=DIRECTION('center_axis',(0.353553390593274,-0.707106781186547,0.612372435695795));
#19298=DIRECTION('ref_axis',(0.866025403784439,0.,-0.5));
#19299=DIRECTION('',(-0.866025403784439,0.,0.5));
#19300=DIRECTION('',(0.654653670707978,0.654653670707978,0.377964473009226));
#19301=DIRECTION('',(0.866025403784439,0.,-0.5));
#19302=DIRECTION('center_axis',(0.353553390593273,0.707106781186548,-0.612372435695794));
#19303=DIRECTION('ref_axis',(-0.866025403784439,0.,-0.5));
#19304=DIRECTION('',(0.866025403784439,0.,0.5));
#19305=DIRECTION('',(0.654653670707977,-0.654653670707977,-0.377964473009228));
#19306=DIRECTION('',(-0.447213595499961,-0.447213595499955,-0.774596669241483));
#19307=DIRECTION('',(-0.866025403784439,0.,-0.5));
#19308=DIRECTION('',(-0.654653670707977,0.654653670707977,0.377964473009228));
#19309=DIRECTION('center_axis',(0.707106781186548,0.707106781186548,0.));
#19310=DIRECTION('ref_axis',(0.,0.,-1.));
#19311=DIRECTION('',(0.,0.,1.));
#19312=DIRECTION('',(0.,0.,-1.));
#19313=DIRECTION('',(-0.654653670707978,0.654653670707978,-0.377964473009226));
#19314=DIRECTION('center_axis',(0.353553390593274,0.707106781186547,0.612372435695795));
#19315=DIRECTION('ref_axis',(0.866025403784439,0.,-0.5));
#19316=DIRECTION('',(-0.654653670707978,0.654653670707978,-0.377964473009226));
#19317=DIRECTION('',(-0.866025403784439,0.,0.5));
#19318=DIRECTION('',(0.866025403784439,0.,-0.5));
#19319=DIRECTION('center_axis',(0.707106781186548,0.707106781186548,0.));
#19320=DIRECTION('ref_axis',(0.,0.,-1.));
#19321=DIRECTION('',(0.,0.,1.));
#19322=DIRECTION('',(0.577350269189626,-0.577350269189626,-0.577350269189626));
#19323=DIRECTION('',(-0.357406744336593,0.357406744336593,0.862856209461017));
#19324=DIRECTION('',(0.,0.,-1.));
#19325=DIRECTION('',(0.44721359549996,-0.44721359549996,0.774596669241481));
#19326=DIRECTION('center_axis',(0.,1.,0.));
#19327=DIRECTION('ref_axis',(0.,0.,1.));
#19328=DIRECTION('',(0.,0.,1.));
#19329=DIRECTION('',(1.,0.,0.));
#19330=DIRECTION('',(0.,0.,-1.));
#19331=DIRECTION('',(-1.,0.,0.));
#19332=DIRECTION('center_axis',(0.707106781186548,0.707106781186548,0.));
#19333=DIRECTION('ref_axis',(0.,0.,-1.));
#19334=DIRECTION('',(0.357406744336597,-0.357406744336597,0.862856209461014));
#19335=DIRECTION('',(-0.577350269189626,0.577350269189626,-0.577350269189626));
#19336=DIRECTION('center_axis',(-0.382683432365092,0.,-0.923879532511286));
#19337=DIRECTION('ref_axis',(-0.923879532511286,0.,0.382683432365092));
#19338=DIRECTION('',(-0.862856209461016,-0.357406744336594,0.357406744336595));
#19339=DIRECTION('',(0.,1.,0.));
#19340=DIRECTION('',(0.862856209461016,-0.357406744336594,-0.357406744336595));
#19341=DIRECTION('',(0.,-1.,0.));
#19342=DIRECTION('center_axis',(0.,-0.707106781186549,-0.707106781186546));
#19343=DIRECTION('ref_axis',(-1.,0.,0.));
#19344=DIRECTION('',(1.,0.,0.));
#19345=DIRECTION('',(-0.862856209461018,0.357406744336591,-0.357406744336592));
#19346=DIRECTION('',(0.577350269189627,-0.577350269189624,0.577350269189627));
#19347=DIRECTION('',(-1.,0.,0.));
#19348=DIRECTION('',(0.577350269189627,0.577350269189624,-0.577350269189627));
#19349=DIRECTION('center_axis',(0.,0.,-1.));
#19350=DIRECTION('ref_axis',(-1.,0.,0.));
#19351=DIRECTION('',(-1.,0.,0.));
#19352=DIRECTION('',(0.,1.,0.));
#19353=DIRECTION('center_axis',(-0.923879532511288,0.,-0.382683432365086));
#19354=DIRECTION('ref_axis',(-0.382683432365086,0.,0.923879532511288));
#19355=DIRECTION('',(0.357406744336591,0.357406744336589,-0.86285620946102));
#19356=DIRECTION('',(0.,-1.,0.));
#19357=DIRECTION('center_axis',(0.923879532511285,0.,-0.382683432365094));
#19358=DIRECTION('ref_axis',(-0.382683432365094,0.,-0.923879532511285));
#19359=DIRECTION('',(0.,1.,0.));
#19360=DIRECTION('center_axis',(0.707106781186548,0.,-0.707106781186548));
#19361=DIRECTION('ref_axis',(-0.707106781186548,0.,-0.707106781186548));
#19362=DIRECTION('',(0.,-1.,0.));
#19363=DIRECTION('',(-0.577350269189627,-0.577350269189624,-0.577350269189627));
#19364=DIRECTION('center_axis',(0.382683432365088,0.,-0.923879532511287));
#19365=DIRECTION('ref_axis',(-0.923879532511287,0.,-0.382683432365088));
#19366=DIRECTION('',(0.862856209461018,0.357406744336591,0.357406744336592));
#19367=DIRECTION('center_axis',(0.353553390593273,-0.707106781186548,-0.612372435695794));
#19368=DIRECTION('ref_axis',(-0.866025403784439,0.,-0.5));
#19369=DIRECTION('',(0.866025403784439,0.,0.5));
#19370=DIRECTION('',(0.447213595499961,-0.447213595499955,0.774596669241483));
#19371=DIRECTION('',(-0.654653670707977,-0.654653670707977,0.377964473009228));
#19372=DIRECTION('',(-0.866025403784439,0.,-0.5));
#19373=DIRECTION('',(0.654653670707977,0.654653670707977,-0.377964473009228));
#19374=DIRECTION('center_axis',(0.707106781186548,-0.707106781186548,0.));
#19375=DIRECTION('ref_axis',(0.,0.,-1.));
#19376=DIRECTION('',(0.,0.,-1.));
#19377=DIRECTION('',(0.,0.,1.));
#19378=DIRECTION('center_axis',(0.,1.,0.));
#19379=DIRECTION('ref_axis',(1.,0.,0.));
#19380=DIRECTION('',(0.,0.,-1.));
#19381=DIRECTION('',(-0.963357112062784,0.,0.2682220621762));
#19382=DIRECTION('',(0.,0.,1.));
#19383=DIRECTION('',(0.966551553961737,0.,0.256472403065422));
#19384=DIRECTION('',(0.,0.,-1.));
#19385=DIRECTION('',(-0.97411712880263,0.,-0.22604384391821));
#19386=DIRECTION('',(0.962508286041597,0.,-0.271252279808425));
#19387=DIRECTION('',(0.,0.,-1.));
#19388=DIRECTION('',(-0.962206043023297,0.,-0.272322475696461));
#19389=DIRECTION('',(0.97146241747779,0.,-0.237193531590151));
#19390=DIRECTION('',(0.,0.,-1.));
#19391=DIRECTION('',(-0.964398558141811,0.,0.264453060209172));
#19392=DIRECTION('',(0.,0.,1.));
#19393=DIRECTION('',(0.963801688090544,0.,0.266620153090154));
#19394=DIRECTION('',(0.,0.,1.));
#19395=DIRECTION('',(-0.940102113801967,0.,0.340892967990063));
#19396=DIRECTION('',(0.,0.,1.));
#19397=DIRECTION('',(0.933526017108979,0.,-0.358509658699241));
#19398=DIRECTION('',(0.,0.,-1.));
#19399=DIRECTION('',(-0.925486632914917,0.,-0.378780269147971));
#19400=DIRECTION('',(0.,0.,1.));
#19401=DIRECTION('',(0.933183015563907,0.,0.359401529578064));
#19402=DIRECTION('',(0.,0.,-1.));
#19403=DIRECTION('',(-1.,0.,0.));
#19404=DIRECTION('',(0.,0.,1.));
#19405=DIRECTION('',(1.,0.,0.));
#19406=DIRECTION('',(1.,0.,3.11798350272655E-15));
#19407=DIRECTION('',(1.,0.,0.));
#19408=DIRECTION('',(0.,0.,1.));
#19409=DIRECTION('',(1.,0.,0.));
#19410=DIRECTION('',(0.0016102970727879,0.,-0.999998703470828));
#19411=DIRECTION('',(-1.,0.,0.));
#19412=DIRECTION('',(-0.264515837084414,0.,0.964381341550909));
#19413=DIRECTION('center_axis',(0.707106781186548,-0.707106781186548,0.));
#19414=DIRECTION('ref_axis',(0.,0.,-1.));
#19415=DIRECTION('',(-0.44721359549996,-0.44721359549996,-0.774596669241481));
#19416=DIRECTION('',(0.,0.,1.));
#19417=DIRECTION('',(0.357406744336593,0.357406744336593,-0.862856209461017));
#19418=DIRECTION('',(-0.577350269189626,-0.577350269189626,0.577350269189626));
#19419=DIRECTION('center_axis',(0.866025403784437,0.,-0.500000000000003));
#19420=DIRECTION('ref_axis',(-0.500000000000003,0.,-0.866025403784437));
#19421=DIRECTION('',(0.,-1.,0.));
#19422=DIRECTION('',(0.,1.,0.));
#19423=DIRECTION('center_axis',(1.,0.,0.));
#19424=DIRECTION('ref_axis',(0.,0.,-1.));
#19425=DIRECTION('',(0.,1.,0.));
#19426=DIRECTION('center_axis',(0.382683432365092,0.,0.923879532511286));
#19427=DIRECTION('ref_axis',(0.923879532511286,0.,-0.382683432365092));
#19428=DIRECTION('',(0.,1.,0.));
#19429=DIRECTION('',(-0.862856209461016,-0.357406744336594,0.357406744336595));
#19430=DIRECTION('center_axis',(0.,0.707106781186549,0.707106781186546));
#19431=DIRECTION('ref_axis',(1.,0.,0.));
#19432=DIRECTION('',(0.577350269189627,0.577350269189624,-0.577350269189627));
#19433=DIRECTION('',(0.577350269189627,-0.577350269189624,0.577350269189627));
#19434=DIRECTION('center_axis',(0.707106781186548,0.,0.707106781186548));
#19435=DIRECTION('ref_axis',(0.707106781186548,0.,-0.707106781186548));
#19436=DIRECTION('',(0.,-1.,0.));
#19437=DIRECTION('center_axis',(0.923879532511287,0.,0.382683432365089));
#19438=DIRECTION('ref_axis',(0.382683432365089,0.,-0.923879532511287));
#19439=DIRECTION('',(0.,1.,0.));
#19440=DIRECTION('',(0.,1.,0.));
#19441=DIRECTION('',(0.,1.,0.));
#19442=DIRECTION('center_axis',(-0.266620153090154,0.,0.963801688090544));
#19443=DIRECTION('ref_axis',(0.963801688090544,0.,0.266620153090154));
#19444=DIRECTION('',(0.,1.,0.));
#19445=DIRECTION('',(0.963801688090544,0.,0.266620153090154));
#19446=DIRECTION('center_axis',(-1.,0.,0.));
#19447=DIRECTION('ref_axis',(0.,0.,1.));
#19448=DIRECTION('',(0.,1.,0.));
#19449=DIRECTION('',(0.,0.,1.));
#19450=DIRECTION('center_axis',(-0.264453060209172,0.,-0.964398558141811));
#19451=DIRECTION('ref_axis',(-0.964398558141811,0.,0.264453060209172));
#19452=DIRECTION('',(0.,1.,0.));
#19453=DIRECTION('',(-0.964398558141811,0.,0.264453060209172));
#19454=DIRECTION('center_axis',(1.,0.,0.));
#19455=DIRECTION('ref_axis',(0.,0.,-1.));
#19456=DIRECTION('',(0.,1.,0.));
#19457=DIRECTION('',(0.,0.,-1.));
#19458=DIRECTION('center_axis',(0.237193531590151,0.,0.97146241747779));
#19459=DIRECTION('ref_axis',(0.97146241747779,0.,-0.237193531590151));
#19460=DIRECTION('',(0.,1.,0.));
#19461=DIRECTION('',(0.97146241747779,0.,-0.237193531590151));
#19462=DIRECTION('',(0.,1.,0.));
#19463=DIRECTION('',(0.,1.,0.));
#19464=DIRECTION('center_axis',(0.272322475696461,0.,-0.962206043023297));
#19465=DIRECTION('ref_axis',(-0.962206043023297,0.,-0.272322475696461));
#19466=DIRECTION('',(0.,1.,0.));
#19467=DIRECTION('',(-0.962206043023297,0.,-0.272322475696461));
#19468=DIRECTION('center_axis',(1.,0.,0.));
#19469=DIRECTION('ref_axis',(0.,0.,-1.));
#19470=DIRECTION('',(0.,1.,0.));
#19471=DIRECTION('',(0.,0.,-1.));
#19472=DIRECTION('center_axis',(0.271252279808425,0.,0.962508286041597));
#19473=DIRECTION('ref_axis',(0.962508286041597,0.,-0.271252279808425));
#19474=DIRECTION('',(0.,1.,0.));
#19475=DIRECTION('',(0.962508286041597,0.,-0.271252279808425));
#19476=DIRECTION('',(0.,1.,0.));
#19477=DIRECTION('',(0.,1.,0.));
#19478=DIRECTION('center_axis',(0.22604384391821,0.,-0.97411712880263));
#19479=DIRECTION('ref_axis',(-0.97411712880263,0.,-0.22604384391821));
#19480=DIRECTION('',(0.,1.,0.));
#19481=DIRECTION('',(-0.97411712880263,0.,-0.22604384391821));
#19482=DIRECTION('center_axis',(1.,0.,0.));
#19483=DIRECTION('ref_axis',(0.,0.,-1.));
#19484=DIRECTION('',(0.,1.,0.));
#19485=DIRECTION('',(0.,0.,-1.));
#19486=DIRECTION('center_axis',(-0.256472403065422,0.,0.966551553961737));
#19487=DIRECTION('ref_axis',(0.966551553961737,0.,0.256472403065422));
#19488=DIRECTION('',(0.,1.,0.));
#19489=DIRECTION('',(0.966551553961737,0.,0.256472403065422));
#19490=DIRECTION('center_axis',(-1.,0.,0.));
#19491=DIRECTION('ref_axis',(0.,0.,1.));
#19492=DIRECTION('',(0.,1.,0.));
#19493=DIRECTION('',(0.,0.,1.));
#19494=DIRECTION('center_axis',(-0.2682220621762,0.,-0.963357112062784));
#19495=DIRECTION('ref_axis',(-0.963357112062784,0.,0.2682220621762));
#19496=DIRECTION('',(-0.963357112062784,0.,0.2682220621762));
#19497=DIRECTION('center_axis',(0.,-1.,0.));
#19498=DIRECTION('ref_axis',(-1.,0.,0.));
#19499=DIRECTION('center_axis',(-1.,0.,0.));
#19500=DIRECTION('ref_axis',(0.,0.,1.));
#19501=DIRECTION('',(0.,1.,0.));
#19502=DIRECTION('',(0.,0.,1.));
#19503=DIRECTION('',(0.,1.,0.));
#19504=DIRECTION('center_axis',(-0.359401529578064,0.,0.933183015563908));
#19505=DIRECTION('ref_axis',(0.933183015563907,0.,0.359401529578064));
#19506=DIRECTION('',(0.,1.,0.));
#19507=DIRECTION('',(0.933183015563907,0.,0.359401529578064));
#19508=DIRECTION('center_axis',(-1.,0.,0.));
#19509=DIRECTION('ref_axis',(0.,0.,1.));
#19510=DIRECTION('',(0.,1.,0.));
#19511=DIRECTION('',(0.,0.,1.));
#19512=DIRECTION('center_axis',(0.378780269147971,0.,-0.925486632914917));
#19513=DIRECTION('ref_axis',(-0.925486632914917,0.,-0.378780269147971));
#19514=DIRECTION('',(0.,1.,0.));
#19515=DIRECTION('',(-0.925486632914917,0.,-0.378780269147971));
#19516=DIRECTION('center_axis',(1.,0.,0.));
#19517=DIRECTION('ref_axis',(0.,0.,-1.));
#19518=DIRECTION('',(0.,1.,0.));
#19519=DIRECTION('',(0.,0.,-1.));
#19520=DIRECTION('center_axis',(0.358509658699241,0.,0.933526017108979));
#19521=DIRECTION('ref_axis',(0.933526017108979,0.,-0.358509658699241));
#19522=DIRECTION('',(0.,1.,0.));
#19523=DIRECTION('',(0.933526017108979,0.,-0.358509658699241));
#19524=DIRECTION('center_axis',(-1.,0.,0.));
#19525=DIRECTION('ref_axis',(0.,0.,1.));
#19526=DIRECTION('',(0.,1.,0.));
#19527=DIRECTION('',(0.,0.,1.));
#19528=DIRECTION('center_axis',(-0.340892967990063,0.,-0.940102113801967));
#19529=DIRECTION('ref_axis',(-0.940102113801967,0.,0.340892967990063));
#19530=DIRECTION('',(-0.940102113801967,0.,0.340892967990063));
#19531=DIRECTION('center_axis',(0.,1.,0.));
#19532=DIRECTION('ref_axis',(0.,0.,1.));
#19533=DIRECTION('',(0.,1.,0.));
#19534=DIRECTION('',(0.,1.,0.));
#19535=DIRECTION('',(0.,1.,0.));
#19536=DIRECTION('',(0.,1.,0.));
#19537=DIRECTION('',(0.,1.,0.));
#19538=DIRECTION('',(0.,1.,0.));
#19539=DIRECTION('',(0.,1.,0.));
#19540=DIRECTION('',(0.,1.,0.));
#19541=DIRECTION('',(0.,1.,0.));
#19542=DIRECTION('',(0.,1.,0.));
#19543=DIRECTION('',(0.,1.,0.));
#19544=DIRECTION('',(0.,1.,0.));
#19545=DIRECTION('center_axis',(0.,-1.,0.));
#19546=DIRECTION('ref_axis',(-1.,0.,0.));
#19547=DIRECTION('',(0.,1.,0.));
#19548=DIRECTION('',(0.,1.,0.));
#19549=DIRECTION('',(0.,1.,0.));
#19550=DIRECTION('center_axis',(-3.11798350272655E-15,0.,1.));
#19551=DIRECTION('ref_axis',(1.,0.,3.11798350272655E-15));
#19552=DIRECTION('',(0.,1.,0.));
#19553=DIRECTION('',(1.,0.,3.11798350272655E-15));
#19554=DIRECTION('',(0.,1.,0.));
#19555=DIRECTION('',(0.,1.,0.));
#19556=DIRECTION('center_axis',(0.,0.,1.));
#19557=DIRECTION('ref_axis',(1.,0.,0.));
#19558=DIRECTION('',(0.,1.,0.));
#19559=DIRECTION('',(1.,0.,0.));
#19560=DIRECTION('center_axis',(-1.,0.,0.));
#19561=DIRECTION('ref_axis',(0.,0.,1.));
#19562=DIRECTION('',(0.,1.,0.));
#19563=DIRECTION('',(0.,0.,1.));
#19564=DIRECTION('center_axis',(0.,0.,-1.));
#19565=DIRECTION('ref_axis',(-1.,0.,0.));
#19566=DIRECTION('',(0.,1.,0.));
#19567=DIRECTION('',(-1.,0.,0.));
#19568=DIRECTION('center_axis',(1.,0.,0.));
#19569=DIRECTION('ref_axis',(0.,0.,-1.));
#19570=DIRECTION('',(0.,0.,-1.));
#19571=DIRECTION('center_axis',(0.,-1.,0.));
#19572=DIRECTION('ref_axis',(-1.,0.,0.));
#19573=DIRECTION('',(0.,1.,0.));
#19574=DIRECTION('',(0.,1.,0.));
#19575=DIRECTION('',(0.,1.,0.));
#19576=DIRECTION('',(0.,1.,0.));
#19577=DIRECTION('',(0.,1.,0.));
#19578=DIRECTION('',(0.,1.,0.));
#19579=DIRECTION('',(0.,1.,0.));
#19580=DIRECTION('',(0.,1.,0.));
#19581=DIRECTION('',(0.,1.,0.));
#19582=DIRECTION('',(0.,1.,0.));
#19583=DIRECTION('',(0.,1.,0.));
#19584=DIRECTION('',(0.,1.,0.));
#19585=DIRECTION('',(0.,1.,0.));
#19586=DIRECTION('center_axis',(-0.964381341550909,0.,-0.264515837084414));
#19587=DIRECTION('ref_axis',(-0.264515837084414,0.,0.964381341550909));
#19588=DIRECTION('',(0.,1.,0.));
#19589=DIRECTION('',(-0.264515837084414,0.,0.964381341550909));
#19590=DIRECTION('',(0.,1.,0.));
#19591=DIRECTION('',(0.,1.,0.));
#19592=DIRECTION('',(0.,1.,0.));
#19593=DIRECTION('',(0.,1.,0.));
#19594=DIRECTION('',(0.,1.,0.));
#19595=DIRECTION('',(0.,1.,0.));
#19596=DIRECTION('',(0.,1.,0.));
#19597=DIRECTION('',(0.,1.,0.));
#19598=DIRECTION('',(0.,1.,0.));
#19599=DIRECTION('',(0.,1.,0.));
#19600=DIRECTION('',(0.,1.,0.));
#19601=DIRECTION('center_axis',(0.,0.,-1.));
#19602=DIRECTION('ref_axis',(-1.,0.,0.));
#19603=DIRECTION('',(0.,1.,0.));
#19604=DIRECTION('',(-1.,0.,0.));
#19605=DIRECTION('center_axis',(0.999998703470828,0.,0.0016102970727879));
#19606=DIRECTION('ref_axis',(0.0016102970727879,0.,-0.999998703470828));
#19607=DIRECTION('',(0.,1.,0.));
#19608=DIRECTION('',(0.0016102970727879,0.,-0.999998703470828));
#19609=DIRECTION('center_axis',(0.,0.,1.));
#19610=DIRECTION('ref_axis',(1.,0.,0.));
#19611=DIRECTION('',(0.,1.,0.));
#19612=DIRECTION('',(1.,0.,0.));
#19613=DIRECTION('center_axis',(-1.,0.,0.));
#19614=DIRECTION('ref_axis',(0.,0.,1.));
#19615=DIRECTION('',(0.,1.,0.));
#19616=DIRECTION('',(0.,0.,1.));
#19617=DIRECTION('center_axis',(0.,0.,1.));
#19618=DIRECTION('ref_axis',(1.,0.,0.));
#19619=DIRECTION('',(1.,0.,0.));
#19620=DIRECTION('center_axis',(0.,-1.,0.));
#19621=DIRECTION('ref_axis',(-1.,0.,0.));
#19622=DIRECTION('center_axis',(-0.707106781186548,0.,-0.707106781186548));
#19623=DIRECTION('ref_axis',(-0.707106781186548,0.,0.707106781186548));
#19624=DIRECTION('',(-0.577350269189627,-0.577350269189624,0.577350269189627));
#19625=DIRECTION('',(-0.577350269189627,0.577350269189624,0.577350269189627));
#19626=DIRECTION('center_axis',(-0.707106781186546,0.707106781186549,0.));
#19627=DIRECTION('ref_axis',(0.,0.,1.));
#19628=DIRECTION('',(0.577350269189627,0.577350269189624,0.577350269189627));
#19629=DIRECTION('center_axis',(0.,0.707106781186549,-0.707106781186546));
#19630=DIRECTION('ref_axis',(-1.,0.,0.));
#19631=DIRECTION('center_axis',(-0.5,0.,-0.866025403784439));
#19632=DIRECTION('ref_axis',(-0.866025403784439,0.,0.5));
#19633=DIRECTION('',(0.,1.,0.));
#19634=DIRECTION('center_axis',(-0.707106781186548,0.,0.707106781186548));
#19635=DIRECTION('ref_axis',(0.707106781186548,0.,0.707106781186548));
#19636=DIRECTION('center_axis',(-0.5,0.,0.866025403784439));
#19637=DIRECTION('ref_axis',(0.866025403784439,0.,0.5));
#19638=DIRECTION('',(0.,1.,0.));
#19639=DIRECTION('center_axis',(-1.,0.,0.));
#19640=DIRECTION('ref_axis',(0.,0.,1.));
#19641=DIRECTION('axis',(0.,0.,1.));
#19642=DIRECTION('refdir',(1.,0.,0.));
#19643=DIRECTION('center_axis',(-1.,0.,0.));
#19644=DIRECTION('ref_axis',(0.,0.,1.));
#19645=DIRECTION('center_axis',(1.,0.,0.));
#19646=DIRECTION('ref_axis',(0.,0.,-1.));
#19647=DIRECTION('center_axis',(1.,0.,0.));
#19648=DIRECTION('ref_axis',(0.,1.,0.));
#19649=DIRECTION('center_axis',(1.,0.,0.));
#19650=DIRECTION('ref_axis',(0.,0.,-1.));
#19651=DIRECTION('',(-0.707106781186548,0.707106781186547,8.65956056235493E-17));
#19652=DIRECTION('center_axis',(1.,0.,0.));
#19653=DIRECTION('ref_axis',(0.,1.,0.));
#19654=DIRECTION('center_axis',(1.,0.,0.));
#19655=DIRECTION('ref_axis',(0.,0.,-1.));
#19656=DIRECTION('',(-1.,0.,0.));
#19657=DIRECTION('center_axis',(1.,0.,0.));
#19658=DIRECTION('ref_axis',(0.,0.,-1.));
#19659=DIRECTION('center_axis',(1.,0.,0.));
#19660=DIRECTION('ref_axis',(0.,0.,-1.));
#19661=DIRECTION('center_axis',(1.,0.,0.));
#19662=DIRECTION('ref_axis',(0.,1.,0.));
#19663=DIRECTION('center_axis',(1.,0.,0.));
#19664=DIRECTION('ref_axis',(0.,0.,-1.));
#19665=DIRECTION('',(-1.,0.,0.));
#19666=DIRECTION('center_axis',(-1.,0.,0.));
#19667=DIRECTION('ref_axis',(0.,0.,1.));
#19668=DIRECTION('center_axis',(1.,0.,0.));
#19669=DIRECTION('ref_axis',(0.,0.,-1.));
#19670=DIRECTION('center_axis',(1.,0.,0.));
#19671=DIRECTION('ref_axis',(0.,1.,0.));
#19672=DIRECTION('center_axis',(1.,0.,0.));
#19673=DIRECTION('ref_axis',(0.,0.,-1.));
#19674=DIRECTION('',(-1.,0.,0.));
#19675=DIRECTION('center_axis',(1.,0.,0.));
#19676=DIRECTION('ref_axis',(0.,0.,-1.));
#19677=DIRECTION('center_axis',(1.,0.,0.));
#19678=DIRECTION('ref_axis',(0.,0.,-1.));
#19679=DIRECTION('center_axis',(1.,0.,0.));
#19680=DIRECTION('ref_axis',(0.,1.,0.));
#19681=DIRECTION('center_axis',(1.,0.,0.));
#19682=DIRECTION('ref_axis',(0.,0.,-1.));
#19683=DIRECTION('',(-1.,0.,0.));
#19684=DIRECTION('center_axis',(-1.,0.,0.));
#19685=DIRECTION('ref_axis',(0.,0.,1.));
#19686=DIRECTION('center_axis',(1.,0.,0.));
#19687=DIRECTION('ref_axis',(0.,0.,-1.));
#19688=DIRECTION('center_axis',(1.,0.,0.));
#19689=DIRECTION('ref_axis',(0.,1.,0.));
#19690=DIRECTION('center_axis',(1.,0.,0.));
#19691=DIRECTION('ref_axis',(0.,0.,-1.));
#19692=DIRECTION('',(-1.,0.,0.));
#19693=DIRECTION('center_axis',(-1.,0.,0.));
#19694=DIRECTION('ref_axis',(0.,1.,0.));
#19695=DIRECTION('center_axis',(1.,0.,0.));
#19696=DIRECTION('ref_axis',(0.,0.,-1.));
#19697=DIRECTION('',(-0.707106781186548,-0.707106781186547,-8.65956056235493E-17));
#19698=DIRECTION('center_axis',(1.,0.,0.));
#19699=DIRECTION('ref_axis',(0.,0.,-1.));
#19700=DIRECTION('axis',(0.,0.,1.));
#19701=DIRECTION('refdir',(1.,0.,0.));
#19702=DIRECTION('center_axis',(1.,0.,0.));
#19703=DIRECTION('ref_axis',(0.,1.,0.));
#19704=DIRECTION('',(-1.,0.,0.));
#19705=DIRECTION('center_axis',(-1.,0.,0.));
#19706=DIRECTION('ref_axis',(0.,1.,0.));
#19707=DIRECTION('center_axis',(1.,0.,0.));
#19708=DIRECTION('ref_axis',(0.,1.,0.));
#19709=DIRECTION('',(-1.,0.,0.));
#19710=DIRECTION('center_axis',(1.,0.,0.));
#19711=DIRECTION('ref_axis',(0.,1.,0.));
#19712=DIRECTION('',(-1.,0.,0.));
#19713=DIRECTION('center_axis',(1.,0.,0.));
#19714=DIRECTION('ref_axis',(0.,1.,0.));
#19715=DIRECTION('',(-1.,0.,0.));
#19716=DIRECTION('center_axis',(1.,0.,0.));
#19717=DIRECTION('ref_axis',(0.,1.,0.));
#19718=DIRECTION('',(-1.,0.,0.));
#19719=DIRECTION('center_axis',(1.,0.,0.));
#19720=DIRECTION('ref_axis',(0.,1.,0.));
#19721=DIRECTION('',(-1.,0.,0.));
#19722=DIRECTION('center_axis',(1.,0.,0.));
#19723=DIRECTION('ref_axis',(0.,1.,0.));
#19724=DIRECTION('',(-1.,0.,0.));
#19725=DIRECTION('center_axis',(1.,0.,0.));
#19726=DIRECTION('ref_axis',(0.,1.,0.));
#19727=DIRECTION('',(-1.,0.,0.));
#19728=DIRECTION('center_axis',(1.,0.,0.));
#19729=DIRECTION('ref_axis',(0.,1.,0.));
#19730=DIRECTION('',(-1.,0.,0.));
#19731=DIRECTION('center_axis',(1.,0.,0.));
#19732=DIRECTION('ref_axis',(0.,1.,0.));
#19733=DIRECTION('',(-1.,0.,0.));
#19734=DIRECTION('center_axis',(1.,0.,0.));
#19735=DIRECTION('ref_axis',(0.,1.,0.));
#19736=DIRECTION('',(-1.,0.,0.));
#19737=DIRECTION('center_axis',(1.,0.,0.));
#19738=DIRECTION('ref_axis',(0.,1.,0.));
#19739=DIRECTION('',(-1.,0.,0.));
#19740=DIRECTION('center_axis',(1.,0.,0.));
#19741=DIRECTION('ref_axis',(0.,1.,5.00345854329736E-14));
#19742=DIRECTION('',(1.,0.,0.));
#19743=DIRECTION('center_axis',(1.,0.,0.));
#19744=DIRECTION('ref_axis',(0.,1.,5.00345854329736E-14));
#19745=DIRECTION('center_axis',(1.,0.,0.));
#19746=DIRECTION('ref_axis',(0.,1.,5.00345854329736E-14));
#19747=DIRECTION('',(1.,0.,0.));
#19748=DIRECTION('center_axis',(1.,0.,0.));
#19749=DIRECTION('ref_axis',(0.,1.,5.00345854329736E-14));
#19750=DIRECTION('',(1.,0.,0.));
#19751=DIRECTION('center_axis',(1.,0.,0.));
#19752=DIRECTION('ref_axis',(0.,1.,5.00345854329736E-14));
#19753=DIRECTION('',(1.,0.,0.));
#19754=DIRECTION('center_axis',(1.,0.,0.));
#19755=DIRECTION('ref_axis',(0.,1.,5.00345854329736E-14));
#19756=DIRECTION('',(1.,0.,0.));
#19757=DIRECTION('center_axis',(1.,0.,0.));
#19758=DIRECTION('ref_axis',(0.,1.,5.00345854329736E-14));
#19759=DIRECTION('',(1.,0.,0.));
#19760=DIRECTION('center_axis',(1.,0.,0.));
#19761=DIRECTION('ref_axis',(0.,1.,5.00345854329736E-14));
#19762=DIRECTION('',(1.,0.,0.));
#19763=DIRECTION('center_axis',(1.,0.,0.));
#19764=DIRECTION('ref_axis',(0.,1.,5.00345854329736E-14));
#19765=DIRECTION('',(1.,0.,0.));
#19766=DIRECTION('center_axis',(1.,0.,0.));
#19767=DIRECTION('ref_axis',(0.,1.,5.00345854329736E-14));
#19768=DIRECTION('',(1.,0.,0.));
#19769=DIRECTION('center_axis',(1.,0.,0.));
#19770=DIRECTION('ref_axis',(0.,1.,5.00345854329736E-14));
#19771=DIRECTION('',(1.,0.,0.));
#19772=DIRECTION('center_axis',(1.,0.,0.));
#19773=DIRECTION('ref_axis',(0.,1.,5.00345854329736E-14));
#19774=DIRECTION('',(1.,0.,0.));
#19775=DIRECTION('center_axis',(-1.,0.,-2.40145555254033E-15));
#19776=DIRECTION('ref_axis',(0.,-1.,-3.14504206142599E-17));
#19777=DIRECTION('center_axis',(-1.,0.,0.));
#19778=DIRECTION('ref_axis',(0.,-1.,0.));
#19779=DIRECTION('',(-0.433188730489141,0.901303236306853,-9.01559303907765E-16));
#19780=DIRECTION('center_axis',(1.,0.,0.));
#19781=DIRECTION('ref_axis',(0.,-1.,-6.12323399573677E-17));
#19782=DIRECTION('center_axis',(1.,0.,0.));
#19783=DIRECTION('ref_axis',(0.,-1.,-6.12323399573677E-17));
#19784=DIRECTION('center_axis',(-1.,0.,0.));
#19785=DIRECTION('ref_axis',(0.,1.,0.));
#19786=DIRECTION('',(-0.78086880944303,-0.624695047554424,-7.65030790430729E-17));
#19787=DIRECTION('center_axis',(-1.,0.,0.));
#19788=DIRECTION('ref_axis',(0.,-1.,-6.12323399573677E-17));
#19789=DIRECTION('center_axis',(-1.,0.,0.));
#19790=DIRECTION('ref_axis',(0.,-1.,-6.12323399573677E-17));
#19791=DIRECTION('center_axis',(1.,0.,0.));
#19792=DIRECTION('ref_axis',(0.,0.,-1.));
#19793=DIRECTION('center_axis',(-1.,0.,0.));
#19794=DIRECTION('ref_axis',(0.,1.,5.00345854329736E-14));
#19795=DIRECTION('center_axis',(-1.,0.,1.56015765102107E-15));
#19796=DIRECTION('ref_axis',(0.,-1.,-3.04068599274537E-17));
#19797=DIRECTION('',(-0.943628319160417,0.331006941435501,1.52281048269397E-15));
#19798=DIRECTION('center_axis',(1.,0.,0.));
#19799=DIRECTION('ref_axis',(0.,-1.,0.));
#19800=DIRECTION('center_axis',(1.,0.,0.));
#19801=DIRECTION('ref_axis',(0.,-1.,0.));
#19802=DIRECTION('center_axis',(1.,0.,0.));
#19803=DIRECTION('ref_axis',(0.,1.,0.));
#19804=DIRECTION('',(-1.,0.,0.));
#19805=DIRECTION('center_axis',(1.,0.,0.));
#19806=DIRECTION('ref_axis',(0.,0.,-1.));
#19807=DIRECTION('center_axis',(1.,0.,0.));
#19808=DIRECTION('ref_axis',(0.,0.,-1.));
#19809=DIRECTION('center_axis',(-1.,0.,0.));
#19810=DIRECTION('ref_axis',(0.,1.,0.));
#19811=DIRECTION('center_axis',(-1.,0.,0.));
#19812=DIRECTION('ref_axis',(0.,1.,0.));
#19813=DIRECTION('center_axis',(1.,0.,0.));
#19814=DIRECTION('ref_axis',(0.,0.888975527931182,0.457954703807566));
#19815=DIRECTION('center_axis',(1.,0.,0.));
#19816=DIRECTION('ref_axis',(0.,-0.48878186078128,-0.872406036528398));
#19817=DIRECTION('center_axis',(-1.,0.,0.));
#19818=DIRECTION('ref_axis',(0.,1.,0.));
#19819=DIRECTION('center_axis',(1.,0.,0.));
#19820=DIRECTION('ref_axis',(0.,1.,0.));
#19821=DIRECTION('center_axis',(1.,0.,0.));
#19822=DIRECTION('ref_axis',(0.,0.,-1.));
#19823=DIRECTION('',(-1.,0.,0.));
#19824=DIRECTION('center_axis',(1.,0.,0.));
#19825=DIRECTION('ref_axis',(0.,0.,-1.));
#19826=DIRECTION('center_axis',(-1.,0.,0.));
#19827=DIRECTION('ref_axis',(0.,0.,1.));
#19828=DIRECTION('center_axis',(1.,0.,0.));
#19829=DIRECTION('ref_axis',(0.,0.,-1.));
#19830=DIRECTION('center_axis',(1.,0.,0.));
#19831=DIRECTION('ref_axis',(0.,1.,0.));
#19832=DIRECTION('',(-0.707106781186555,0.70710678118654,8.65956056235484E-17));
#19833=DIRECTION('center_axis',(-1.,0.,0.));
#19834=DIRECTION('ref_axis',(0.,1.,0.));
#19835=DIRECTION('center_axis',(1.,0.,0.));
#19836=DIRECTION('ref_axis',(0.,0.,-1.));
#19837=DIRECTION('',(-0.707106781186555,-0.70710678118654,-8.65956056235484E-17));
#19838=DIRECTION('center_axis',(1.,0.,0.));
#19839=DIRECTION('ref_axis',(0.,0.,-1.));
#19840=DIRECTION('center_axis',(1.,0.,0.));
#19841=DIRECTION('ref_axis',(0.,0.,-1.));
#19842=DIRECTION('center_axis',(1.,0.,0.));
#19843=DIRECTION('ref_axis',(0.,1.,0.));
#19844=DIRECTION('',(-1.,0.,0.));
#19845=DIRECTION('center_axis',(1.,0.,0.));
#19846=DIRECTION('ref_axis',(0.,0.,-1.));
#19847=DIRECTION('center_axis',(-1.,0.,0.));
#19848=DIRECTION('ref_axis',(0.,0.,1.));
#19849=DIRECTION('center_axis',(1.,0.,0.));
#19850=DIRECTION('ref_axis',(0.,0.,-1.));
#19851=DIRECTION('center_axis',(1.,0.,0.));
#19852=DIRECTION('ref_axis',(0.,1.,0.));
#19853=DIRECTION('',(-1.,0.,0.));
#19854=DIRECTION('center_axis',(1.,0.,0.));
#19855=DIRECTION('ref_axis',(0.,0.,-1.));
#19856=DIRECTION('center_axis',(1.,0.,0.));
#19857=DIRECTION('ref_axis',(0.,0.,-1.));
#19858=DIRECTION('axis',(0.,0.,1.));
#19859=DIRECTION('refdir',(1.,0.,0.));
#19860=DIRECTION('center_axis',(1.,0.,0.));
#19861=DIRECTION('ref_axis',(0.,1.,0.));
#19862=DIRECTION('',(-1.,0.,0.));
#19863=DIRECTION('center_axis',(1.,0.,0.));
#19864=DIRECTION('ref_axis',(0.,1.,0.));
#19865=DIRECTION('center_axis',(1.,0.,0.));
#19866=DIRECTION('ref_axis',(0.,1.,0.));
#19867=DIRECTION('',(-1.,0.,0.));
#19868=DIRECTION('center_axis',(1.,0.,0.));
#19869=DIRECTION('ref_axis',(0.,1.,0.));
#19870=DIRECTION('',(-1.,0.,0.));
#19871=DIRECTION('center_axis',(1.,0.,0.));
#19872=DIRECTION('ref_axis',(0.,1.,0.));
#19873=DIRECTION('',(-1.,0.,0.));
#19874=DIRECTION('center_axis',(1.,0.,0.));
#19875=DIRECTION('ref_axis',(0.,1.,0.));
#19876=DIRECTION('',(-1.,0.,0.));
#19877=DIRECTION('center_axis',(1.,0.,0.));
#19878=DIRECTION('ref_axis',(0.,1.,0.));
#19879=DIRECTION('',(-1.,0.,0.));
#19880=DIRECTION('center_axis',(1.,0.,0.));
#19881=DIRECTION('ref_axis',(0.,1.,0.));
#19882=DIRECTION('',(-1.,0.,0.));
#19883=DIRECTION('center_axis',(1.,0.,0.));
#19884=DIRECTION('ref_axis',(0.,1.,0.));
#19885=DIRECTION('',(-1.,0.,0.));
#19886=DIRECTION('center_axis',(1.,0.,0.));
#19887=DIRECTION('ref_axis',(0.,1.,0.));
#19888=DIRECTION('',(-1.,0.,0.));
#19889=DIRECTION('center_axis',(1.,0.,0.));
#19890=DIRECTION('ref_axis',(0.,1.,0.));
#19891=DIRECTION('',(-1.,0.,0.));
#19892=DIRECTION('center_axis',(1.,0.,0.));
#19893=DIRECTION('ref_axis',(0.,1.,0.));
#19894=DIRECTION('',(-1.,0.,0.));
#19895=DIRECTION('center_axis',(1.,0.,0.));
#19896=DIRECTION('ref_axis',(0.,1.,0.));
#19897=DIRECTION('',(-1.,0.,0.));
#19898=DIRECTION('center_axis',(1.,0.,0.));
#19899=DIRECTION('ref_axis',(0.,1.,0.));
#19900=DIRECTION('',(-1.,0.,0.));
#19901=DIRECTION('center_axis',(1.,0.,0.));
#19902=DIRECTION('ref_axis',(0.,1.,7.05550968452284E-14));
#19903=DIRECTION('',(1.,0.,0.));
#19904=DIRECTION('center_axis',(1.,0.,0.));
#19905=DIRECTION('ref_axis',(0.,1.,7.05550968452284E-14));
#19906=DIRECTION('center_axis',(1.,0.,0.));
#19907=DIRECTION('ref_axis',(0.,1.,7.05550968452284E-14));
#19908=DIRECTION('',(1.,0.,0.));
#19909=DIRECTION('center_axis',(1.,0.,0.));
#19910=DIRECTION('ref_axis',(0.,1.,7.05550968452284E-14));
#19911=DIRECTION('center_axis',(1.,0.,0.));
#19912=DIRECTION('ref_axis',(0.,1.,7.05550968452284E-14));
#19913=DIRECTION('',(1.,0.,0.));
#19914=DIRECTION('center_axis',(1.,0.,0.));
#19915=DIRECTION('ref_axis',(0.,1.,7.05550968452284E-14));
#19916=DIRECTION('',(1.,0.,0.));
#19917=DIRECTION('center_axis',(1.,0.,0.));
#19918=DIRECTION('ref_axis',(0.,1.,7.05550968452284E-14));
#19919=DIRECTION('',(1.,0.,0.));
#19920=DIRECTION('center_axis',(1.,0.,0.));
#19921=DIRECTION('ref_axis',(0.,1.,7.05550968452284E-14));
#19922=DIRECTION('',(1.,0.,0.));
#19923=DIRECTION('center_axis',(1.,0.,0.));
#19924=DIRECTION('ref_axis',(0.,1.,7.05550968452284E-14));
#19925=DIRECTION('',(1.,0.,0.));
#19926=DIRECTION('center_axis',(1.,0.,0.));
#19927=DIRECTION('ref_axis',(0.,1.,7.05550968452284E-14));
#19928=DIRECTION('',(1.,0.,0.));
#19929=DIRECTION('center_axis',(1.,0.,0.));
#19930=DIRECTION('ref_axis',(0.,1.,7.05550968452284E-14));
#19931=DIRECTION('',(1.,0.,0.));
#19932=DIRECTION('center_axis',(1.,0.,0.));
#19933=DIRECTION('ref_axis',(0.,1.,7.05550968452284E-14));
#19934=DIRECTION('',(1.,0.,0.));
#19935=DIRECTION('center_axis',(1.,0.,0.));
#19936=DIRECTION('ref_axis',(0.,1.,7.05550968452284E-14));
#19937=DIRECTION('',(1.,0.,0.));
#19938=DIRECTION('center_axis',(1.,0.,0.));
#19939=DIRECTION('ref_axis',(0.,1.,7.05550968452284E-14));
#19940=DIRECTION('',(1.,0.,0.));
#19941=DIRECTION('center_axis',(1.,0.,0.));
#19942=DIRECTION('ref_axis',(0.,1.,7.05550968452284E-14));
#19943=DIRECTION('',(1.,0.,0.));
#19944=DIRECTION('center_axis',(0.707106781186543,-0.707106781186553,0.));
#19945=DIRECTION('ref_axis',(0.,0.,-1.));
#19946=DIRECTION('',(0.,0.,1.));
#19947=DIRECTION('center_axis',(0.707106781186543,-0.707106781186553,0.));
#19948=DIRECTION('ref_axis',(0.707106781186553,0.707106781186543,0.));
#19949=DIRECTION('',(0.,0.,-1.));
#19950=DIRECTION('center_axis',(0.707106781186543,-0.707106781186553,0.));
#19951=DIRECTION('ref_axis',(0.707106781186553,0.707106781186543,0.));
#19952=DIRECTION('center_axis',(1.,0.,0.));
#19953=DIRECTION('ref_axis',(0.,0.,-1.));
#19954=DIRECTION('center_axis',(1.,0.,0.));
#19955=DIRECTION('ref_axis',(0.,0.,-1.));
#19956=DIRECTION('center_axis',(0.707106781186543,0.707106781186553,0.));
#19957=DIRECTION('ref_axis',(0.,0.,-1.));
#19958=DIRECTION('',(0.,0.,-1.));
#19959=DIRECTION('center_axis',(0.707106781186543,0.707106781186553,0.));
#19960=DIRECTION('ref_axis',(-0.707106781186553,0.707106781186543,0.));
#19961=DIRECTION('',(0.,0.,1.));
#19962=DIRECTION('center_axis',(0.707106781186543,0.707106781186553,0.));
#19963=DIRECTION('ref_axis',(-0.707106781186553,0.707106781186543,0.));
#19964=DIRECTION('center_axis',(1.,0.,0.));
#19965=DIRECTION('ref_axis',(0.,1.,0.));
#19966=DIRECTION('center_axis',(1.,0.,0.));
#19967=DIRECTION('ref_axis',(0.,0.,-1.));
#19968=DIRECTION('',(-1.,0.,0.));
#19969=DIRECTION('center_axis',(-1.,0.,0.));
#19970=DIRECTION('ref_axis',(0.,1.,0.));
#19971=DIRECTION('',(-1.,0.,0.));
#19972=DIRECTION('center_axis',(-1.,0.,0.));
#19973=DIRECTION('ref_axis',(0.,1.,0.));
#19974=DIRECTION('',(1.,0.,0.));
#19975=DIRECTION('center_axis',(-1.,0.,0.));
#19976=DIRECTION('ref_axis',(0.,1.,0.));
#19977=DIRECTION('',(1.,0.,0.));
#19978=DIRECTION('center_axis',(1.,0.,0.));
#19979=DIRECTION('ref_axis',(0.,0.,-1.));
#19980=DIRECTION('',(-1.,0.,0.));
#19981=DIRECTION('center_axis',(1.,0.,0.));
#19982=DIRECTION('ref_axis',(0.,1.,0.));
#19983=DIRECTION('',(-1.,0.,0.));
#19984=DIRECTION('center_axis',(-1.,0.,0.));
#19985=DIRECTION('ref_axis',(0.,1.,0.));
#19986=DIRECTION('',(-1.,0.,0.));
#19987=DIRECTION('center_axis',(1.,0.,0.));
#19988=DIRECTION('ref_axis',(0.,0.,-1.));
#19989=DIRECTION('center_axis',(-1.,0.,0.));
#19990=DIRECTION('ref_axis',(0.,1.,0.));
#19991=DIRECTION('',(1.,0.,0.));
#19992=DIRECTION('center_axis',(1.,0.,0.));
#19993=DIRECTION('ref_axis',(0.,1.,0.));
#19994=DIRECTION('center_axis',(1.,0.,0.));
#19995=DIRECTION('ref_axis',(0.,0.,-1.));
#19996=DIRECTION('',(-1.,0.,0.));
#19997=DIRECTION('center_axis',(-1.,0.,0.));
#19998=DIRECTION('ref_axis',(0.,1.,0.));
#19999=DIRECTION('',(-1.,0.,0.));
#20000=DIRECTION('center_axis',(-1.,0.,0.));
#20001=DIRECTION('ref_axis',(0.,1.,0.));
#20002=DIRECTION('',(1.,0.,0.));
#20003=DIRECTION('center_axis',(-1.,0.,0.));
#20004=DIRECTION('ref_axis',(0.,1.,0.));
#20005=DIRECTION('',(1.,0.,0.));
#20006=DIRECTION('',(1.,0.,0.));
#20007=DIRECTION('center_axis',(1.,0.,0.));
#20008=DIRECTION('ref_axis',(0.,1.,0.));
#20009=DIRECTION('',(-1.,0.,0.));
#20010=DIRECTION('center_axis',(-1.,0.,0.));
#20011=DIRECTION('ref_axis',(0.,1.,0.));
#20012=DIRECTION('',(1.,0.,0.));
#20013=DIRECTION('center_axis',(1.,0.,0.));
#20014=DIRECTION('ref_axis',(0.,1.,0.));
#20015=DIRECTION('',(-1.,0.,0.));
#20016=DIRECTION('center_axis',(-1.,0.,0.));
#20017=DIRECTION('ref_axis',(0.,1.,0.));
#20018=DIRECTION('',(1.,0.,0.));
#20019=DIRECTION('center_axis',(1.,0.,0.));
#20020=DIRECTION('ref_axis',(0.,1.,0.));
#20021=DIRECTION('',(-1.,0.,0.));
#20022=DIRECTION('center_axis',(-1.,0.,0.));
#20023=DIRECTION('ref_axis',(0.,1.,0.));
#20024=DIRECTION('',(1.,0.,0.));
#20025=DIRECTION('center_axis',(1.,0.,0.));
#20026=DIRECTION('ref_axis',(0.,1.,0.));
#20027=DIRECTION('',(-1.,0.,0.));
#20028=DIRECTION('center_axis',(-1.,0.,0.));
#20029=DIRECTION('ref_axis',(0.,1.,0.));
#20030=DIRECTION('',(1.,0.,0.));
#20031=DIRECTION('center_axis',(1.,0.,0.));
#20032=DIRECTION('ref_axis',(0.,1.,0.));
#20033=DIRECTION('',(-1.,0.,0.));
#20034=DIRECTION('center_axis',(-1.,0.,0.));
#20035=DIRECTION('ref_axis',(0.,1.,0.));
#20036=DIRECTION('',(1.,0.,0.));
#20037=DIRECTION('center_axis',(1.,0.,0.));
#20038=DIRECTION('ref_axis',(0.,1.,0.));
#20039=DIRECTION('',(-1.,0.,0.));
#20040=DIRECTION('center_axis',(-1.,0.,0.));
#20041=DIRECTION('ref_axis',(0.,1.,0.));
#20042=DIRECTION('',(1.,0.,0.));
#20043=DIRECTION('center_axis',(1.,0.,0.));
#20044=DIRECTION('ref_axis',(0.,1.,0.));
#20045=DIRECTION('',(-1.,0.,0.));
#20046=DIRECTION('center_axis',(-1.,0.,0.));
#20047=DIRECTION('ref_axis',(0.,1.,0.));
#20048=DIRECTION('',(1.,0.,0.));
#20049=DIRECTION('center_axis',(1.,0.,0.));
#20050=DIRECTION('ref_axis',(0.,1.,0.));
#20051=DIRECTION('',(-1.,0.,0.));
#20052=DIRECTION('center_axis',(-1.,0.,0.));
#20053=DIRECTION('ref_axis',(0.,1.,0.));
#20054=DIRECTION('',(1.,0.,0.));
#20055=DIRECTION('center_axis',(1.,0.,0.));
#20056=DIRECTION('ref_axis',(0.,1.,0.));
#20057=DIRECTION('',(-1.,0.,0.));
#20058=DIRECTION('center_axis',(-1.,0.,0.));
#20059=DIRECTION('ref_axis',(0.,1.,0.));
#20060=DIRECTION('',(1.,0.,0.));
#20061=DIRECTION('center_axis',(1.,0.,0.));
#20062=DIRECTION('ref_axis',(0.,1.,0.));
#20063=DIRECTION('',(-1.,0.,0.));
#20064=DIRECTION('center_axis',(-1.,0.,0.));
#20065=DIRECTION('ref_axis',(0.,1.,0.));
#20066=DIRECTION('',(1.,0.,0.));
#20067=DIRECTION('center_axis',(1.,0.,0.));
#20068=DIRECTION('ref_axis',(0.,1.,0.));
#20069=DIRECTION('',(-1.,0.,0.));
#20070=DIRECTION('center_axis',(-1.,0.,0.));
#20071=DIRECTION('ref_axis',(0.,1.,0.));
#20072=DIRECTION('',(1.,0.,0.));
#20073=DIRECTION('center_axis',(1.,0.,0.));
#20074=DIRECTION('ref_axis',(0.,1.,0.));
#20075=DIRECTION('',(-1.,0.,0.));
#20076=DIRECTION('center_axis',(-1.,0.,0.));
#20077=DIRECTION('ref_axis',(0.,1.,0.));
#20078=DIRECTION('',(1.,0.,0.));
#20079=DIRECTION('center_axis',(1.,0.,0.));
#20080=DIRECTION('ref_axis',(0.,1.,0.));
#20081=DIRECTION('',(-1.,0.,0.));
#20082=DIRECTION('center_axis',(-1.,0.,0.));
#20083=DIRECTION('ref_axis',(0.,1.,0.));
#20084=DIRECTION('',(1.,0.,0.));
#20085=DIRECTION('center_axis',(1.,0.,0.));
#20086=DIRECTION('ref_axis',(0.,1.,0.));
#20087=DIRECTION('',(-1.,0.,0.));
#20088=DIRECTION('center_axis',(-1.,0.,0.));
#20089=DIRECTION('ref_axis',(0.,1.,0.));
#20090=DIRECTION('',(1.,0.,0.));
#20091=DIRECTION('center_axis',(1.,0.,0.));
#20092=DIRECTION('ref_axis',(0.,1.,0.));
#20093=DIRECTION('',(-1.,0.,0.));
#20094=DIRECTION('center_axis',(-1.,0.,0.));
#20095=DIRECTION('ref_axis',(0.,1.,0.));
#20096=DIRECTION('',(1.,0.,0.));
#20097=DIRECTION('center_axis',(1.,0.,0.));
#20098=DIRECTION('ref_axis',(0.,1.,0.));
#20099=DIRECTION('',(-1.,0.,0.));
#20100=DIRECTION('center_axis',(-1.,0.,0.));
#20101=DIRECTION('ref_axis',(0.,1.,0.));
#20102=DIRECTION('',(1.,0.,0.));
#20103=DIRECTION('center_axis',(1.,0.,0.));
#20104=DIRECTION('ref_axis',(0.,1.,0.));
#20105=DIRECTION('',(-1.,0.,0.));
#20106=DIRECTION('center_axis',(-1.,0.,0.));
#20107=DIRECTION('ref_axis',(0.,1.,0.));
#20108=DIRECTION('',(1.,0.,0.));
#20109=DIRECTION('center_axis',(1.,0.,0.));
#20110=DIRECTION('ref_axis',(0.,1.,0.));
#20111=DIRECTION('',(-1.,0.,0.));
#20112=DIRECTION('center_axis',(-1.,0.,0.));
#20113=DIRECTION('ref_axis',(0.,1.,0.));
#20114=DIRECTION('',(1.,0.,0.));
#20115=DIRECTION('center_axis',(1.,0.,0.));
#20116=DIRECTION('ref_axis',(0.,1.,0.));
#20117=DIRECTION('',(-1.,0.,0.));
#20118=DIRECTION('center_axis',(-1.,0.,0.));
#20119=DIRECTION('ref_axis',(0.,1.,0.));
#20120=DIRECTION('',(1.,0.,0.));
#20121=DIRECTION('center_axis',(1.,0.,0.));
#20122=DIRECTION('ref_axis',(0.,1.,0.));
#20123=DIRECTION('',(-1.,0.,0.));
#20124=DIRECTION('center_axis',(-1.,0.,0.));
#20125=DIRECTION('ref_axis',(0.,1.,0.));
#20126=DIRECTION('',(1.,0.,0.));
#20127=DIRECTION('center_axis',(1.,0.,0.));
#20128=DIRECTION('ref_axis',(0.,1.,0.));
#20129=DIRECTION('',(-1.,0.,0.));
#20130=DIRECTION('center_axis',(-1.,0.,0.));
#20131=DIRECTION('ref_axis',(0.,1.,0.));
#20132=DIRECTION('center_axis',(-1.,0.,0.));
#20133=DIRECTION('ref_axis',(0.,-1.,-1.22464679914735E-16));
#20134=DIRECTION('center_axis',(1.,0.,0.));
#20135=DIRECTION('ref_axis',(0.,0.,-1.));
#20136=DIRECTION('center_axis',(1.,0.,0.));
#20137=DIRECTION('ref_axis',(0.,0.,-1.));
#20138=DIRECTION('center_axis',(1.,0.,0.));
#20139=DIRECTION('ref_axis',(0.,0.,-1.));
#20140=DIRECTION('center_axis',(1.,0.,0.));
#20141=DIRECTION('ref_axis',(0.,1.,0.));
#20142=DIRECTION('center_axis',(1.,0.,0.));
#20143=DIRECTION('ref_axis',(0.,1.,0.));
#20144=DIRECTION('center_axis',(-1.,0.,0.));
#20145=DIRECTION('ref_axis',(0.,1.,7.05550968452284E-14));
#20146=DIRECTION('center_axis',(1.,0.,0.));
#20147=DIRECTION('ref_axis',(0.,0.888987169455759,0.457932104730644));
#20148=DIRECTION('center_axis',(0.,-1.,0.));
#20149=DIRECTION('ref_axis',(0.,0.,1.));
#20150=DIRECTION('',(0.,0.,1.));
#20151=DIRECTION('center_axis',(-1.,0.,0.));
#20152=DIRECTION('ref_axis',(0.,0.,1.));
#20153=DIRECTION('',(0.,0.,-1.));
#20154=DIRECTION('',(0.,0.707106781186547,0.707106781186548));
#20155=DIRECTION('',(0.,0.707106781186547,-0.707106781186548));
#20156=DIRECTION('',(0.,-0.707106781186547,-0.707106781186548));
#20157=DIRECTION('',(0.,-0.707106781186547,0.707106781186548));
#20158=DIRECTION('center_axis',(0.,1.,0.));
#20159=DIRECTION('ref_axis',(0.,0.,-1.));
#20160=DIRECTION('center_axis',(0.,-0.707106781186548,0.707106781186547));
#20161=DIRECTION('ref_axis',(0.,-0.707106781186547,-0.707106781186548));
#20162=DIRECTION('',(0.,-0.707106781186547,-0.707106781186548));
#20163=DIRECTION('',(1.,0.,0.));
#20164=DIRECTION('center_axis',(0.,-0.499999999999999,0.866025403784439));
#20165=DIRECTION('ref_axis',(0.,-0.866025403784439,-0.499999999999999));
#20166=DIRECTION('',(0.,-0.866025403784439,-0.499999999999999));
#20167=DIRECTION('',(1.,0.,0.));
#20168=DIRECTION('',(0.,-0.866025403784439,-0.499999999999999));
#20169=DIRECTION('center_axis',(1.,0.,0.));
#20170=DIRECTION('ref_axis',(0.,-0.258819045102522,-0.965925826289068));
#20171=DIRECTION('',(0.,0.5,-0.866025403784439));
#20172=DIRECTION('center_axis',(0.,-0.866025403784439,-0.5));
#20173=DIRECTION('ref_axis',(0.,0.5,-0.866025403784439));
#20174=DIRECTION('',(0.,0.5,-0.866025403784439));
#20175=DIRECTION('center_axis',(1.,0.,0.));
#20176=DIRECTION('ref_axis',(0.,-0.258819045102522,-0.965925826289068));
#20177=DIRECTION('center_axis',(0.,-0.25881904510252,0.965925826289069));
#20178=DIRECTION('ref_axis',(0.,-0.965925826289069,-0.25881904510252));
#20179=DIRECTION('',(0.,-0.965925826289069,-0.25881904510252));
#20180=DIRECTION('',(1.,0.,0.));
#20181=DIRECTION('',(0.,-0.965925826289069,-0.25881904510252));
#20182=DIRECTION('center_axis',(1.,0.,0.));
#20183=DIRECTION('ref_axis',(0.,-0.5,-0.866025403784438));
#20184=DIRECTION('',(0.,0.258819045102521,-0.965925826289068));
#20185=DIRECTION('center_axis',(0.,-0.965925826289068,-0.258819045102521));
#20186=DIRECTION('ref_axis',(0.,0.258819045102521,-0.965925826289068));
#20187=DIRECTION('',(0.,0.258819045102521,-0.965925826289068));
#20188=DIRECTION('center_axis',(1.,0.,0.));
#20189=DIRECTION('ref_axis',(0.,-0.5,-0.866025403784438));
#20190=DIRECTION('center_axis',(0.,6.66133814775094E-16,1.));
#20191=DIRECTION('ref_axis',(0.,-1.,6.66133814775094E-16));
#20192=DIRECTION('',(0.,-1.,6.66133814775094E-16));
#20193=DIRECTION('',(1.,0.,0.));
#20194=DIRECTION('',(0.,-1.,6.66133814775094E-16));
#20195=DIRECTION('center_axis',(1.,0.,0.));
#20196=DIRECTION('ref_axis',(0.,-0.707106781186548,-0.707106781186547));
#20197=DIRECTION('',(0.,2.22044604925031E-16,-1.));
#20198=DIRECTION('center_axis',(0.,-1.,-2.22044604925031E-16));
#20199=DIRECTION('ref_axis',(0.,2.22044604925031E-16,-1.));
#20200=DIRECTION('',(0.,2.22044604925031E-16,-1.));
#20201=DIRECTION('center_axis',(1.,0.,0.));
#20202=DIRECTION('ref_axis',(0.,-0.707106781186548,-0.707106781186547));
#20203=DIRECTION('center_axis',(0.,0.258819045102522,0.965925826289068));
#20204=DIRECTION('ref_axis',(0.,-0.965925826289068,0.258819045102522));
#20205=DIRECTION('',(0.,-0.965925826289068,0.258819045102522));
#20206=DIRECTION('',(1.,0.,0.));
#20207=DIRECTION('',(0.,-0.965925826289068,0.258819045102522));
#20208=DIRECTION('center_axis',(1.,0.,0.));
#20209=DIRECTION('ref_axis',(0.,-0.866025403784439,-0.499999999999999));
#20210=DIRECTION('',(0.,-0.258819045102521,-0.965925826289068));
#20211=DIRECTION('center_axis',(0.,-0.965925826289068,0.258819045102521));
#20212=DIRECTION('ref_axis',(0.,-0.258819045102521,-0.965925826289068));
#20213=DIRECTION('',(0.,-0.258819045102521,-0.965925826289068));
#20214=DIRECTION('center_axis',(1.,0.,0.));
#20215=DIRECTION('ref_axis',(0.,-0.866025403784439,-0.499999999999999));
#20216=DIRECTION('center_axis',(0.,0.500000000000001,0.866025403784438));
#20217=DIRECTION('ref_axis',(0.,-0.866025403784438,0.500000000000001));
#20218=DIRECTION('',(0.,-0.866025403784438,0.500000000000001));
#20219=DIRECTION('',(1.,0.,0.));
#20220=DIRECTION('',(0.,-0.866025403784438,0.500000000000001));
#20221=DIRECTION('center_axis',(1.,0.,0.));
#20222=DIRECTION('ref_axis',(0.,-0.965925826289068,-0.25881904510252));
#20223=DIRECTION('',(0.,-0.5,-0.866025403784439));
#20224=DIRECTION('center_axis',(0.,-0.866025403784439,0.5));
#20225=DIRECTION('ref_axis',(0.,-0.5,-0.866025403784439));
#20226=DIRECTION('',(0.,-0.5,-0.866025403784439));
#20227=DIRECTION('center_axis',(1.,0.,0.));
#20228=DIRECTION('ref_axis',(0.,-0.965925826289068,-0.25881904510252));
#20229=DIRECTION('center_axis',(0.,0.707106781186548,0.707106781186547));
#20230=DIRECTION('ref_axis',(0.,-0.707106781186547,0.707106781186548));
#20231=DIRECTION('',(0.,-0.707106781186547,0.707106781186548));
#20232=DIRECTION('center_axis',(1.,0.,0.));
#20233=DIRECTION('ref_axis',(0.,-1.,1.83697019872103E-16));
#20234=DIRECTION('center_axis',(0.,0.866025403784439,0.499999999999999));
#20235=DIRECTION('ref_axis',(0.,-0.499999999999999,0.866025403784439));
#20236=DIRECTION('',(0.,-0.499999999999999,0.866025403784439));
#20237=DIRECTION('',(1.,0.,0.));
#20238=DIRECTION('',(0.,-0.499999999999999,0.866025403784439));
#20239=DIRECTION('center_axis',(1.,0.,0.));
#20240=DIRECTION('ref_axis',(0.,-0.965925826289068,0.258819045102522));
#20241=DIRECTION('',(0.,-0.866025403784439,-0.5));
#20242=DIRECTION('center_axis',(0.,-0.5,0.866025403784439));
#20243=DIRECTION('ref_axis',(0.,-0.866025403784439,-0.5));
#20244=DIRECTION('',(0.,-0.866025403784439,-0.5));
#20245=DIRECTION('center_axis',(1.,0.,0.));
#20246=DIRECTION('ref_axis',(0.,-0.965925826289068,0.258819045102522));
#20247=DIRECTION('center_axis',(0.,0.965925826289069,0.25881904510252));
#20248=DIRECTION('ref_axis',(0.,-0.25881904510252,0.965925826289069));
#20249=DIRECTION('',(0.,-0.25881904510252,0.965925826289069));
#20250=DIRECTION('',(1.,0.,0.));
#20251=DIRECTION('',(0.,-0.25881904510252,0.965925826289069));
#20252=DIRECTION('center_axis',(1.,0.,0.));
#20253=DIRECTION('ref_axis',(0.,-0.866025403784438,0.5));
#20254=DIRECTION('',(0.,-0.965925826289068,-0.258819045102521));
#20255=DIRECTION('center_axis',(0.,-0.258819045102521,0.965925826289068));
#20256=DIRECTION('ref_axis',(0.,-0.965925826289068,-0.258819045102521));
#20257=DIRECTION('',(0.,-0.965925826289068,-0.258819045102521));
#20258=DIRECTION('center_axis',(1.,0.,0.));
#20259=DIRECTION('ref_axis',(0.,-0.866025403784438,0.5));
#20260=DIRECTION('center_axis',(0.,1.,-1.0547118733939E-15));
#20261=DIRECTION('ref_axis',(0.,1.0547118733939E-15,1.));
#20262=DIRECTION('',(0.,1.0547118733939E-15,1.));
#20263=DIRECTION('',(1.,0.,0.));
#20264=DIRECTION('',(0.,1.0547118733939E-15,1.));
#20265=DIRECTION('center_axis',(1.,0.,0.));
#20266=DIRECTION('ref_axis',(0.,-0.707106781186547,0.707106781186548));
#20267=DIRECTION('',(0.,-1.,1.11022302462516E-16));
#20268=DIRECTION('center_axis',(0.,1.11022302462516E-16,1.));
#20269=DIRECTION('ref_axis',(0.,-1.,1.11022302462516E-16));
#20270=DIRECTION('',(0.,-1.,1.11022302462516E-16));
#20271=DIRECTION('center_axis',(1.,0.,0.));
#20272=DIRECTION('ref_axis',(0.,-0.707106781186547,0.707106781186548));
#20273=DIRECTION('center_axis',(0.,0.965925826289068,-0.258819045102522));
#20274=DIRECTION('ref_axis',(0.,0.258819045102522,0.965925826289068));
#20275=DIRECTION('',(0.,0.258819045102522,0.965925826289068));
#20276=DIRECTION('',(1.,0.,0.));
#20277=DIRECTION('',(0.,0.258819045102522,0.965925826289068));
#20278=DIRECTION('center_axis',(1.,0.,0.));
#20279=DIRECTION('ref_axis',(0.,-0.5,0.866025403784439));
#20280=DIRECTION('',(0.,-0.965925826289068,0.258819045102521));
#20281=DIRECTION('center_axis',(0.,0.258819045102521,0.965925826289068));
#20282=DIRECTION('ref_axis',(0.,-0.965925826289068,0.258819045102521));
#20283=DIRECTION('',(0.,-0.965925826289068,0.258819045102521));
#20284=DIRECTION('center_axis',(1.,0.,0.));
#20285=DIRECTION('ref_axis',(0.,-0.5,0.866025403784439));
#20286=DIRECTION('center_axis',(0.,0.866025403784438,-0.500000000000001));
#20287=DIRECTION('ref_axis',(0.,0.500000000000001,0.866025403784438));
#20288=DIRECTION('',(0.,0.500000000000001,0.866025403784438));
#20289=DIRECTION('',(1.,0.,0.));
#20290=DIRECTION('',(0.,0.500000000000001,0.866025403784438));
#20291=DIRECTION('center_axis',(1.,0.,0.));
#20292=DIRECTION('ref_axis',(0.,-0.25881904510252,0.965925826289068));
#20293=DIRECTION('',(0.,-0.866025403784439,0.5));
#20294=DIRECTION('center_axis',(0.,0.5,0.866025403784439));
#20295=DIRECTION('ref_axis',(0.,-0.866025403784439,0.5));
#20296=DIRECTION('',(0.,-0.866025403784439,0.5));
#20297=DIRECTION('center_axis',(1.,0.,0.));
#20298=DIRECTION('ref_axis',(0.,-0.25881904510252,0.965925826289068));
#20299=DIRECTION('center_axis',(0.,0.707106781186547,-0.707106781186548));
#20300=DIRECTION('ref_axis',(0.,0.707106781186548,0.707106781186547));
#20301=DIRECTION('',(0.,0.707106781186548,0.707106781186547));
#20302=DIRECTION('',(1.,0.,0.));
#20303=DIRECTION('',(0.,0.707106781186548,0.707106781186547));
#20304=DIRECTION('center_axis',(1.,0.,0.));
#20305=DIRECTION('ref_axis',(0.,1.22464679914735E-16,1.));
#20306=DIRECTION('',(0.,-0.707106781186548,0.707106781186547));
#20307=DIRECTION('center_axis',(0.,0.707106781186547,0.707106781186548));
#20308=DIRECTION('ref_axis',(0.,-0.707106781186548,0.707106781186547));
#20309=DIRECTION('',(0.,-0.707106781186548,0.707106781186547));
#20310=DIRECTION('center_axis',(1.,0.,0.));
#20311=DIRECTION('ref_axis',(0.,1.22464679914735E-16,1.));
#20312=DIRECTION('center_axis',(0.,0.499999999999999,-0.866025403784439));
#20313=DIRECTION('ref_axis',(0.,0.866025403784439,0.499999999999999));
#20314=DIRECTION('',(0.,0.866025403784439,0.499999999999999));
#20315=DIRECTION('',(1.,0.,0.));
#20316=DIRECTION('',(0.,0.866025403784439,0.499999999999999));
#20317=DIRECTION('center_axis',(1.,0.,0.));
#20318=DIRECTION('ref_axis',(0.,0.258819045102521,0.965925826289068));
#20319=DIRECTION('',(0.,-0.5,0.866025403784439));
#20320=DIRECTION('center_axis',(0.,0.866025403784439,0.5));
#20321=DIRECTION('ref_axis',(0.,-0.5,0.866025403784439));
#20322=DIRECTION('',(0.,-0.5,0.866025403784439));
#20323=DIRECTION('center_axis',(1.,0.,0.));
#20324=DIRECTION('ref_axis',(0.,0.258819045102521,0.965925826289068));
#20325=DIRECTION('center_axis',(0.,0.25881904510252,-0.965925826289069));
#20326=DIRECTION('ref_axis',(0.,0.965925826289068,0.25881904510252));
#20327=DIRECTION('',(0.,0.965925826289068,0.25881904510252));
#20328=DIRECTION('',(1.,0.,0.));
#20329=DIRECTION('',(0.,0.965925826289068,0.25881904510252));
#20330=DIRECTION('center_axis',(1.,0.,0.));
#20331=DIRECTION('ref_axis',(0.,0.5,0.866025403784438));
#20332=DIRECTION('',(0.,-0.258819045102521,0.965925826289068));
#20333=DIRECTION('center_axis',(0.,0.965925826289068,0.258819045102521));
#20334=DIRECTION('ref_axis',(0.,-0.258819045102521,0.965925826289068));
#20335=DIRECTION('',(0.,-0.258819045102521,0.965925826289068));
#20336=DIRECTION('center_axis',(1.,0.,0.));
#20337=DIRECTION('ref_axis',(0.,0.5,0.866025403784438));
#20338=DIRECTION('center_axis',(0.,-5.55111512312578E-16,-1.));
#20339=DIRECTION('ref_axis',(0.,1.,-5.55111512312578E-16));
#20340=DIRECTION('',(0.,1.,-5.55111512312578E-16));
#20341=DIRECTION('',(1.,0.,0.));
#20342=DIRECTION('',(0.,1.,-5.55111512312578E-16));
#20343=DIRECTION('center_axis',(1.,0.,0.));
#20344=DIRECTION('ref_axis',(0.,0.707106781186548,0.707106781186547));
#20345=DIRECTION('',(0.,-3.88578058618805E-16,1.));
#20346=DIRECTION('center_axis',(0.,1.,3.88578058618805E-16));
#20347=DIRECTION('ref_axis',(0.,-3.88578058618805E-16,1.));
#20348=DIRECTION('',(0.,-3.88578058618805E-16,1.));
#20349=DIRECTION('center_axis',(1.,0.,0.));
#20350=DIRECTION('ref_axis',(0.,0.707106781186548,0.707106781186547));
#20351=DIRECTION('center_axis',(0.,-0.258819045102522,-0.965925826289068));
#20352=DIRECTION('ref_axis',(0.,0.965925826289068,-0.258819045102522));
#20353=DIRECTION('',(0.,0.965925826289068,-0.258819045102522));
#20354=DIRECTION('',(1.,0.,0.));
#20355=DIRECTION('',(0.,0.965925826289068,-0.258819045102522));
#20356=DIRECTION('center_axis',(1.,0.,0.));
#20357=DIRECTION('ref_axis',(0.,0.866025403784439,0.5));
#20358=DIRECTION('',(0.,0.25881904510252,0.965925826289068));
#20359=DIRECTION('center_axis',(0.,0.965925826289068,-0.258819045102521));
#20360=DIRECTION('ref_axis',(0.,0.25881904510252,0.965925826289068));
#20361=DIRECTION('',(0.,0.25881904510252,0.965925826289068));
#20362=DIRECTION('center_axis',(1.,0.,0.));
#20363=DIRECTION('ref_axis',(0.,0.866025403784439,0.5));
#20364=DIRECTION('center_axis',(0.,-0.500000000000001,-0.866025403784438));
#20365=DIRECTION('ref_axis',(0.,0.866025403784438,-0.500000000000001));
#20366=DIRECTION('',(0.,0.866025403784438,-0.500000000000001));
#20367=DIRECTION('',(1.,0.,0.));
#20368=DIRECTION('',(0.,0.866025403784438,-0.500000000000001));
#20369=DIRECTION('center_axis',(1.,0.,0.));
#20370=DIRECTION('ref_axis',(0.,0.965925826289068,0.258819045102521));
#20371=DIRECTION('',(0.,0.5,0.866025403784439));
#20372=DIRECTION('center_axis',(0.,0.866025403784439,-0.5));
#20373=DIRECTION('ref_axis',(0.,0.5,0.866025403784439));
#20374=DIRECTION('',(0.,0.5,0.866025403784439));
#20375=DIRECTION('center_axis',(1.,0.,0.));
#20376=DIRECTION('ref_axis',(0.,0.965925826289068,0.258819045102521));
#20377=DIRECTION('center_axis',(0.,-0.707106781186548,-0.707106781186547));
#20378=DIRECTION('ref_axis',(0.,0.707106781186547,-0.707106781186548));
#20379=DIRECTION('',(1.,0.,0.));
#20380=DIRECTION('',(0.,0.707106781186547,-0.707106781186548));
#20381=DIRECTION('center_axis',(1.,0.,0.));
#20382=DIRECTION('ref_axis',(0.,1.,-6.12323399573677E-17));
#20383=DIRECTION('',(0.,0.707106781186547,0.707106781186548));
#20384=DIRECTION('center_axis',(0.,0.707106781186548,-0.707106781186547));
#20385=DIRECTION('ref_axis',(0.,0.707106781186547,0.707106781186548));
#20386=DIRECTION('center_axis',(0.,-0.866025403784439,-0.499999999999999));
#20387=DIRECTION('ref_axis',(0.,0.499999999999999,-0.866025403784439));
#20388=DIRECTION('',(0.,0.499999999999999,-0.866025403784439));
#20389=DIRECTION('',(1.,0.,0.));
#20390=DIRECTION('',(0.,0.499999999999999,-0.866025403784439));
#20391=DIRECTION('center_axis',(1.,0.,0.));
#20392=DIRECTION('ref_axis',(0.,0.965925826289068,-0.258819045102521));
#20393=DIRECTION('',(0.,0.866025403784439,0.5));
#20394=DIRECTION('center_axis',(0.,0.5,-0.866025403784439));
#20395=DIRECTION('ref_axis',(0.,0.866025403784439,0.5));
#20396=DIRECTION('',(0.,0.866025403784439,0.5));
#20397=DIRECTION('center_axis',(1.,0.,0.));
#20398=DIRECTION('ref_axis',(0.,0.965925826289068,-0.258819045102521));
#20399=DIRECTION('center_axis',(0.,-0.965925826289068,-0.25881904510252));
#20400=DIRECTION('ref_axis',(0.,0.25881904510252,-0.965925826289068));
#20401=DIRECTION('',(0.,0.25881904510252,-0.965925826289068));
#20402=DIRECTION('',(1.,0.,0.));
#20403=DIRECTION('',(0.,0.25881904510252,-0.965925826289068));
#20404=DIRECTION('center_axis',(1.,0.,0.));
#20405=DIRECTION('ref_axis',(0.,0.866025403784439,-0.5));
#20406=DIRECTION('',(0.,0.965925826289068,0.258819045102521));
#20407=DIRECTION('center_axis',(0.,0.258819045102521,-0.965925826289068));
#20408=DIRECTION('ref_axis',(0.,0.965925826289068,0.258819045102521));
#20409=DIRECTION('',(0.,0.965925826289068,0.258819045102521));
#20410=DIRECTION('center_axis',(1.,0.,0.));
#20411=DIRECTION('ref_axis',(0.,0.866025403784439,-0.5));
#20412=DIRECTION('center_axis',(0.,-1.,4.9960036108132E-16));
#20413=DIRECTION('ref_axis',(0.,-4.9960036108132E-16,-1.));
#20414=DIRECTION('',(0.,-4.9960036108132E-16,-1.));
#20415=DIRECTION('',(1.,0.,0.));
#20416=DIRECTION('',(0.,-4.9960036108132E-16,-1.));
#20417=DIRECTION('center_axis',(1.,0.,0.));
#20418=DIRECTION('ref_axis',(0.,0.707106781186548,-0.707106781186548));
#20419=DIRECTION('',(0.,1.,4.9960036108132E-16));
#20420=DIRECTION('center_axis',(0.,4.9960036108132E-16,-1.));
#20421=DIRECTION('ref_axis',(0.,1.,4.9960036108132E-16));
#20422=DIRECTION('',(0.,1.,4.9960036108132E-16));
#20423=DIRECTION('center_axis',(1.,0.,0.));
#20424=DIRECTION('ref_axis',(0.,0.707106781186548,-0.707106781186548));
#20425=DIRECTION('center_axis',(0.,-0.965925826289068,0.258819045102521));
#20426=DIRECTION('ref_axis',(0.,-0.258819045102521,-0.965925826289068));
#20427=DIRECTION('',(0.,-0.258819045102521,-0.965925826289068));
#20428=DIRECTION('',(1.,0.,0.));
#20429=DIRECTION('',(0.,-0.258819045102521,-0.965925826289068));
#20430=DIRECTION('center_axis',(1.,0.,0.));
#20431=DIRECTION('ref_axis',(0.,0.5,-0.866025403784439));
#20432=DIRECTION('',(0.,0.965925826289068,-0.25881904510252));
#20433=DIRECTION('center_axis',(0.,-0.25881904510252,-0.965925826289068));
#20434=DIRECTION('ref_axis',(0.,0.965925826289068,-0.25881904510252));
#20435=DIRECTION('',(0.,0.965925826289068,-0.25881904510252));
#20436=DIRECTION('center_axis',(1.,0.,0.));
#20437=DIRECTION('ref_axis',(0.,0.5,-0.866025403784439));
#20438=DIRECTION('center_axis',(0.,-0.866025403784438,0.5));
#20439=DIRECTION('ref_axis',(0.,-0.5,-0.866025403784438));
#20440=DIRECTION('',(0.,-0.5,-0.866025403784438));
#20441=DIRECTION('',(1.,0.,0.));
#20442=DIRECTION('',(0.,-0.5,-0.866025403784438));
#20443=DIRECTION('center_axis',(1.,0.,0.));
#20444=DIRECTION('ref_axis',(0.,0.258819045102521,-0.965925826289068));
#20445=DIRECTION('',(0.,0.866025403784439,-0.5));
#20446=DIRECTION('center_axis',(0.,-0.5,-0.866025403784439));
#20447=DIRECTION('ref_axis',(0.,0.866025403784439,-0.5));
#20448=DIRECTION('',(0.,0.866025403784439,-0.5));
#20449=DIRECTION('center_axis',(1.,0.,0.));
#20450=DIRECTION('ref_axis',(0.,0.258819045102521,-0.965925826289068));
#20451=DIRECTION('center_axis',(0.,-0.707106781186547,0.707106781186548));
#20452=DIRECTION('ref_axis',(0.,-0.707106781186548,-0.707106781186547));
#20453=DIRECTION('',(0.,-0.707106781186548,-0.707106781186547));
#20454=DIRECTION('',(1.,0.,0.));
#20455=DIRECTION('',(0.,-0.707106781186548,-0.707106781186547));
#20456=DIRECTION('center_axis',(1.,0.,0.));
#20457=DIRECTION('ref_axis',(0.,0.,-1.));
#20458=DIRECTION('',(0.,0.707106781186548,-0.707106781186547));
#20459=DIRECTION('center_axis',(0.,-0.707106781186547,-0.707106781186548));
#20460=DIRECTION('ref_axis',(0.,0.707106781186548,-0.707106781186547));
#20461=DIRECTION('',(0.,0.707106781186548,-0.707106781186547));
#20462=DIRECTION('center_axis',(1.,0.,0.));
#20463=DIRECTION('ref_axis',(0.,0.,-1.));
#20464=DIRECTION('center_axis',(-1.,0.,0.));
#20465=DIRECTION('ref_axis',(0.,0.,1.));
#20466=DIRECTION('center_axis',(1.,0.,0.));
#20467=DIRECTION('ref_axis',(0.,0.,-1.));
#20468=DIRECTION('center_axis',(1.,0.,0.));
#20469=DIRECTION('ref_axis',(0.,1.,0.));
#20470=DIRECTION('',(-0.707106781186571,0.707106781186524,8.65956056235465E-17));
#20471=DIRECTION('center_axis',(1.,0.,0.));
#20472=DIRECTION('ref_axis',(0.,1.,0.));
#20473=DIRECTION('center_axis',(1.,0.,0.));
#20474=DIRECTION('ref_axis',(0.,1.,0.));
#20475=DIRECTION('center_axis',(-1.,0.,0.));
#20476=DIRECTION('ref_axis',(0.,0.,1.));
#20477=DIRECTION('center_axis',(1.,0.,0.));
#20478=DIRECTION('ref_axis',(0.,0.,-1.));
#20479=DIRECTION('center_axis',(1.,0.,0.));
#20480=DIRECTION('ref_axis',(0.,1.,0.));
#20481=DIRECTION('',(-0.707106781186571,0.707106781186524,8.65956056235465E-17));
#20482=DIRECTION('center_axis',(-1.,0.,0.));
#20483=DIRECTION('ref_axis',(0.,1.,0.));
#20484=DIRECTION('axis',(0.,0.,1.));
#20485=DIRECTION('refdir',(1.,0.,0.));
#20486=DIRECTION('center_axis',(-1.,0.,0.));
#20487=DIRECTION('ref_axis',(0.,-1.,0.));
#20488=DIRECTION('center_axis',(-1.,0.,0.));
#20489=DIRECTION('ref_axis',(0.,-1.,0.));
#20490=DIRECTION('',(0.707106781186552,-0.707106781186543,8.65956056235488E-17));
#20491=DIRECTION('center_axis',(1.,0.,0.));
#20492=DIRECTION('ref_axis',(0.,-1.,0.));
#20493=DIRECTION('center_axis',(1.,0.,0.));
#20494=DIRECTION('ref_axis',(0.,-1.,0.));
#20495=DIRECTION('center_axis',(1.,0.,0.));
#20496=DIRECTION('ref_axis',(0.,1.,0.));
#20497=DIRECTION('center_axis',(1.,0.,0.));
#20498=DIRECTION('ref_axis',(0.,0.,-1.));
#20499=DIRECTION('',(-1.,0.,0.));
#20500=DIRECTION('center_axis',(-1.,0.,0.));
#20501=DIRECTION('ref_axis',(0.,0.,1.));
#20502=DIRECTION('center_axis',(1.,0.,0.));
#20503=DIRECTION('ref_axis',(0.,0.,-1.));
#20504=DIRECTION('center_axis',(1.,0.,0.));
#20505=DIRECTION('ref_axis',(0.,1.,0.));
#20506=DIRECTION('',(-1.,0.,0.));
#20507=DIRECTION('center_axis',(1.,0.,0.));
#20508=DIRECTION('ref_axis',(0.,0.,-1.));
#20509=DIRECTION('center_axis',(-1.,0.,0.));
#20510=DIRECTION('ref_axis',(0.,0.,1.));
#20511=DIRECTION('center_axis',(1.,0.,0.));
#20512=DIRECTION('ref_axis',(0.,0.,-1.));
#20513=DIRECTION('center_axis',(1.,0.,0.));
#20514=DIRECTION('ref_axis',(0.,1.,0.));
#20515=DIRECTION('center_axis',(1.,0.,0.));
#20516=DIRECTION('ref_axis',(0.,0.,-1.));
#20517=DIRECTION('',(-0.70710678118654,0.707106781186555,8.65956056235503E-17));
#20518=DIRECTION('center_axis',(1.,0.,0.));
#20519=DIRECTION('ref_axis',(0.,1.,0.));
#20520=DIRECTION('center_axis',(1.,0.,0.));
#20521=DIRECTION('ref_axis',(0.,0.,-1.));
#20522=DIRECTION('',(-1.,0.,0.));
#20523=DIRECTION('center_axis',(-1.,0.,0.));
#20524=DIRECTION('ref_axis',(0.,1.,0.));
#20525=DIRECTION('center_axis',(1.,0.,0.));
#20526=DIRECTION('ref_axis',(0.,0.,-1.));
#20527=DIRECTION('',(-0.707106781186548,-0.707106781186547,-8.65956056235492E-17));
#20528=DIRECTION('center_axis',(1.,0.,0.));
#20529=DIRECTION('ref_axis',(0.,0.,-1.));
#20530=DIRECTION('center_axis',(-1.,0.,0.));
#20531=DIRECTION('ref_axis',(0.,0.,1.));
#20532=DIRECTION('axis',(0.,0.,1.));
#20533=DIRECTION('refdir',(1.,0.,0.));
#20534=DIRECTION('center_axis',(-1.,0.,-3.28183559150414E-15));
#20535=DIRECTION('ref_axis',(0.,-1.,-3.24835777379068E-17));
#20536=DIRECTION('center_axis',(-1.,0.,0.));
#20537=DIRECTION('ref_axis',(0.,-1.,0.));
#20538=DIRECTION('',(-0.16018224300698,0.987087457637495,-3.72744304515565E-16));
#20539=DIRECTION('center_axis',(1.,0.,0.));
#20540=DIRECTION('ref_axis',(0.,-1.,-6.12323399573677E-17));
#20541=DIRECTION('center_axis',(1.,0.,0.));
#20542=DIRECTION('ref_axis',(0.,-1.,-6.12323399573677E-17));
#20543=DIRECTION('center_axis',(-1.,0.,0.));
#20544=DIRECTION('ref_axis',(0.,1.,0.));
#20545=DIRECTION('',(-0.316227766016835,-0.948683298050515,-1.16180196436212E-16));
#20546=DIRECTION('center_axis',(-1.,0.,0.));
#20547=DIRECTION('ref_axis',(0.,-1.,-6.12323399573676E-17));
#20548=DIRECTION('center_axis',(-1.,0.,0.));
#20549=DIRECTION('ref_axis',(0.,-1.,-6.12323399573676E-17));
#20550=DIRECTION('center_axis',(1.,0.,0.));
#20551=DIRECTION('ref_axis',(0.,0.,-1.));
#20552=DIRECTION('center_axis',(-1.,0.,-8.29060943031117E-17));
#20553=DIRECTION('ref_axis',(0.,-1.,-6.12323399573677E-17));
#20554=DIRECTION('',(-0.594101906730864,0.804389783885121,9.85093374101743E-17));
#20555=DIRECTION('center_axis',(1.,0.,0.));
#20556=DIRECTION('ref_axis',(0.,-1.,-6.12323399573677E-17));
#20557=DIRECTION('center_axis',(1.,0.,0.));
#20558=DIRECTION('ref_axis',(0.,-1.,-6.12323399573677E-17));
#20559=DIRECTION('center_axis',(-1.,0.,0.));
#20560=DIRECTION('ref_axis',(0.,1.,0.));
#20561=DIRECTION('',(-0.813733471206736,-0.581238193719095,-7.11811493480279E-17));
#20562=DIRECTION('center_axis',(-1.,0.,0.));
#20563=DIRECTION('ref_axis',(0.,-1.,-6.12323399573677E-17));
#20564=DIRECTION('center_axis',(-1.,0.,0.));
#20565=DIRECTION('ref_axis',(0.,-1.,-6.12323399573677E-17));
#20566=DIRECTION('center_axis',(-1.,0.,9.93188719646043E-16));
#20567=DIRECTION('ref_axis',(0.,-1.,-3.03166806120925E-17));
#20568=DIRECTION('',(-0.952295508549404,0.305177431007982,9.92434579972342E-16));
#20569=DIRECTION('center_axis',(1.,0.,0.));
#20570=DIRECTION('ref_axis',(0.,-1.,0.));
#20571=DIRECTION('center_axis',(1.,0.,0.));
#20572=DIRECTION('ref_axis',(0.,-1.,0.));
#20573=DIRECTION('center_axis',(1.,0.,0.));
#20574=DIRECTION('ref_axis',(0.,1.,0.));
#20575=DIRECTION('',(-1.,0.,0.));
#20576=DIRECTION('center_axis',(1.,0.,0.));
#20577=DIRECTION('ref_axis',(0.,0.,-1.));
#20578=DIRECTION('center_axis',(1.,0.,0.));
#20579=DIRECTION('ref_axis',(0.,1.,0.));
#20580=DIRECTION('center_axis',(1.,0.,0.));
#20581=DIRECTION('ref_axis',(0.,0.,-1.));
#20582=DIRECTION('',(-1.,0.,0.));
#20583=DIRECTION('center_axis',(1.,0.,0.));
#20584=DIRECTION('ref_axis',(0.,0.,-1.));
#20585=DIRECTION('center_axis',(-1.,0.,0.));
#20586=DIRECTION('ref_axis',(0.,0.,1.));
#20587=DIRECTION('center_axis',(1.,0.,0.));
#20588=DIRECTION('ref_axis',(0.,0.,-1.));
#20589=DIRECTION('center_axis',(1.,0.,0.));
#20590=DIRECTION('ref_axis',(0.,1.,0.));
#20591=DIRECTION('',(-0.707106781186532,0.707106781186563,8.65956056235512E-17));
#20592=DIRECTION('center_axis',(-1.,0.,0.));
#20593=DIRECTION('ref_axis',(0.,0.,1.));
#20594=DIRECTION('center_axis',(1.,0.,0.));
#20595=DIRECTION('ref_axis',(0.,0.,-1.));
#20596=DIRECTION('center_axis',(-1.,0.,0.));
#20597=DIRECTION('ref_axis',(0.,1.,0.));
#20598=DIRECTION('',(-0.707106781186548,-0.707106781186547,-8.65956056235492E-17));
#20599=DIRECTION('axis',(0.,0.,1.));
#20600=DIRECTION('refdir',(1.,0.,0.));
#20601=DIRECTION('center_axis',(1.,0.,0.));
#20602=DIRECTION('ref_axis',(0.,1.,0.));
#20603=DIRECTION('',(-1.,0.,0.));
#20604=DIRECTION('center_axis',(1.,0.,0.));
#20605=DIRECTION('ref_axis',(0.,1.,0.));
#20606=DIRECTION('center_axis',(1.,0.,0.));
#20607=DIRECTION('ref_axis',(0.,1.,0.));
#20608=DIRECTION('',(-1.,0.,0.));
#20609=DIRECTION('center_axis',(1.,0.,0.));
#20610=DIRECTION('ref_axis',(0.,1.,0.));
#20611=DIRECTION('',(-1.,0.,0.));
#20612=DIRECTION('center_axis',(1.,0.,0.));
#20613=DIRECTION('ref_axis',(0.,1.,0.));
#20614=DIRECTION('',(-1.,0.,0.));
#20615=DIRECTION('center_axis',(1.,0.,0.));
#20616=DIRECTION('ref_axis',(0.,1.,0.));
#20617=DIRECTION('',(-1.,0.,0.));
#20618=DIRECTION('center_axis',(1.,0.,0.));
#20619=DIRECTION('ref_axis',(0.,1.,0.));
#20620=DIRECTION('',(-1.,0.,0.));
#20621=DIRECTION('center_axis',(1.,0.,0.));
#20622=DIRECTION('ref_axis',(0.,1.,0.));
#20623=DIRECTION('',(-1.,0.,0.));
#20624=DIRECTION('center_axis',(1.,0.,0.));
#20625=DIRECTION('ref_axis',(0.,1.,0.));
#20626=DIRECTION('',(-1.,0.,0.));
#20627=DIRECTION('center_axis',(1.,0.,0.));
#20628=DIRECTION('ref_axis',(0.,1.,0.));
#20629=DIRECTION('',(-1.,0.,0.));
#20630=DIRECTION('center_axis',(1.,0.,0.));
#20631=DIRECTION('ref_axis',(0.,1.,0.));
#20632=DIRECTION('',(-1.,0.,0.));
#20633=DIRECTION('center_axis',(1.,0.,0.));
#20634=DIRECTION('ref_axis',(0.,1.,0.));
#20635=DIRECTION('',(-1.,0.,0.));
#20636=DIRECTION('center_axis',(1.,0.,0.));
#20637=DIRECTION('ref_axis',(0.,1.,0.));
#20638=DIRECTION('',(-1.,0.,0.));
#20639=DIRECTION('center_axis',(1.,0.,0.));
#20640=DIRECTION('ref_axis',(0.,1.,0.));
#20641=DIRECTION('',(-1.,0.,0.));
#20642=DIRECTION('center_axis',(1.,0.,0.));
#20643=DIRECTION('ref_axis',(0.,0.957230166128618,-0.289327511746427));
#20644=DIRECTION('',(1.,0.,0.));
#20645=DIRECTION('center_axis',(1.,0.,0.));
#20646=DIRECTION('ref_axis',(0.,1.,6.85471472797398E-14));
#20647=DIRECTION('center_axis',(1.,0.,0.));
#20648=DIRECTION('ref_axis',(0.,1.,6.85471472797398E-14));
#20649=DIRECTION('',(1.,0.,0.));
#20650=DIRECTION('center_axis',(1.,0.,0.));
#20651=DIRECTION('ref_axis',(0.,1.,6.85471472797398E-14));
#20652=DIRECTION('',(1.,0.,0.));
#20653=DIRECTION('center_axis',(1.,0.,0.));
#20654=DIRECTION('ref_axis',(0.,1.,6.85471472797398E-14));
#20655=DIRECTION('',(1.,0.,0.));
#20656=DIRECTION('center_axis',(1.,0.,0.));
#20657=DIRECTION('ref_axis',(0.,1.,6.85471472797398E-14));
#20658=DIRECTION('',(1.,0.,0.));
#20659=DIRECTION('center_axis',(1.,0.,0.));
#20660=DIRECTION('ref_axis',(0.,1.,6.85471472797398E-14));
#20661=DIRECTION('',(1.,0.,0.));
#20662=DIRECTION('center_axis',(1.,0.,0.));
#20663=DIRECTION('ref_axis',(0.,1.,6.85471472797398E-14));
#20664=DIRECTION('',(1.,0.,0.));
#20665=DIRECTION('center_axis',(1.,0.,0.));
#20666=DIRECTION('ref_axis',(0.,1.,6.85471472797398E-14));
#20667=DIRECTION('',(1.,0.,0.));
#20668=DIRECTION('center_axis',(1.,0.,0.));
#20669=DIRECTION('ref_axis',(0.,1.,6.85471472797398E-14));
#20670=DIRECTION('',(1.,0.,0.));
#20671=DIRECTION('center_axis',(1.,0.,0.));
#20672=DIRECTION('ref_axis',(0.,1.,6.85471472797398E-14));
#20673=DIRECTION('',(1.,0.,0.));
#20674=DIRECTION('center_axis',(1.,0.,0.));
#20675=DIRECTION('ref_axis',(0.,1.,6.85471472797398E-14));
#20676=DIRECTION('',(1.,0.,0.));
#20677=DIRECTION('center_axis',(1.,0.,0.));
#20678=DIRECTION('ref_axis',(0.,1.,6.85471472797398E-14));
#20679=DIRECTION('',(1.,0.,0.));
#20680=DIRECTION('center_axis',(1.,0.,0.));
#20681=DIRECTION('ref_axis',(0.,0.,-1.));
#20682=DIRECTION('center_axis',(1.,0.,0.));
#20683=DIRECTION('ref_axis',(0.,1.,0.));
#20684=DIRECTION('center_axis',(1.,0.,0.));
#20685=DIRECTION('ref_axis',(0.,1.,0.));
#20686=DIRECTION('center_axis',(-1.,0.,0.));
#20687=DIRECTION('ref_axis',(0.,1.,6.85471472797398E-14));
#20688=DIRECTION('center_axis',(1.,0.,0.));
#20689=DIRECTION('ref_axis',(0.,1.,6.85471472797398E-14));
#20690=DIRECTION('center_axis',(1.,0.,0.));
#20691=DIRECTION('ref_axis',(0.,0.,-1.));
#20692=DIRECTION('center_axis',(-1.,0.,0.));
#20693=DIRECTION('ref_axis',(0.,1.,0.));
#20694=DIRECTION('center_axis',(1.,0.,0.));
#20695=DIRECTION('ref_axis',(0.,0.,-1.));
#20696=DIRECTION('',(-1.,0.,0.));
#20697=DIRECTION('',(-1.,0.,0.));
#20698=DIRECTION('',(-1.,0.,0.));
#20699=DIRECTION('',(-1.,0.,0.));
#20700=DIRECTION('',(-1.,0.,0.));
#20701=DIRECTION('',(-1.,0.,0.));
#20702=DIRECTION('',(-1.,0.,0.));
#20703=DIRECTION('',(-1.,0.,0.));
#20704=DIRECTION('',(-1.,0.,0.));
#20705=DIRECTION('',(-1.,0.,0.));
#20706=DIRECTION('',(-1.,0.,0.));
#20707=DIRECTION('center_axis',(1.,0.,0.));
#20708=DIRECTION('ref_axis',(0.,0.,-1.));
#20709=DIRECTION('center_axis',(0.,0.427000673777987,0.904251306105302));
#20710=DIRECTION('ref_axis',(0.,0.904251306105302,-0.427000673777987));
#20711=DIRECTION('',(0.,0.904251306105302,-0.427000673777987));
#20712=DIRECTION('',(-1.,0.,0.));
#20713=DIRECTION('',(0.,0.904251306105302,-0.427000673777987));
#20714=DIRECTION('',(-1.,0.,0.));
#20715=DIRECTION('center_axis',(0.,-0.514495755427527,0.857492925712544));
#20716=DIRECTION('ref_axis',(0.,0.857492925712544,0.514495755427527));
#20717=DIRECTION('',(0.,0.857492925712544,0.514495755427527));
#20718=DIRECTION('',(-1.,0.,0.));
#20719=DIRECTION('',(0.,0.857492925712544,0.514495755427527));
#20720=DIRECTION('center_axis',(0.,-0.857492925712544,-0.514495755427526));
#20721=DIRECTION('ref_axis',(0.,-0.514495755427526,0.857492925712544));
#20722=DIRECTION('',(0.,-0.514495755427526,0.857492925712544));
#20723=DIRECTION('',(-1.,0.,0.));
#20724=DIRECTION('',(0.,-0.514495755427526,0.857492925712544));
#20725=DIRECTION('center_axis',(0.,0.514495755427526,-0.857492925712544));
#20726=DIRECTION('ref_axis',(0.,-0.857492925712544,-0.514495755427526));
#20727=DIRECTION('',(0.,-0.857492925712544,-0.514495755427526));
#20728=DIRECTION('',(-1.,0.,0.));
#20729=DIRECTION('',(0.,-0.857492925712544,-0.514495755427526));
#20730=DIRECTION('center_axis',(0.,0.857492925712544,0.514495755427527));
#20731=DIRECTION('ref_axis',(0.,0.514495755427527,-0.857492925712544));
#20732=DIRECTION('',(0.,0.514495755427527,-0.857492925712544));
#20733=DIRECTION('',(-1.,0.,0.));
#20734=DIRECTION('',(0.,0.514495755427527,-0.857492925712544));
#20735=DIRECTION('center_axis',(0.,-0.426637779431547,-0.904422581076854));
#20736=DIRECTION('ref_axis',(0.,-0.904422581076854,0.426637779431547));
#20737=DIRECTION('',(0.,-0.904422581076854,0.426637779431547));
#20738=DIRECTION('',(-1.,0.,0.));
#20739=DIRECTION('',(0.,-0.904422581076854,0.426637779431547));
#20740=DIRECTION('center_axis',(0.,0.51449575542753,-0.857492925712542));
#20741=DIRECTION('ref_axis',(0.,-0.857492925712542,-0.51449575542753));
#20742=DIRECTION('',(0.,-0.857492925712542,-0.51449575542753));
#20743=DIRECTION('',(-1.,0.,0.));
#20744=DIRECTION('',(0.,-0.857492925712542,-0.51449575542753));
#20745=DIRECTION('center_axis',(0.,0.857492925712544,0.514495755427527));
#20746=DIRECTION('ref_axis',(0.,0.514495755427527,-0.857492925712544));
#20747=DIRECTION('',(0.,0.514495755427527,-0.857492925712544));
#20748=DIRECTION('',(-1.,0.,0.));
#20749=DIRECTION('',(0.,0.514495755427527,-0.857492925712544));
#20750=DIRECTION('center_axis',(0.,-0.514495755427528,0.857492925712544));
#20751=DIRECTION('ref_axis',(0.,0.857492925712543,0.514495755427528));
#20752=DIRECTION('',(0.,0.857492925712543,0.514495755427528));
#20753=DIRECTION('',(-1.,0.,0.));
#20754=DIRECTION('',(0.,0.857492925712543,0.514495755427528));
#20755=DIRECTION('center_axis',(0.,-0.857492925712544,-0.514495755427527));
#20756=DIRECTION('ref_axis',(0.,-0.514495755427527,0.857492925712544));
#20757=DIRECTION('',(0.,-0.514495755427527,0.857492925712544));
#20758=DIRECTION('',(0.,-0.514495755427527,0.857492925712544));
#20759=DIRECTION('center_axis',(-1.,0.,0.));
#20760=DIRECTION('ref_axis',(0.,0.,1.));
#20761=DIRECTION('',(-1.,0.,0.));
#20762=DIRECTION('',(-1.,0.,0.));
#20763=DIRECTION('',(-1.,0.,0.));
#20764=DIRECTION('',(-1.,0.,0.));
#20765=DIRECTION('',(-1.,0.,0.));
#20766=DIRECTION('',(-1.,0.,0.));
#20767=DIRECTION('',(-1.,0.,0.));
#20768=DIRECTION('',(-1.,0.,0.));
#20769=DIRECTION('',(-1.,0.,0.));
#20770=DIRECTION('',(-1.,0.,0.));
#20771=DIRECTION('',(-1.,0.,0.));
#20772=DIRECTION('center_axis',(1.,0.,0.));
#20773=DIRECTION('ref_axis',(0.,0.,-1.));
#20774=DIRECTION('center_axis',(0.,-0.447213595499958,-0.894427190999916));
#20775=DIRECTION('ref_axis',(0.,-0.894427190999916,0.447213595499958));
#20776=DIRECTION('',(0.,-0.894427190999916,0.447213595499958));
#20777=DIRECTION('',(-1.,0.,0.));
#20778=DIRECTION('',(0.,-0.894427190999916,0.447213595499958));
#20779=DIRECTION('',(-1.,0.,0.));
#20780=DIRECTION('center_axis',(0.,0.894427190999917,-0.447213595499956));
#20781=DIRECTION('ref_axis',(0.,-0.447213595499956,-0.894427190999917));
#20782=DIRECTION('',(0.,-0.447213595499956,-0.894427190999917));
#20783=DIRECTION('',(-1.,0.,0.));
#20784=DIRECTION('',(0.,-0.447213595499956,-0.894427190999917));
#20785=DIRECTION('center_axis',(0.,0.447213595499957,0.894427190999916));
#20786=DIRECTION('ref_axis',(0.,0.894427190999916,-0.447213595499957));
#20787=DIRECTION('',(0.,0.894427190999916,-0.447213595499957));
#20788=DIRECTION('',(-1.,0.,0.));
#20789=DIRECTION('',(0.,0.894427190999916,-0.447213595499957));
#20790=DIRECTION('center_axis',(0.,0.894427190999916,-0.447213595499958));
#20791=DIRECTION('ref_axis',(0.,-0.447213595499958,-0.894427190999916));
#20792=DIRECTION('',(0.,-0.447213595499958,-0.894427190999916));
#20793=DIRECTION('',(-1.,0.,0.));
#20794=DIRECTION('',(0.,-0.447213595499958,-0.894427190999916));
#20795=DIRECTION('center_axis',(0.,-0.447213595499958,-0.894427190999916));
#20796=DIRECTION('ref_axis',(0.,-0.894427190999916,0.447213595499958));
#20797=DIRECTION('',(0.,-0.894427190999916,0.447213595499958));
#20798=DIRECTION('',(-1.,0.,0.));
#20799=DIRECTION('',(0.,-0.894427190999916,0.447213595499958));
#20800=DIRECTION('center_axis',(0.,0.894427190999917,-0.447213595499956));
#20801=DIRECTION('ref_axis',(0.,-0.447213595499956,-0.894427190999917));
#20802=DIRECTION('',(0.,-0.447213595499956,-0.894427190999917));
#20803=DIRECTION('',(-1.,0.,0.));
#20804=DIRECTION('',(0.,-0.447213595499956,-0.894427190999917));
#20805=DIRECTION('center_axis',(0.,0.447213595499958,0.894427190999916));
#20806=DIRECTION('ref_axis',(0.,0.894427190999916,-0.447213595499958));
#20807=DIRECTION('',(0.,0.894427190999916,-0.447213595499958));
#20808=DIRECTION('',(-1.,0.,0.));
#20809=DIRECTION('',(0.,0.894427190999916,-0.447213595499958));
#20810=DIRECTION('center_axis',(0.,-0.894427190999916,0.447213595499958));
#20811=DIRECTION('ref_axis',(0.,0.447213595499958,0.894427190999916));
#20812=DIRECTION('',(0.,0.447213595499958,0.894427190999916));
#20813=DIRECTION('',(-1.,0.,0.));
#20814=DIRECTION('',(0.,0.447213595499958,0.894427190999916));
#20815=DIRECTION('center_axis',(0.,-0.447213595499959,-0.894427190999915));
#20816=DIRECTION('ref_axis',(0.,-0.894427190999915,0.447213595499959));
#20817=DIRECTION('',(0.,-0.894427190999915,0.447213595499959));
#20818=DIRECTION('',(-1.,0.,0.));
#20819=DIRECTION('',(0.,-0.894427190999915,0.447213595499959));
#20820=DIRECTION('center_axis',(0.,0.894427190999916,-0.447213595499958));
#20821=DIRECTION('ref_axis',(0.,-0.447213595499958,-0.894427190999916));
#20822=DIRECTION('',(0.,-0.447213595499958,-0.894427190999916));
#20823=DIRECTION('',(0.,-0.447213595499958,-0.894427190999916));
#20824=DIRECTION('center_axis',(-1.,0.,0.));
#20825=DIRECTION('ref_axis',(0.,0.,1.));
#20826=DIRECTION('center_axis',(0.,-0.447213595499958,-0.894427190999916));
#20827=DIRECTION('ref_axis',(0.,-0.894427190999916,0.447213595499958));
#20828=DIRECTION('',(0.,-0.894427190999916,0.447213595499958));
#20829=DIRECTION('',(-1.,0.,0.));
#20830=DIRECTION('',(0.,-0.894427190999916,0.447213595499958));
#20831=DIRECTION('',(-1.,0.,0.));
#20832=DIRECTION('center_axis',(0.,0.894427190999917,-0.447213595499956));
#20833=DIRECTION('ref_axis',(0.,-0.447213595499956,-0.894427190999917));
#20834=DIRECTION('',(0.,-0.447213595499956,-0.894427190999917));
#20835=DIRECTION('',(-1.,0.,0.));
#20836=DIRECTION('',(0.,-0.447213595499956,-0.894427190999917));
#20837=DIRECTION('center_axis',(0.,0.447213595499957,0.894427190999916));
#20838=DIRECTION('ref_axis',(0.,0.894427190999916,-0.447213595499957));
#20839=DIRECTION('',(0.,0.894427190999917,-0.447213595499957));
#20840=DIRECTION('',(-1.,0.,0.));
#20841=DIRECTION('',(0.,0.894427190999916,-0.447213595499957));
#20842=DIRECTION('center_axis',(0.,0.894427190999916,-0.447213595499958));
#20843=DIRECTION('ref_axis',(0.,-0.447213595499958,-0.894427190999916));
#20844=DIRECTION('',(0.,-0.447213595499958,-0.894427190999916));
#20845=DIRECTION('',(-1.,0.,0.));
#20846=DIRECTION('',(0.,-0.447213595499958,-0.894427190999916));
#20847=DIRECTION('center_axis',(0.,-0.447213595499958,-0.894427190999916));
#20848=DIRECTION('ref_axis',(0.,-0.894427190999916,0.447213595499958));
#20849=DIRECTION('',(0.,-0.894427190999916,0.447213595499958));
#20850=DIRECTION('',(-1.,0.,0.));
#20851=DIRECTION('',(0.,-0.894427190999916,0.447213595499958));
#20852=DIRECTION('center_axis',(0.,0.894427190999916,-0.447213595499958));
#20853=DIRECTION('ref_axis',(0.,-0.447213595499958,-0.894427190999916));
#20854=DIRECTION('',(0.,-0.447213595499958,-0.894427190999916));
#20855=DIRECTION('',(-1.,0.,0.));
#20856=DIRECTION('',(0.,-0.447213595499958,-0.894427190999916));
#20857=DIRECTION('center_axis',(0.,0.447213595499958,0.894427190999916));
#20858=DIRECTION('ref_axis',(0.,0.894427190999916,-0.447213595499958));
#20859=DIRECTION('',(0.,0.894427190999916,-0.447213595499958));
#20860=DIRECTION('',(-1.,0.,0.));
#20861=DIRECTION('',(0.,0.894427190999916,-0.447213595499958));
#20862=DIRECTION('center_axis',(0.,-0.894427190999916,0.447213595499958));
#20863=DIRECTION('ref_axis',(0.,0.447213595499958,0.894427190999916));
#20864=DIRECTION('',(0.,0.447213595499958,0.894427190999916));
#20865=DIRECTION('',(-1.,0.,0.));
#20866=DIRECTION('',(0.,0.447213595499958,0.894427190999916));
#20867=DIRECTION('center_axis',(0.,-0.447213595499957,-0.894427190999916));
#20868=DIRECTION('ref_axis',(0.,-0.894427190999916,0.447213595499957));
#20869=DIRECTION('',(0.,-0.894427190999916,0.447213595499957));
#20870=DIRECTION('',(-1.,0.,0.));
#20871=DIRECTION('',(0.,-0.894427190999916,0.447213595499957));
#20872=DIRECTION('center_axis',(0.,0.894427190999916,-0.447213595499958));
#20873=DIRECTION('ref_axis',(0.,-0.447213595499958,-0.894427190999916));
#20874=DIRECTION('',(0.,-0.447213595499958,-0.894427190999916));
#20875=DIRECTION('',(0.,-0.447213595499958,-0.894427190999916));
#20876=DIRECTION('center_axis',(-1.,0.,0.));
#20877=DIRECTION('ref_axis',(0.,0.,1.));
#20878=DIRECTION('center_axis',(-1.,0.,0.));
#20879=DIRECTION('ref_axis',(0.,0.,1.));
#20880=DIRECTION('center_axis',(1.,0.,0.));
#20881=DIRECTION('ref_axis',(0.,0.,-1.));
#20882=DIRECTION('center_axis',(1.,0.,0.));
#20883=DIRECTION('ref_axis',(0.,0.,-1.));
#20884=DIRECTION('center_axis',(1.,0.,0.));
#20885=DIRECTION('ref_axis',(0.,1.,0.));
#20886=DIRECTION('',(1.,0.,0.));
#20887=DIRECTION('center_axis',(-1.,0.,0.));
#20888=DIRECTION('ref_axis',(0.,1.,0.));
#20889=DIRECTION('center_axis',(1.,0.,0.));
#20890=DIRECTION('ref_axis',(0.,1.,0.));
#20891=DIRECTION('',(1.,0.,0.));
#20892=DIRECTION('center_axis',(1.,0.,0.));
#20893=DIRECTION('ref_axis',(0.,1.,0.));
#20894=DIRECTION('center_axis',(1.,0.,0.));
#20895=DIRECTION('ref_axis',(0.,0.,-1.));
#20896=DIRECTION('center_axis',(0.,-0.599220281862479,0.800584195325296));
#20897=DIRECTION('ref_axis',(0.,-0.800584195325296,-0.599220281862479));
#20898=DIRECTION('',(-1.,0.,0.));
#20899=DIRECTION('',(0.,-0.800584195325296,-0.599220281862479));
#20900=DIRECTION('',(1.,0.,0.));
#20901=DIRECTION('',(0.,-0.800584195325296,-0.599220281862479));
#20902=DIRECTION('center_axis',(1.,0.,0.));
#20903=DIRECTION('ref_axis',(0.,-0.20791169081776,-0.978147600733805));
#20904=DIRECTION('center_axis',(-1.,0.,0.));
#20905=DIRECTION('ref_axis',(0.,1.,0.));
#20906=DIRECTION('',(0.,0.4876452091922,-0.873041894728939));
#20907=DIRECTION('center_axis',(0.,-0.873041894728939,-0.4876452091922));
#20908=DIRECTION('ref_axis',(0.,0.4876452091922,-0.873041894728939));
#20909=DIRECTION('',(1.,0.,0.));
#20910=DIRECTION('',(0.,0.4876452091922,-0.873041894728939));
#20911=DIRECTION('center_axis',(1.,0.,0.));
#20912=DIRECTION('ref_axis',(0.,-0.20791169081776,-0.978147600733805));
#20913=DIRECTION('center_axis',(1.,0.,0.));
#20914=DIRECTION('ref_axis',(0.,1.,0.));
#20915=DIRECTION('center_axis',(0.,-0.419675067322761,0.907674411817165));
#20916=DIRECTION('ref_axis',(0.,-0.907674411817165,-0.419675067322761));
#20917=DIRECTION('',(-1.,0.,0.));
#20918=DIRECTION('',(0.,-0.907674411817165,-0.419675067322761));
#20919=DIRECTION('',(1.,0.,0.));
#20920=DIRECTION('',(0.,-0.907674411817165,-0.419675067322761));
#20921=DIRECTION('center_axis',(1.,0.,0.));
#20922=DIRECTION('ref_axis',(0.,-0.406736643075801,-0.913545457642601));
#20923=DIRECTION('center_axis',(-1.,0.,0.));
#20924=DIRECTION('ref_axis',(0.,1.,0.));
#20925=DIRECTION('',(0.,0.295473374892851,-0.955350974631538));
#20926=DIRECTION('center_axis',(0.,-0.955350974631538,-0.295473374892851));
#20927=DIRECTION('ref_axis',(0.,0.295473374892851,-0.955350974631538));
#20928=DIRECTION('',(1.,0.,0.));
#20929=DIRECTION('',(0.,0.295473374892851,-0.955350974631538));
#20930=DIRECTION('center_axis',(1.,0.,0.));
#20931=DIRECTION('ref_axis',(0.,-0.406736643075801,-0.913545457642601));
#20932=DIRECTION('center_axis',(1.,0.,0.));
#20933=DIRECTION('ref_axis',(0.,1.,0.));
#20934=DIRECTION('center_axis',(0.,-0.221788038516636,0.97509490100756));
#20935=DIRECTION('ref_axis',(0.,-0.97509490100756,-0.221788038516636));
#20936=DIRECTION('',(-1.,0.,0.));
#20937=DIRECTION('',(0.,-0.97509490100756,-0.221788038516636));
#20938=DIRECTION('',(1.,0.,0.));
#20939=DIRECTION('',(0.,-0.97509490100756,-0.221788038516636));
#20940=DIRECTION('center_axis',(1.,0.,0.));
#20941=DIRECTION('ref_axis',(0.,-0.587785252292473,-0.809016994374947));
#20942=DIRECTION('center_axis',(-1.,0.,0.));
#20943=DIRECTION('ref_axis',(0.,1.,0.));
#20944=DIRECTION('',(0.,0.0903879362721259,-0.995906632660144));
#20945=DIRECTION('center_axis',(0.,-0.995906632660144,-0.0903879362721259));
#20946=DIRECTION('ref_axis',(0.,0.0903879362721259,-0.995906632660144));
#20947=DIRECTION('',(1.,0.,0.));
#20948=DIRECTION('',(0.,0.0903879362721259,-0.995906632660144));
#20949=DIRECTION('center_axis',(1.,0.,0.));
#20950=DIRECTION('ref_axis',(0.,-0.587785252292473,-0.809016994374947));
#20951=DIRECTION('center_axis',(1.,0.,0.));
#20952=DIRECTION('ref_axis',(0.,1.,0.));
#20953=DIRECTION('center_axis',(0.,-0.0142078081702462,0.999899063999461));
#20954=DIRECTION('ref_axis',(0.,-0.999899063999461,-0.0142078081702462));
#20955=DIRECTION('',(-1.,0.,0.));
#20956=DIRECTION('',(0.,-0.999899063999461,-0.0142078081702462));
#20957=DIRECTION('',(1.,0.,0.));
#20958=DIRECTION('',(0.,-0.999899063999461,-0.0142078081702462));
#20959=DIRECTION('center_axis',(1.,0.,0.));
#20960=DIRECTION('ref_axis',(0.,-0.743144825477395,-0.669130606358858));
#20961=DIRECTION('center_axis',(-1.,0.,0.));
#20962=DIRECTION('ref_axis',(0.,1.,0.));
#20963=DIRECTION('',(0.,-0.118647888893132,-0.992936391951268));
#20964=DIRECTION('center_axis',(0.,-0.992936391951268,0.118647888893132));
#20965=DIRECTION('ref_axis',(0.,-0.118647888893132,-0.992936391951268));
#20966=DIRECTION('',(1.,0.,0.));
#20967=DIRECTION('',(0.,-0.118647888893132,-0.992936391951268));
#20968=DIRECTION('center_axis',(1.,0.,0.));
#20969=DIRECTION('ref_axis',(0.,-0.743144825477395,-0.669130606358858));
#20970=DIRECTION('center_axis',(1.,0.,0.));
#20971=DIRECTION('ref_axis',(0.,1.,0.));
#20972=DIRECTION('center_axis',(0.,0.193993371569811,0.981002839846541));
#20973=DIRECTION('ref_axis',(0.,-0.981002839846541,0.193993371569811));
#20974=DIRECTION('',(-1.,0.,0.));
#20975=DIRECTION('',(0.,-0.981002839846541,0.193993371569811));
#20976=DIRECTION('',(1.,0.,0.));
#20977=DIRECTION('',(0.,-0.981002839846541,0.193993371569811));
#20978=DIRECTION('center_axis',(1.,0.,0.));
#20979=DIRECTION('ref_axis',(0.,-0.866025403784439,-0.499999999999999));
#20980=DIRECTION('center_axis',(-1.,0.,0.));
#20981=DIRECTION('ref_axis',(0.,1.,0.));
#20982=DIRECTION('',(0.,-0.322498231978022,-0.946570066276686));
#20983=DIRECTION('center_axis',(0.,-0.946570066276686,0.322498231978022));
#20984=DIRECTION('ref_axis',(0.,-0.322498231978022,-0.946570066276686));
#20985=DIRECTION('',(1.,0.,0.));
#20986=DIRECTION('',(0.,-0.322498231978022,-0.946570066276686));
#20987=DIRECTION('center_axis',(1.,0.,0.));
#20988=DIRECTION('ref_axis',(0.,-0.866025403784439,-0.499999999999999));
#20989=DIRECTION('center_axis',(1.,0.,0.));
#20990=DIRECTION('ref_axis',(0.,1.,0.));
#20991=DIRECTION('center_axis',(0.,0.393716110088789,0.919232084218427));
#20992=DIRECTION('ref_axis',(0.,-0.919232084218427,0.393716110088789));
#20993=DIRECTION('',(-1.,0.,0.));
#20994=DIRECTION('',(0.,-0.919232084218427,0.393716110088789));
#20995=DIRECTION('',(1.,0.,0.));
#20996=DIRECTION('',(0.,-0.919232084218427,0.393716110088789));
#20997=DIRECTION('center_axis',(1.,0.,0.));
#20998=DIRECTION('ref_axis',(0.,-0.951056516295154,-0.309016994374947));
#20999=DIRECTION('center_axis',(-1.,0.,0.));
#21000=DIRECTION('ref_axis',(0.,1.,0.));
#21001=DIRECTION('',(0.,-0.51225385480726,-0.858834086558692));
#21002=DIRECTION('center_axis',(0.,-0.858834086558692,0.51225385480726));
#21003=DIRECTION('ref_axis',(0.,-0.51225385480726,-0.858834086558692));
#21004=DIRECTION('',(1.,0.,0.));
#21005=DIRECTION('',(0.,-0.51225385480726,-0.858834086558692));
#21006=DIRECTION('center_axis',(1.,0.,0.));
#21007=DIRECTION('ref_axis',(0.,-0.951056516295154,-0.309016994374947));
#21008=DIRECTION('center_axis',(1.,0.,0.));
#21009=DIRECTION('ref_axis',(0.,1.,0.));
#21010=DIRECTION('center_axis',(0.,0.576231565337382,0.817286475545038));
#21011=DIRECTION('ref_axis',(0.,-0.817286475545038,0.576231565337382));
#21012=DIRECTION('',(-1.,0.,0.));
#21013=DIRECTION('',(0.,-0.817286475545038,0.576231565337382));
#21014=DIRECTION('',(1.,0.,0.));
#21015=DIRECTION('',(0.,-0.817286475545038,0.576231565337382));
#21016=DIRECTION('center_axis',(1.,0.,0.));
#21017=DIRECTION('ref_axis',(0.,-0.994521895368273,-0.104528463267653));
#21018=DIRECTION('center_axis',(-1.,0.,0.));
#21019=DIRECTION('ref_axis',(0.,1.,0.));
#21020=DIRECTION('',(0.,-0.679621526114708,-0.733562936114901));
#21021=DIRECTION('center_axis',(0.,-0.733562936114901,0.679621526114709));
#21022=DIRECTION('ref_axis',(0.,-0.679621526114708,-0.733562936114901));
#21023=DIRECTION('',(1.,0.,0.));
#21024=DIRECTION('',(0.,-0.679621526114708,-0.733562936114901));
#21025=DIRECTION('center_axis',(1.,0.,0.));
#21026=DIRECTION('ref_axis',(0.,-0.994521895368273,-0.104528463267653));
#21027=DIRECTION('center_axis',(1.,0.,0.));
#21028=DIRECTION('ref_axis',(0.,1.,0.));
#21029=DIRECTION('center_axis',(0.,0.733562936114902,0.679621526114708));
#21030=DIRECTION('ref_axis',(0.,-0.679621526114708,0.733562936114902));
#21031=DIRECTION('',(-1.,0.,0.));
#21032=DIRECTION('',(0.,-0.679621526114708,0.733562936114902));
#21033=DIRECTION('',(1.,0.,0.));
#21034=DIRECTION('',(0.,-0.679621526114708,0.733562936114902));
#21035=DIRECTION('center_axis',(1.,0.,0.));
#21036=DIRECTION('ref_axis',(0.,-0.994521895368273,0.104528463267654));
#21037=DIRECTION('center_axis',(-1.,0.,0.));
#21038=DIRECTION('ref_axis',(0.,1.,0.));
#21039=DIRECTION('',(0.,-0.817286475545039,-0.576231565337381));
#21040=DIRECTION('center_axis',(0.,-0.576231565337381,0.817286475545039));
#21041=DIRECTION('ref_axis',(0.,-0.817286475545039,-0.576231565337381));
#21042=DIRECTION('',(1.,0.,0.));
#21043=DIRECTION('',(0.,-0.817286475545039,-0.576231565337381));
#21044=DIRECTION('center_axis',(1.,0.,0.));
#21045=DIRECTION('ref_axis',(0.,-0.994521895368273,0.104528463267654));
#21046=DIRECTION('center_axis',(1.,0.,0.));
#21047=DIRECTION('ref_axis',(0.,1.,0.));
#21048=DIRECTION('center_axis',(0.,0.858834086558692,0.51225385480726));
#21049=DIRECTION('ref_axis',(0.,-0.51225385480726,0.858834086558692));
#21050=DIRECTION('',(-1.,0.,0.));
#21051=DIRECTION('',(0.,-0.51225385480726,0.858834086558692));
#21052=DIRECTION('',(1.,0.,0.));
#21053=DIRECTION('',(0.,-0.51225385480726,0.858834086558692));
#21054=DIRECTION('center_axis',(1.,0.,0.));
#21055=DIRECTION('ref_axis',(0.,-0.951056516295153,0.309016994374948));
#21056=DIRECTION('center_axis',(-1.,0.,0.));
#21057=DIRECTION('ref_axis',(0.,1.,0.));
#21058=DIRECTION('',(0.,-0.919232084218427,-0.393716110088789));
#21059=DIRECTION('center_axis',(0.,-0.393716110088789,0.919232084218427));
#21060=DIRECTION('ref_axis',(0.,-0.919232084218427,-0.393716110088789));
#21061=DIRECTION('',(1.,0.,0.));
#21062=DIRECTION('',(0.,-0.919232084218427,-0.393716110088789));
#21063=DIRECTION('center_axis',(1.,0.,0.));
#21064=DIRECTION('ref_axis',(0.,-0.951056516295153,0.309016994374948));
#21065=DIRECTION('center_axis',(1.,0.,0.));
#21066=DIRECTION('ref_axis',(0.,1.,0.));
#21067=DIRECTION('center_axis',(0.,0.946570066276687,0.322498231978021));
#21068=DIRECTION('ref_axis',(0.,-0.322498231978021,0.946570066276686));
#21069=DIRECTION('',(-1.,0.,0.));
#21070=DIRECTION('',(0.,-0.322498231978021,0.946570066276686));
#21071=DIRECTION('',(1.,0.,0.));
#21072=DIRECTION('',(0.,-0.322498231978021,0.946570066276686));
#21073=DIRECTION('center_axis',(1.,0.,0.));
#21074=DIRECTION('ref_axis',(0.,-0.866025403784438,0.5));
#21075=DIRECTION('center_axis',(-1.,0.,0.));
#21076=DIRECTION('ref_axis',(0.,1.,0.));
#21077=DIRECTION('',(0.,-0.981002839846541,-0.193993371569809));
#21078=DIRECTION('center_axis',(0.,-0.193993371569809,0.981002839846541));
#21079=DIRECTION('ref_axis',(0.,-0.981002839846541,-0.193993371569809));
#21080=DIRECTION('',(1.,0.,0.));
#21081=DIRECTION('',(0.,-0.981002839846541,-0.193993371569809));
#21082=DIRECTION('center_axis',(1.,0.,0.));
#21083=DIRECTION('ref_axis',(0.,-0.866025403784438,0.5));
#21084=DIRECTION('center_axis',(1.,0.,0.));
#21085=DIRECTION('ref_axis',(0.,1.,0.));
#21086=DIRECTION('center_axis',(0.,0.992936391951269,0.118647888893131));
#21087=DIRECTION('ref_axis',(0.,-0.118647888893131,0.992936391951268));
#21088=DIRECTION('',(-1.,0.,0.));
#21089=DIRECTION('',(0.,-0.118647888893131,0.992936391951268));
#21090=DIRECTION('',(1.,0.,0.));
#21091=DIRECTION('',(0.,-0.118647888893131,0.992936391951268));
#21092=DIRECTION('center_axis',(1.,0.,0.));
#21093=DIRECTION('ref_axis',(0.,-0.743144825477394,0.669130606358858));
#21094=DIRECTION('center_axis',(-1.,0.,0.));
#21095=DIRECTION('ref_axis',(0.,1.,0.));
#21096=DIRECTION('',(0.,-0.999899063999461,0.014207808170247));
#21097=DIRECTION('center_axis',(0.,0.014207808170247,0.999899063999461));
#21098=DIRECTION('ref_axis',(0.,-0.999899063999461,0.014207808170247));
#21099=DIRECTION('',(1.,0.,0.));
#21100=DIRECTION('',(0.,-0.999899063999461,0.014207808170247));
#21101=DIRECTION('center_axis',(1.,0.,0.));
#21102=DIRECTION('ref_axis',(0.,-0.743144825477394,0.669130606358858));
#21103=DIRECTION('center_axis',(1.,0.,0.));
#21104=DIRECTION('ref_axis',(0.,1.,0.));
#21105=DIRECTION('center_axis',(0.,0.995906632660144,-0.0903879362721262));
#21106=DIRECTION('ref_axis',(0.,0.0903879362721261,0.995906632660144));
#21107=DIRECTION('',(-1.,0.,0.));
#21108=DIRECTION('',(0.,0.0903879362721261,0.995906632660144));
#21109=DIRECTION('',(1.,0.,0.));
#21110=DIRECTION('',(0.,0.0903879362721261,0.995906632660144));
#21111=DIRECTION('center_axis',(1.,0.,0.));
#21112=DIRECTION('ref_axis',(0.,-0.587785252292473,0.809016994374947));
#21113=DIRECTION('center_axis',(-1.,0.,0.));
#21114=DIRECTION('ref_axis',(0.,1.,0.));
#21115=DIRECTION('',(0.,-0.97509490100756,0.221788038516636));
#21116=DIRECTION('center_axis',(0.,0.221788038516636,0.97509490100756));
#21117=DIRECTION('ref_axis',(0.,-0.97509490100756,0.221788038516636));
#21118=DIRECTION('',(1.,0.,0.));
#21119=DIRECTION('',(0.,-0.97509490100756,0.221788038516636));
#21120=DIRECTION('center_axis',(1.,0.,0.));
#21121=DIRECTION('ref_axis',(0.,-0.587785252292473,0.809016994374947));
#21122=DIRECTION('center_axis',(1.,0.,0.));
#21123=DIRECTION('ref_axis',(0.,1.,0.));
#21124=DIRECTION('center_axis',(0.,0.955350974631537,-0.295473374892852));
#21125=DIRECTION('ref_axis',(0.,0.295473374892852,0.955350974631537));
#21126=DIRECTION('',(-1.,0.,0.));
#21127=DIRECTION('',(0.,0.295473374892852,0.955350974631537));
#21128=DIRECTION('',(1.,0.,0.));
#21129=DIRECTION('',(0.,0.295473374892852,0.955350974631537));
#21130=DIRECTION('center_axis',(1.,0.,0.));
#21131=DIRECTION('ref_axis',(0.,-0.4067366430758,0.913545457642601));
#21132=DIRECTION('center_axis',(-1.,0.,0.));
#21133=DIRECTION('ref_axis',(0.,1.,0.));
#21134=DIRECTION('',(0.,-0.907674411817164,0.419675067322762));
#21135=DIRECTION('center_axis',(0.,0.419675067322762,0.907674411817164));
#21136=DIRECTION('ref_axis',(0.,-0.907674411817164,0.419675067322762));
#21137=DIRECTION('',(1.,0.,0.));
#21138=DIRECTION('',(0.,-0.907674411817164,0.419675067322762));
#21139=DIRECTION('center_axis',(1.,0.,0.));
#21140=DIRECTION('ref_axis',(0.,-0.4067366430758,0.913545457642601));
#21141=DIRECTION('center_axis',(1.,0.,0.));
#21142=DIRECTION('ref_axis',(0.,1.,0.));
#21143=DIRECTION('center_axis',(0.,0.873041894728938,-0.487645209192201));
#21144=DIRECTION('ref_axis',(0.,0.487645209192201,0.873041894728938));
#21145=DIRECTION('',(-1.,0.,0.));
#21146=DIRECTION('',(0.,0.487645209192201,0.873041894728938));
#21147=DIRECTION('',(1.,0.,0.));
#21148=DIRECTION('',(0.,0.487645209192201,0.873041894728938));
#21149=DIRECTION('center_axis',(1.,0.,0.));
#21150=DIRECTION('ref_axis',(0.,-0.207911690817759,0.978147600733806));
#21151=DIRECTION('center_axis',(-1.,0.,0.));
#21152=DIRECTION('ref_axis',(0.,1.,0.));
#21153=DIRECTION('',(0.,-0.800584195325295,0.59922028186248));
#21154=DIRECTION('center_axis',(0.,0.59922028186248,0.800584195325295));
#21155=DIRECTION('ref_axis',(0.,-0.800584195325295,0.59922028186248));
#21156=DIRECTION('',(1.,0.,0.));
#21157=DIRECTION('',(0.,-0.800584195325295,0.59922028186248));
#21158=DIRECTION('center_axis',(1.,0.,0.));
#21159=DIRECTION('ref_axis',(0.,-0.207911690817759,0.978147600733806));
#21160=DIRECTION('center_axis',(1.,0.,0.));
#21161=DIRECTION('ref_axis',(0.,1.,0.));
#21162=DIRECTION('center_axis',(0.,0.752576694706876,-0.65850460786852));
#21163=DIRECTION('ref_axis',(0.,0.65850460786852,0.752576694706876));
#21164=DIRECTION('',(-1.,0.,0.));
#21165=DIRECTION('',(0.,0.65850460786852,0.752576694706876));
#21166=DIRECTION('',(1.,0.,0.));
#21167=DIRECTION('',(0.,0.65850460786852,0.752576694706876));
#21168=DIRECTION('center_axis',(1.,0.,0.));
#21169=DIRECTION('ref_axis',(0.,1.22464679914735E-16,1.));
#21170=DIRECTION('center_axis',(-1.,0.,0.));
#21171=DIRECTION('ref_axis',(0.,1.,0.));
#21172=DIRECTION('',(0.,-0.658504607868519,0.752576694706877));
#21173=DIRECTION('center_axis',(-1.,0.,0.));
#21174=DIRECTION('ref_axis',(0.,1.,0.));
#21175=DIRECTION('center_axis',(0.,0.752576694706877,0.658504607868519));
#21176=DIRECTION('ref_axis',(0.,-0.658504607868519,0.752576694706877));
#21177=DIRECTION('',(1.,0.,0.));
#21178=DIRECTION('',(0.,-0.658504607868519,0.752576694706877));
#21179=DIRECTION('center_axis',(1.,0.,0.));
#21180=DIRECTION('ref_axis',(0.,1.22464679914735E-16,1.));
#21181=DIRECTION('center_axis',(1.,0.,0.));
#21182=DIRECTION('ref_axis',(0.,1.,0.));
#21183=DIRECTION('center_axis',(1.,0.,0.));
#21184=DIRECTION('ref_axis',(0.,1.,0.));
#21185=DIRECTION('center_axis',(0.,0.599220281862479,-0.800584195325296));
#21186=DIRECTION('ref_axis',(0.,0.800584195325295,0.599220281862479));
#21187=DIRECTION('',(-1.,0.,0.));
#21188=DIRECTION('',(0.,0.800584195325295,0.599220281862479));
#21189=DIRECTION('',(1.,0.,0.));
#21190=DIRECTION('',(0.,0.800584195325295,0.599220281862479));
#21191=DIRECTION('center_axis',(1.,0.,0.));
#21192=DIRECTION('ref_axis',(0.,0.20791169081776,0.978147600733805));
#21193=DIRECTION('center_axis',(-1.,0.,0.));
#21194=DIRECTION('ref_axis',(0.,1.,0.));
#21195=DIRECTION('',(0.,-0.4876452091922,0.873041894728939));
#21196=DIRECTION('center_axis',(0.,0.873041894728939,0.4876452091922));
#21197=DIRECTION('ref_axis',(0.,-0.4876452091922,0.873041894728939));
#21198=DIRECTION('',(1.,0.,0.));
#21199=DIRECTION('',(0.,-0.4876452091922,0.873041894728939));
#21200=DIRECTION('center_axis',(1.,0.,0.));
#21201=DIRECTION('ref_axis',(0.,0.20791169081776,0.978147600733805));
#21202=DIRECTION('center_axis',(1.,0.,0.));
#21203=DIRECTION('ref_axis',(0.,1.,0.));
#21204=DIRECTION('center_axis',(0.,0.419675067322761,-0.907674411817165));
#21205=DIRECTION('ref_axis',(0.,0.907674411817165,0.419675067322761));
#21206=DIRECTION('',(-1.,0.,0.));
#21207=DIRECTION('',(0.,0.907674411817165,0.419675067322761));
#21208=DIRECTION('',(1.,0.,0.));
#21209=DIRECTION('',(0.,0.907674411817165,0.419675067322761));
#21210=DIRECTION('center_axis',(1.,0.,0.));
#21211=DIRECTION('ref_axis',(0.,0.4067366430758,0.913545457642601));
#21212=DIRECTION('center_axis',(-1.,0.,0.));
#21213=DIRECTION('ref_axis',(0.,1.,0.));
#21214=DIRECTION('',(0.,-0.295473374892852,0.955350974631537));
#21215=DIRECTION('center_axis',(0.,0.955350974631537,0.295473374892852));
#21216=DIRECTION('ref_axis',(0.,-0.295473374892852,0.955350974631537));
#21217=DIRECTION('',(1.,0.,0.));
#21218=DIRECTION('',(0.,-0.295473374892852,0.955350974631537));
#21219=DIRECTION('center_axis',(1.,0.,0.));
#21220=DIRECTION('ref_axis',(0.,0.4067366430758,0.913545457642601));
#21221=DIRECTION('center_axis',(1.,0.,0.));
#21222=DIRECTION('ref_axis',(0.,1.,0.));
#21223=DIRECTION('center_axis',(0.,0.221788038516636,-0.97509490100756));
#21224=DIRECTION('ref_axis',(0.,0.97509490100756,0.221788038516636));
#21225=DIRECTION('',(-1.,0.,0.));
#21226=DIRECTION('',(0.,0.97509490100756,0.221788038516636));
#21227=DIRECTION('',(1.,0.,0.));
#21228=DIRECTION('',(0.,0.97509490100756,0.221788038516636));
#21229=DIRECTION('center_axis',(1.,0.,0.));
#21230=DIRECTION('ref_axis',(0.,0.587785252292473,0.809016994374947));
#21231=DIRECTION('center_axis',(-1.,0.,0.));
#21232=DIRECTION('ref_axis',(0.,1.,0.));
#21233=DIRECTION('',(0.,-0.0903879362721259,0.995906632660144));
#21234=DIRECTION('center_axis',(0.,0.995906632660144,0.0903879362721259));
#21235=DIRECTION('ref_axis',(0.,-0.0903879362721259,0.995906632660144));
#21236=DIRECTION('',(1.,0.,0.));
#21237=DIRECTION('',(0.,-0.0903879362721259,0.995906632660144));
#21238=DIRECTION('center_axis',(1.,0.,0.));
#21239=DIRECTION('ref_axis',(0.,0.587785252292473,0.809016994374947));
#21240=DIRECTION('center_axis',(1.,0.,0.));
#21241=DIRECTION('ref_axis',(0.,1.,0.));
#21242=DIRECTION('center_axis',(0.,0.0142078081702464,-0.999899063999461));
#21243=DIRECTION('ref_axis',(0.,0.999899063999461,0.0142078081702464));
#21244=DIRECTION('',(-1.,0.,0.));
#21245=DIRECTION('',(0.,0.999899063999461,0.0142078081702464));
#21246=DIRECTION('',(1.,0.,0.));
#21247=DIRECTION('',(0.,0.999899063999461,0.0142078081702464));
#21248=DIRECTION('center_axis',(1.,0.,0.));
#21249=DIRECTION('ref_axis',(0.,0.743144825477394,0.669130606358858));
#21250=DIRECTION('center_axis',(-1.,0.,0.));
#21251=DIRECTION('ref_axis',(0.,1.,0.));
#21252=DIRECTION('',(0.,0.118647888893132,0.992936391951268));
#21253=DIRECTION('center_axis',(0.,0.992936391951269,-0.118647888893132));
#21254=DIRECTION('ref_axis',(0.,0.118647888893132,0.992936391951268));
#21255=DIRECTION('',(1.,0.,0.));
#21256=DIRECTION('',(0.,0.118647888893132,0.992936391951268));
#21257=DIRECTION('center_axis',(1.,0.,0.));
#21258=DIRECTION('ref_axis',(0.,0.743144825477394,0.669130606358858));
#21259=DIRECTION('center_axis',(1.,0.,0.));
#21260=DIRECTION('ref_axis',(0.,1.,0.));
#21261=DIRECTION('center_axis',(0.,-0.19399337156981,-0.981002839846541));
#21262=DIRECTION('ref_axis',(0.,0.981002839846541,-0.19399337156981));
#21263=DIRECTION('',(-1.,0.,0.));
#21264=DIRECTION('',(0.,0.981002839846541,-0.19399337156981));
#21265=DIRECTION('',(1.,0.,0.));
#21266=DIRECTION('',(0.,0.981002839846541,-0.19399337156981));
#21267=DIRECTION('center_axis',(1.,0.,0.));
#21268=DIRECTION('ref_axis',(0.,0.866025403784439,0.5));
#21269=DIRECTION('center_axis',(-1.,0.,0.));
#21270=DIRECTION('ref_axis',(0.,1.,0.));
#21271=DIRECTION('',(0.,0.322498231978021,0.946570066276686));
#21272=DIRECTION('center_axis',(0.,0.946570066276686,-0.322498231978021));
#21273=DIRECTION('ref_axis',(0.,0.322498231978021,0.946570066276686));
#21274=DIRECTION('',(1.,0.,0.));
#21275=DIRECTION('',(0.,0.322498231978021,0.946570066276686));
#21276=DIRECTION('center_axis',(1.,0.,0.));
#21277=DIRECTION('ref_axis',(0.,0.866025403784439,0.5));
#21278=DIRECTION('center_axis',(1.,0.,0.));
#21279=DIRECTION('ref_axis',(0.,1.,0.));
#21280=DIRECTION('center_axis',(0.,-0.393716110088789,-0.919232084218427));
#21281=DIRECTION('ref_axis',(0.,0.919232084218427,-0.393716110088789));
#21282=DIRECTION('',(-1.,0.,0.));
#21283=DIRECTION('',(0.,0.919232084218427,-0.393716110088789));
#21284=DIRECTION('',(1.,0.,0.));
#21285=DIRECTION('',(0.,0.919232084218427,-0.393716110088789));
#21286=DIRECTION('center_axis',(1.,0.,0.));
#21287=DIRECTION('ref_axis',(0.,0.951056516295154,0.309016994374947));
#21288=DIRECTION('center_axis',(-1.,0.,0.));
#21289=DIRECTION('ref_axis',(0.,1.,0.));
#21290=DIRECTION('',(0.,0.51225385480726,0.858834086558692));
#21291=DIRECTION('center_axis',(0.,0.858834086558692,-0.51225385480726));
#21292=DIRECTION('ref_axis',(0.,0.51225385480726,0.858834086558692));
#21293=DIRECTION('',(1.,0.,0.));
#21294=DIRECTION('',(0.,0.51225385480726,0.858834086558692));
#21295=DIRECTION('center_axis',(1.,0.,0.));
#21296=DIRECTION('ref_axis',(0.,0.951056516295154,0.309016994374947));
#21297=DIRECTION('center_axis',(1.,0.,0.));
#21298=DIRECTION('ref_axis',(0.,1.,0.));
#21299=DIRECTION('center_axis',(0.,-0.576231565337382,-0.817286475545038));
#21300=DIRECTION('ref_axis',(0.,0.817286475545038,-0.576231565337382));
#21301=DIRECTION('',(-1.,0.,0.));
#21302=DIRECTION('',(0.,0.817286475545038,-0.576231565337382));
#21303=DIRECTION('',(1.,0.,0.));
#21304=DIRECTION('',(0.,0.817286475545038,-0.576231565337382));
#21305=DIRECTION('center_axis',(1.,0.,0.));
#21306=DIRECTION('ref_axis',(0.,0.994521895368273,0.104528463267653));
#21307=DIRECTION('center_axis',(-1.,0.,0.));
#21308=DIRECTION('ref_axis',(0.,1.,0.));
#21309=DIRECTION('',(0.,0.679621526114708,0.733562936114901));
#21310=DIRECTION('center_axis',(0.,0.733562936114902,-0.679621526114708));
#21311=DIRECTION('ref_axis',(0.,0.679621526114708,0.733562936114901));
#21312=DIRECTION('',(1.,0.,0.));
#21313=DIRECTION('',(0.,0.679621526114708,0.733562936114901));
#21314=DIRECTION('center_axis',(1.,0.,0.));
#21315=DIRECTION('ref_axis',(0.,0.994521895368273,0.104528463267653));
#21316=DIRECTION('center_axis',(1.,0.,0.));
#21317=DIRECTION('ref_axis',(0.,1.,0.));
#21318=DIRECTION('center_axis',(0.,-0.733562936114902,-0.679621526114708));
#21319=DIRECTION('ref_axis',(0.,0.679621526114708,-0.733562936114902));
#21320=DIRECTION('',(-1.,0.,0.));
#21321=DIRECTION('',(0.,0.679621526114708,-0.733562936114902));
#21322=DIRECTION('',(1.,0.,0.));
#21323=DIRECTION('',(0.,0.679621526114708,-0.733562936114902));
#21324=DIRECTION('center_axis',(1.,0.,0.));
#21325=DIRECTION('ref_axis',(0.,0.994521895368273,-0.104528463267654));
#21326=DIRECTION('center_axis',(-1.,0.,0.));
#21327=DIRECTION('ref_axis',(0.,1.,0.));
#21328=DIRECTION('',(0.,0.817286475545038,0.576231565337382));
#21329=DIRECTION('center_axis',(0.,0.576231565337382,-0.817286475545039));
#21330=DIRECTION('ref_axis',(0.,0.817286475545038,0.576231565337382));
#21331=DIRECTION('',(1.,0.,0.));
#21332=DIRECTION('',(0.,0.817286475545038,0.576231565337382));
#21333=DIRECTION('center_axis',(1.,0.,0.));
#21334=DIRECTION('ref_axis',(0.,0.994521895368273,-0.104528463267654));
#21335=DIRECTION('center_axis',(1.,0.,0.));
#21336=DIRECTION('ref_axis',(0.,1.,0.));
#21337=DIRECTION('center_axis',(0.,-0.858834086558692,-0.51225385480726));
#21338=DIRECTION('ref_axis',(0.,0.51225385480726,-0.858834086558692));
#21339=DIRECTION('',(-1.,0.,0.));
#21340=DIRECTION('',(0.,0.51225385480726,-0.858834086558692));
#21341=DIRECTION('',(1.,0.,0.));
#21342=DIRECTION('',(0.,0.51225385480726,-0.858834086558692));
#21343=DIRECTION('center_axis',(1.,0.,0.));
#21344=DIRECTION('ref_axis',(0.,0.951056516295154,-0.309016994374948));
#21345=DIRECTION('center_axis',(-1.,0.,0.));
#21346=DIRECTION('ref_axis',(0.,1.,0.));
#21347=DIRECTION('',(0.,0.919232084218427,0.393716110088789));
#21348=DIRECTION('center_axis',(0.,0.393716110088789,-0.919232084218427));
#21349=DIRECTION('ref_axis',(0.,0.919232084218427,0.393716110088789));
#21350=DIRECTION('',(1.,0.,0.));
#21351=DIRECTION('',(0.,0.919232084218427,0.393716110088789));
#21352=DIRECTION('center_axis',(1.,0.,0.));
#21353=DIRECTION('ref_axis',(0.,0.951056516295154,-0.309016994374948));
#21354=DIRECTION('center_axis',(1.,0.,0.));
#21355=DIRECTION('ref_axis',(0.,1.,0.));
#21356=DIRECTION('center_axis',(0.,-0.946570066276686,-0.322498231978021));
#21357=DIRECTION('ref_axis',(0.,0.322498231978021,-0.946570066276686));
#21358=DIRECTION('',(-1.,0.,0.));
#21359=DIRECTION('',(0.,0.322498231978021,-0.946570066276686));
#21360=DIRECTION('',(1.,0.,0.));
#21361=DIRECTION('',(0.,0.322498231978021,-0.946570066276686));
#21362=DIRECTION('center_axis',(1.,0.,0.));
#21363=DIRECTION('ref_axis',(0.,0.866025403784439,-0.5));
#21364=DIRECTION('center_axis',(-1.,0.,0.));
#21365=DIRECTION('ref_axis',(0.,1.,0.));
#21366=DIRECTION('',(0.,0.981002839846541,0.19399337156981));
#21367=DIRECTION('center_axis',(0.,0.19399337156981,-0.981002839846541));
#21368=DIRECTION('ref_axis',(0.,0.981002839846541,0.19399337156981));
#21369=DIRECTION('',(1.,0.,0.));
#21370=DIRECTION('',(0.,0.981002839846541,0.19399337156981));
#21371=DIRECTION('center_axis',(1.,0.,0.));
#21372=DIRECTION('ref_axis',(0.,0.866025403784439,-0.5));
#21373=DIRECTION('center_axis',(1.,0.,0.));
#21374=DIRECTION('ref_axis',(0.,1.,0.));
#21375=DIRECTION('center_axis',(0.,-0.992936391951269,-0.118647888893131));
#21376=DIRECTION('ref_axis',(0.,0.118647888893131,-0.992936391951268));
#21377=DIRECTION('',(-1.,0.,0.));
#21378=DIRECTION('',(0.,0.118647888893131,-0.992936391951268));
#21379=DIRECTION('',(1.,0.,0.));
#21380=DIRECTION('',(0.,0.118647888893131,-0.992936391951268));
#21381=DIRECTION('center_axis',(1.,0.,0.));
#21382=DIRECTION('ref_axis',(0.,0.743144825477394,-0.669130606358858));
#21383=DIRECTION('center_axis',(-1.,0.,0.));
#21384=DIRECTION('ref_axis',(0.,1.,0.));
#21385=DIRECTION('',(0.,0.999899063999461,-0.0142078081702469));
#21386=DIRECTION('center_axis',(0.,-0.0142078081702469,-0.999899063999461));
#21387=DIRECTION('ref_axis',(0.,0.999899063999461,-0.0142078081702469));
#21388=DIRECTION('',(1.,0.,0.));
#21389=DIRECTION('',(0.,0.999899063999461,-0.0142078081702469));
#21390=DIRECTION('center_axis',(1.,0.,0.));
#21391=DIRECTION('ref_axis',(0.,0.743144825477394,-0.669130606358858));
#21392=DIRECTION('center_axis',(1.,0.,0.));
#21393=DIRECTION('ref_axis',(0.,1.,0.));
#21394=DIRECTION('center_axis',(0.,-0.995906632660144,0.0903879362721262));
#21395=DIRECTION('ref_axis',(0.,-0.0903879362721261,-0.995906632660144));
#21396=DIRECTION('',(-1.,0.,0.));
#21397=DIRECTION('',(0.,-0.0903879362721261,-0.995906632660144));
#21398=DIRECTION('',(1.,0.,0.));
#21399=DIRECTION('',(0.,-0.0903879362721261,-0.995906632660144));
#21400=DIRECTION('center_axis',(1.,0.,0.));
#21401=DIRECTION('ref_axis',(0.,0.587785252292473,-0.809016994374947));
#21402=DIRECTION('center_axis',(-1.,0.,0.));
#21403=DIRECTION('ref_axis',(0.,1.,0.));
#21404=DIRECTION('',(0.,0.97509490100756,-0.221788038516636));
#21405=DIRECTION('center_axis',(0.,-0.221788038516636,-0.97509490100756));
#21406=DIRECTION('ref_axis',(0.,0.97509490100756,-0.221788038516636));
#21407=DIRECTION('',(1.,0.,0.));
#21408=DIRECTION('',(0.,0.97509490100756,-0.221788038516636));
#21409=DIRECTION('center_axis',(1.,0.,0.));
#21410=DIRECTION('ref_axis',(0.,0.587785252292473,-0.809016994374947));
#21411=DIRECTION('center_axis',(1.,0.,0.));
#21412=DIRECTION('ref_axis',(0.,1.,0.));
#21413=DIRECTION('center_axis',(0.,-0.955350974631537,0.295473374892852));
#21414=DIRECTION('ref_axis',(0.,-0.295473374892852,-0.955350974631537));
#21415=DIRECTION('',(-1.,0.,0.));
#21416=DIRECTION('',(0.,-0.295473374892852,-0.955350974631537));
#21417=DIRECTION('',(1.,0.,0.));
#21418=DIRECTION('',(0.,-0.295473374892852,-0.955350974631537));
#21419=DIRECTION('center_axis',(1.,0.,0.));
#21420=DIRECTION('ref_axis',(0.,0.4067366430758,-0.913545457642601));
#21421=DIRECTION('center_axis',(-1.,0.,0.));
#21422=DIRECTION('ref_axis',(0.,1.,0.));
#21423=DIRECTION('',(0.,0.907674411817164,-0.419675067322762));
#21424=DIRECTION('center_axis',(0.,-0.419675067322762,-0.907674411817164));
#21425=DIRECTION('ref_axis',(0.,0.907674411817164,-0.419675067322762));
#21426=DIRECTION('',(1.,0.,0.));
#21427=DIRECTION('',(0.,0.907674411817164,-0.419675067322762));
#21428=DIRECTION('center_axis',(1.,0.,0.));
#21429=DIRECTION('ref_axis',(0.,0.4067366430758,-0.913545457642601));
#21430=DIRECTION('center_axis',(1.,0.,0.));
#21431=DIRECTION('ref_axis',(0.,1.,0.));
#21432=DIRECTION('center_axis',(0.,-0.873041894728939,0.487645209192201));
#21433=DIRECTION('ref_axis',(0.,-0.487645209192201,-0.873041894728939));
#21434=DIRECTION('',(-1.,0.,0.));
#21435=DIRECTION('',(0.,-0.487645209192201,-0.873041894728939));
#21436=DIRECTION('',(1.,0.,0.));
#21437=DIRECTION('',(0.,-0.487645209192201,-0.873041894728939));
#21438=DIRECTION('center_axis',(1.,0.,0.));
#21439=DIRECTION('ref_axis',(0.,0.207911690817759,-0.978147600733806));
#21440=DIRECTION('center_axis',(-1.,0.,0.));
#21441=DIRECTION('ref_axis',(0.,1.,0.));
#21442=DIRECTION('',(0.,0.800584195325295,-0.59922028186248));
#21443=DIRECTION('center_axis',(0.,-0.59922028186248,-0.800584195325295));
#21444=DIRECTION('ref_axis',(0.,0.800584195325295,-0.59922028186248));
#21445=DIRECTION('',(1.,0.,0.));
#21446=DIRECTION('',(0.,0.800584195325295,-0.59922028186248));
#21447=DIRECTION('center_axis',(1.,0.,0.));
#21448=DIRECTION('ref_axis',(0.,0.207911690817759,-0.978147600733806));
#21449=DIRECTION('center_axis',(1.,0.,0.));
#21450=DIRECTION('ref_axis',(0.,1.,0.));
#21451=DIRECTION('center_axis',(0.,-0.752576694706877,0.65850460786852));
#21452=DIRECTION('ref_axis',(0.,-0.65850460786852,-0.752576694706877));
#21453=DIRECTION('',(-1.,0.,0.));
#21454=DIRECTION('',(0.,-0.65850460786852,-0.752576694706877));
#21455=DIRECTION('',(1.,0.,0.));
#21456=DIRECTION('',(0.,-0.65850460786852,-0.752576694706877));
#21457=DIRECTION('center_axis',(1.,0.,0.));
#21458=DIRECTION('ref_axis',(0.,0.,-1.));
#21459=DIRECTION('center_axis',(-1.,0.,0.));
#21460=DIRECTION('ref_axis',(0.,1.,0.));
#21461=DIRECTION('',(0.,0.65850460786852,-0.752576694706877));
#21462=DIRECTION('center_axis',(0.,-0.752576694706877,-0.65850460786852));
#21463=DIRECTION('ref_axis',(0.,0.65850460786852,-0.752576694706877));
#21464=DIRECTION('',(1.,0.,0.));
#21465=DIRECTION('',(0.,0.65850460786852,-0.752576694706877));
#21466=DIRECTION('center_axis',(1.,0.,0.));
#21467=DIRECTION('ref_axis',(0.,0.,-1.));
#21468=DIRECTION('center_axis',(1.,0.,0.));
#21469=DIRECTION('ref_axis',(0.,1.,0.));
#21470=DIRECTION('center_axis',(-1.,0.,0.));
#21471=DIRECTION('ref_axis',(0.,0.,1.));
#21472=DIRECTION('center_axis',(1.,0.,0.));
#21473=DIRECTION('ref_axis',(0.,0.,-1.));
#21474=DIRECTION('center_axis',(1.,0.,0.));
#21475=DIRECTION('ref_axis',(0.,1.,0.));
#21476=DIRECTION('center_axis',(1.,0.,0.));
#21477=DIRECTION('ref_axis',(0.,0.,-1.));
#21478=DIRECTION('',(-0.554700196225229,0.832050294337844,1.01896772969045E-16));
#21479=DIRECTION('center_axis',(1.,0.,0.));
#21480=DIRECTION('ref_axis',(0.,1.,0.));
#21481=DIRECTION('',(-0.707106781186547,0.707106781186548,8.65956056235493E-17));
#21482=DIRECTION('center_axis',(1.,0.,0.));
#21483=DIRECTION('ref_axis',(0.,-0.367056220099871,-0.93019875902196));
#21484=DIRECTION('center_axis',(1.,0.,0.));
#21485=DIRECTION('ref_axis',(0.,1.,0.));
#21486=DIRECTION('center_axis',(1.,0.,0.));
#21487=DIRECTION('ref_axis',(0.,0.,-1.));
#21488=DIRECTION('',(-1.,0.,0.));
#21489=DIRECTION('center_axis',(-1.,0.,0.));
#21490=DIRECTION('ref_axis',(0.,0.,1.));
#21491=DIRECTION('center_axis',(1.,0.,0.));
#21492=DIRECTION('ref_axis',(0.,0.,-1.));
#21493=DIRECTION('center_axis',(1.,0.,0.));
#21494=DIRECTION('ref_axis',(0.,1.,0.));
#21495=DIRECTION('center_axis',(1.,0.,0.));
#21496=DIRECTION('ref_axis',(0.,0.,-1.));
#21497=DIRECTION('',(-0.707106781186549,0.707106781186546,8.65956056235492E-17));
#21498=DIRECTION('center_axis',(1.,0.,0.));
#21499=DIRECTION('ref_axis',(0.,1.,0.));
#21500=DIRECTION('center_axis',(1.,0.,0.));
#21501=DIRECTION('ref_axis',(0.,0.,-1.));
#21502=DIRECTION('',(-1.,0.,0.));
#21503=DIRECTION('',(-1.,0.,0.));
#21504=DIRECTION('center_axis',(-1.,0.,0.));
#21505=DIRECTION('ref_axis',(0.,1.,0.));
#21506=DIRECTION('center_axis',(1.,0.,0.));
#21507=DIRECTION('ref_axis',(0.,0.,-1.));
#21508=DIRECTION('',(-0.707106781186548,-0.707106781186548,-8.65956056235493E-17));
#21509=DIRECTION('center_axis',(1.,0.,0.));
#21510=DIRECTION('ref_axis',(0.,0.,-1.));
#21511=DIRECTION('axis',(0.,0.,1.));
#21512=DIRECTION('refdir',(1.,0.,0.));
#21513=DIRECTION('center_axis',(-0.707106781186549,0.,-0.707106781186546));
#21514=DIRECTION('ref_axis',(-0.707106781186546,0.,0.707106781186549));
#21515=DIRECTION('',(0.707106781186546,0.,-0.707106781186549));
#21516=DIRECTION('',(0.,1.,0.));
#21517=DIRECTION('',(-0.707106781186546,0.,0.707106781186549));
#21518=DIRECTION('',(0.,-1.,0.));
#21519=DIRECTION('center_axis',(-1.,0.,0.));
#21520=DIRECTION('ref_axis',(0.,0.,1.));
#21521=DIRECTION('',(0.,0.,-1.));
#21522=DIRECTION('',(0.,-1.,0.));
#21523=DIRECTION('',(0.,0.,1.));
#21524=DIRECTION('center_axis',(-0.707106781186549,0.,-0.707106781186546));
#21525=DIRECTION('ref_axis',(-0.707106781186546,0.,0.707106781186549));
#21526=DIRECTION('',(0.707106781186546,0.,-0.707106781186549));
#21527=DIRECTION('',(0.,1.,0.));
#21528=DIRECTION('',(-0.707106781186546,0.,0.707106781186549));
#21529=DIRECTION('',(0.,-1.,0.));
#21530=DIRECTION('center_axis',(-1.,0.,0.));
#21531=DIRECTION('ref_axis',(0.,0.,1.));
#21532=DIRECTION('',(0.,0.,-1.));
#21533=DIRECTION('',(0.,1.,0.));
#21534=DIRECTION('',(0.,0.,1.));
#21535=DIRECTION('center_axis',(0.0563883874434601,0.707106781186547,-0.704854843043252));
#21536=DIRECTION('ref_axis',(-0.996815278536125,0.,-0.07974522228289));
#21537=DIRECTION('',(0.996815278536125,0.,0.07974522228289));
#21538=DIRECTION('',(-0.996835435102578,0.0794928633517165,0.));
#21539=DIRECTION('',(-0.561362850588527,-0.561362850588533,-0.608065374740446));
#21540=DIRECTION('',(-0.996815278536125,0.,-0.07974522228289));
#21541=DIRECTION('',(-0.0282279077199712,0.706825008480088,0.706825008480088));
#21542=DIRECTION('center_axis',(0.,0.707106781186548,-0.707106781186548));
#21543=DIRECTION('ref_axis',(-1.,0.,0.));
#21544=DIRECTION('',(-1.,0.,0.));
#21545=DIRECTION('',(0.,0.707106781186547,0.707106781186547));
#21546=DIRECTION('',(1.,0.,0.));
#21547=DIRECTION('center_axis',(0.,-1.,0.));
#21548=DIRECTION('ref_axis',(0.,0.,-1.));
#21549=DIRECTION('',(0.,0.707106781186547,-0.707106781186548));
#21550=DIRECTION('center_axis',(0.,-1.,0.));
#21551=DIRECTION('ref_axis',(0.,0.,-1.));
#21552=DIRECTION('center_axis',(0.,1.,0.));
#21553=DIRECTION('ref_axis',(0.,0.,-1.));
#21554=DIRECTION('center_axis',(0.,0.707106781186548,0.707106781186548));
#21555=DIRECTION('ref_axis',(1.,0.,0.));
#21556=DIRECTION('',(0.577350269189625,-0.577350269189626,0.577350269189626));
#21557=DIRECTION('',(1.,0.,0.));
#21558=DIRECTION('center_axis',(0.,1.,0.));
#21559=DIRECTION('ref_axis',(1.,0.,0.));
#21560=DIRECTION('',(1.,0.,0.));
#21561=DIRECTION('',(1.,0.,0.));
#21562=DIRECTION('center_axis',(0.,-1.,0.));
#21563=DIRECTION('ref_axis',(1.,0.,0.));
#21564=DIRECTION('center_axis',(0.,-1.,0.));
#21565=DIRECTION('ref_axis',(1.,0.,0.));
#21566=DIRECTION('center_axis',(0.0563883874434601,-0.707106781186547,-0.704854843043252));
#21567=DIRECTION('ref_axis',(-0.996815278536125,0.,-0.07974522228289));
#21568=DIRECTION('',(0.996815278536125,0.,0.07974522228289));
#21569=DIRECTION('',(0.561362850588529,-0.561362850588532,0.608065374740446));
#21570=DIRECTION('',(0.996835435102578,0.0794928633517165,0.));
#21571=DIRECTION('',(-0.996815278536125,0.,-0.07974522228289));
#21572=DIRECTION('',(0.0282279077199586,0.706825008480088,-0.706825008480088));
#21573=DIRECTION('center_axis',(0.,-0.707106781186548,0.707106781186548));
#21574=DIRECTION('ref_axis',(1.,0.,0.));
#21575=DIRECTION('',(-0.577350269189625,-0.577350269189626,-0.577350269189626));
#21576=DIRECTION('',(-1.,0.,0.));
#21577=DIRECTION('',(0.,-0.707106781186547,-0.707106781186547));
#21578=DIRECTION('center_axis',(0.,1.,0.));
#21579=DIRECTION('ref_axis',(0.,0.,-1.));
#21580=DIRECTION('center_axis',(0.,-1.,0.));
#21581=DIRECTION('ref_axis',(0.,0.,-1.));
#21582=DIRECTION('',(0.,-0.707106781186547,0.707106781186547));
#21583=DIRECTION('center_axis',(0.,1.,0.));
#21584=DIRECTION('ref_axis',(0.,0.,-1.));
#21585=DIRECTION('center_axis',(0.,-0.707106781186548,-0.707106781186548));
#21586=DIRECTION('ref_axis',(-1.,0.,0.));
#21587=DIRECTION('',(-1.,0.,0.));
#21588=DIRECTION('',(1.,0.,0.));
#21589=DIRECTION('center_axis',(0.734760240582904,0.,-0.678326904124075));
#21590=DIRECTION('ref_axis',(-0.678326904124075,0.,-0.734760240582904));
#21591=DIRECTION('',(0.,1.,0.));
#21592=DIRECTION('',(0.,1.,0.));
#21593=DIRECTION('',(-0.678326904124075,0.,-0.734760240582904));
#21594=DIRECTION('',(0.,-1.,0.));
#21595=DIRECTION('center_axis',(0.734760240582904,0.,-0.678326904124075));
#21596=DIRECTION('ref_axis',(-0.678326904124075,0.,-0.734760240582904));
#21597=DIRECTION('center_axis',(0.07974522228289,0.,-0.996815278536125));
#21598=DIRECTION('ref_axis',(-0.996815278536125,0.,-0.07974522228289));
#21599=DIRECTION('',(0.,1.,0.));
#21600=DIRECTION('',(-0.996815278536125,0.,-0.07974522228289));
#21601=DIRECTION('center_axis',(0.,0.,-1.));
#21602=DIRECTION('ref_axis',(-1.,0.,0.));
#21603=DIRECTION('',(0.,1.,0.));
#21604=DIRECTION('',(-1.,0.,0.));
#21605=DIRECTION('center_axis',(0.,1.,0.));
#21606=DIRECTION('ref_axis',(0.,0.,-1.));
#21607=DIRECTION('',(0.,1.,0.));
#21608=DIRECTION('center_axis',(0.,1.,0.));
#21609=DIRECTION('ref_axis',(-1.,0.,-6.12323399573677E-17));
#21610=DIRECTION('center_axis',(0.,0.,1.));
#21611=DIRECTION('ref_axis',(1.,0.,0.));
#21612=DIRECTION('',(0.,-1.,0.));
#21613=DIRECTION('',(-1.,0.,0.));
#21614=DIRECTION('',(0.,-1.,0.));
#21615=DIRECTION('',(1.,0.,0.));
#21616=DIRECTION('',(0.,1.,0.));
#21617=DIRECTION('center_axis',(-0.707106781186548,0.,0.707106781186547));
#21618=DIRECTION('ref_axis',(0.707106781186547,0.,0.707106781186548));
#21619=DIRECTION('',(-0.678326904124083,0.,-0.734760240582897));
#21620=DIRECTION('',(0.678326904124076,0.,0.734760240582904));
#21621=DIRECTION('center_axis',(0.734760240582906,0.,-0.678326904124074));
#21622=DIRECTION('ref_axis',(-0.678326904124074,0.,-0.734760240582906));
#21623=DIRECTION('',(0.,1.,0.));
#21624=DIRECTION('center_axis',(0.734760240582906,0.,-0.678326904124074));
#21625=DIRECTION('ref_axis',(-0.678326904124074,0.,-0.734760240582906));
#21626=DIRECTION('',(0.,-1.,0.));
#21627=DIRECTION('',(0.,1.,0.));
#21628=DIRECTION('center_axis',(0.,1.,0.));
#21629=DIRECTION('ref_axis',(1.,0.,0.));
#21630=DIRECTION('',(0.,0.,-1.));
#21631=DIRECTION('',(0.707106781186547,0.,-0.707106781186548));
#21632=DIRECTION('',(1.,0.,0.));
#21633=DIRECTION('center_axis',(0.,1.,0.));
#21634=DIRECTION('ref_axis',(-1.,0.,-6.12323399573677E-17));
#21635=DIRECTION('',(-1.,0.,0.));
#21636=DIRECTION('',(-0.996815278536125,0.,-0.07974522228289));
#21637=DIRECTION('center_axis',(0.,1.,0.));
#21638=DIRECTION('ref_axis',(1.,0.,0.));
#21639=DIRECTION('center_axis',(0.,1.,0.));
#21640=DIRECTION('ref_axis',(1.,0.,0.));
#21641=DIRECTION('center_axis',(0.,0.,1.));
#21642=DIRECTION('ref_axis',(0.707106781186546,-0.707106781186549,0.));
#21643=DIRECTION('',(0.,0.,1.));
#21644=DIRECTION('center_axis',(1.,0.,0.));
#21645=DIRECTION('ref_axis',(0.,0.,-1.));
#21646=DIRECTION('center_axis',(-1.,0.,0.));
#21647=DIRECTION('ref_axis',(0.,0.,-1.));
#21648=DIRECTION('center_axis',(-1.,0.,0.));
#21649=DIRECTION('ref_axis',(0.,0.,-1.));
#21650=DIRECTION('',(0.,0.,-1.));
#21651=DIRECTION('',(0.,1.,0.));
#21652=DIRECTION('',(0.678326904124078,0.,0.734760240582902));
#21653=DIRECTION('center_axis',(-0.996815278536125,0.,-0.07974522228289));
#21654=DIRECTION('ref_axis',(0.0563883874434599,0.707106781186548,-0.704854843043251));
#21655=DIRECTION('center_axis',(-0.999203502429842,0.,-0.0399043948950148));
#21656=DIRECTION('ref_axis',(0.0399043948950148,0.,-0.999203502429842));
#21657=DIRECTION('',(0.996815278536125,0.,0.07974522228289));
#21658=DIRECTION('center_axis',(0.,1.,0.));
#21659=DIRECTION('ref_axis',(1.,0.,0.));
#21660=DIRECTION('',(-1.,0.,0.));
#21661=DIRECTION('',(-1.,0.,0.));
#21662=DIRECTION('center_axis',(0.,1.,0.));
#21663=DIRECTION('ref_axis',(1.,0.,0.));
#21664=DIRECTION('center_axis',(0.,1.,0.));
#21665=DIRECTION('ref_axis',(1.,0.,0.));
#21666=DIRECTION('center_axis',(0.,0.,-1.));
#21667=DIRECTION('ref_axis',(-1.,0.,0.));
#21668=DIRECTION('',(-1.,0.,0.));
#21669=DIRECTION('',(0.,-1.,0.));
#21670=DIRECTION('',(1.,0.,0.));
#21671=DIRECTION('',(-0.707106781186542,0.,0.707106781186553));
#21672=DIRECTION('',(0.707106781186555,0.,-0.70710678118654));
#21673=DIRECTION('center_axis',(0.70710678118655,0.,0.707106781186545));
#21674=DIRECTION('ref_axis',(0.707106781186545,0.,-0.70710678118655));
#21675=DIRECTION('',(0.707106781186539,0.,-0.707106781186556));
#21676=DIRECTION('center_axis',(-1.,0.,0.));
#21677=DIRECTION('ref_axis',(0.,-0.707106781186548,0.707106781186548));
#21678=DIRECTION('center_axis',(1.,0.,0.));
#21679=DIRECTION('ref_axis',(0.,0.,1.));
#21680=DIRECTION('center_axis',(1.,0.,0.));
#21681=DIRECTION('ref_axis',(0.,0.707106781186548,0.707106781186548));
#21682=DIRECTION('',(-1.,0.,0.));
#21683=DIRECTION('center_axis',(-1.,0.,-7.96639400082368E-16));
#21684=DIRECTION('ref_axis',(-7.96639400082368E-16,0.,1.));
#21685=DIRECTION('center_axis',(0.,0.,-1.));
#21686=DIRECTION('ref_axis',(0.707106781186546,0.707106781186549,0.));
#21687=DIRECTION('',(0.,0.,1.));
#21688=DIRECTION('center_axis',(-1.,0.,0.));
#21689=DIRECTION('ref_axis',(0.,0.707106781186548,-0.707106781186548));
#21690=DIRECTION('center_axis',(1.,0.,0.));
#21691=DIRECTION('ref_axis',(0.,0.,-1.));
#21692=DIRECTION('',(1.,0.,0.));
#21693=DIRECTION('center_axis',(0.,1.,0.));
#21694=DIRECTION('ref_axis',(0.,0.,1.));
#21695=DIRECTION('center_axis',(0.,-1.,0.));
#21696=DIRECTION('ref_axis',(-1.,0.,-6.12323399573677E-17));
#21697=DIRECTION('center_axis',(0.,1.,0.));
#21698=DIRECTION('ref_axis',(1.,0.,0.));
#21699=DIRECTION('center_axis',(0.,-1.,0.));
#21700=DIRECTION('ref_axis',(1.,0.,0.));
#21701=DIRECTION('center_axis',(0.,-1.,0.));
#21702=DIRECTION('ref_axis',(1.,0.,0.));
#21703=DIRECTION('center_axis',(0.996815278536125,0.,0.07974522228289));
#21704=DIRECTION('ref_axis',(0.05638838744346,-0.707106781186549,-0.70485484304325));
#21705=DIRECTION('center_axis',(0.999203502429842,0.,0.0399043948950059));
#21706=DIRECTION('ref_axis',(0.0399043948950059,0.,-0.999203502429842));
#21707=DIRECTION('',(0.996815278536125,0.,0.07974522228289));
#21708=DIRECTION('center_axis',(0.,-1.,0.));
#21709=DIRECTION('ref_axis',(0.,0.,-1.));
#21710=DIRECTION('center_axis',(-1.,0.,0.));
#21711=DIRECTION('ref_axis',(0.,0.,-1.));
#21712=DIRECTION('center_axis',(0.,-1.,0.));
#21713=DIRECTION('ref_axis',(-1.,0.,-6.12323399573677E-17));
#21714=DIRECTION('center_axis',(1.,0.,0.));
#21715=DIRECTION('ref_axis',(0.,-0.707106781186548,-0.707106781186548));
#21716=DIRECTION('',(1.,0.,0.));
#21717=DIRECTION('center_axis',(0.,0.,-1.));
#21718=DIRECTION('ref_axis',(1.,0.,0.));
#21719=DIRECTION('',(0.,-1.,0.));
#21720=DIRECTION('',(0.,-1.,0.));
#21721=DIRECTION('center_axis',(0.,-1.,0.));
#21722=DIRECTION('ref_axis',(0.,0.,-1.));
#21723=DIRECTION('center_axis',(0.,1.,0.));
#21724=DIRECTION('ref_axis',(1.,0.,0.));
#21725=DIRECTION('',(0.,1.,0.));
#21726=DIRECTION('center_axis',(0.,1.,0.));
#21727=DIRECTION('ref_axis',(1.,0.,0.));
#21728=DIRECTION('',(0.,1.,0.));
#21729=DIRECTION('center_axis',(0.,1.,0.));
#21730=DIRECTION('ref_axis',(1.,0.,0.));
#21731=DIRECTION('',(0.,1.,0.));
#21732=DIRECTION('center_axis',(0.,1.,0.));
#21733=DIRECTION('ref_axis',(1.,0.,0.));
#21734=DIRECTION('',(0.,1.,0.));
#21735=DIRECTION('center_axis',(1.,0.,0.));
#21736=DIRECTION('ref_axis',(0.,0.,-1.));
#21737=DIRECTION('center_axis',(1.,0.,0.));
#21738=DIRECTION('ref_axis',(0.,0.,-1.));
#21739=DIRECTION('',(-1.,0.,0.));
#21740=DIRECTION('center_axis',(1.,0.,0.));
#21741=DIRECTION('ref_axis',(0.,0.,-1.));
#21742=DIRECTION('center_axis',(0.,-1.,0.));
#21743=DIRECTION('ref_axis',(0.,0.,-1.));
#21744=DIRECTION('center_axis',(0.906307787036649,0.,0.422618261740702));
#21745=DIRECTION('ref_axis',(0.422618261740701,0.,-0.906307787036649));
#21746=DIRECTION('center_axis',(0.,1.,0.));
#21747=DIRECTION('ref_axis',(0.,0.,-1.));
#21748=DIRECTION('center_axis',(0.906307787036649,0.,0.422618261740702));
#21749=DIRECTION('ref_axis',(0.422618261740702,0.,-0.906307787036649));
#21750=DIRECTION('center_axis',(1.,0.,0.));
#21751=DIRECTION('ref_axis',(0.,0.,-1.));
#21752=DIRECTION('center_axis',(0.,0.,-1.));
#21753=DIRECTION('ref_axis',(-1.,0.,0.));
#21754=DIRECTION('center_axis',(0.07974522228289,0.,-0.996815278536125));
#21755=DIRECTION('ref_axis',(0.996815278536125,0.,0.07974522228289));
#21756=DIRECTION('axis',(0.,0.,1.));
#21757=DIRECTION('refdir',(1.,0.,0.));
#21758=DIRECTION('center_axis',(1.,7.63756368739912E-16,0.));
#21759=DIRECTION('ref_axis',(0.,3.0116113276618E-17,-1.));
#21760=DIRECTION('center_axis',(1.,0.,0.));
#21761=DIRECTION('ref_axis',(0.,6.12323399573677E-17,-1.));
#21762=DIRECTION('',(0.923879532511286,7.40959143359019E-16,0.382683432365092));
#21763=DIRECTION('center_axis',(-1.,0.,0.));
#21764=DIRECTION('ref_axis',(0.,0.,-1.));
#21765=DIRECTION('center_axis',(1.,0.,0.));
#21766=DIRECTION('ref_axis',(0.,0.,-1.));
#21767=DIRECTION('',(-0.707106781186546,8.65956056235495E-17,-0.707106781186549));
#21768=DIRECTION('center_axis',(-1.,0.,0.));
#21769=DIRECTION('ref_axis',(0.,6.12323399573677E-17,-1.));
#21770=DIRECTION('center_axis',(1.,0.,0.));
#21771=DIRECTION('ref_axis',(0.,0.,-1.));
#21772=DIRECTION('center_axis',(1.,0.,0.));
#21773=DIRECTION('ref_axis',(0.,0.,-1.));
#21774=DIRECTION('',(-1.,0.,0.));
#21775=DIRECTION('center_axis',(1.,-1.79314445242836E-15,0.));
#21776=DIRECTION('ref_axis',(0.,3.1932434889965E-17,-1.));
#21777=DIRECTION('',(-0.382683432365088,8.28851008028559E-16,-0.923879532511287));
#21778=DIRECTION('center_axis',(1.,0.,0.));
#21779=DIRECTION('ref_axis',(0.,0.,-1.));
#21780=DIRECTION('center_axis',(1.,0.,0.));
#21781=DIRECTION('ref_axis',(0.,0.,-1.));
#21782=DIRECTION('center_axis',(1.,0.,0.));
#21783=DIRECTION('ref_axis',(0.,0.,-1.));
#21784=DIRECTION('center_axis',(0.906307787036649,-6.16297582203915E-33,
0.422618261740701));
#21785=DIRECTION('ref_axis',(0.422618261740702,0.,-0.906307787036649));
#21786=DIRECTION('center_axis',(-0.906307787036649,6.16297582203915E-33,
-0.422618261740701));
#21787=DIRECTION('ref_axis',(2.06315799195206E-17,1.,-4.42445659184577E-17));
#21788=DIRECTION('center_axis',(5.17558101501968E-17,-1.,-1.10990693043675E-16));
#21789=DIRECTION('ref_axis',(-0.422618261740701,-1.22464679914735E-16,0.906307787036649));
#21790=DIRECTION('center_axis',(0.906307787036649,-6.16297582203915E-33,
0.422618261740701));
#21791=DIRECTION('ref_axis',(-1.00929365875014E-16,1.,-1.00929365875014E-16));
#21792=DIRECTION('center_axis',(0.906307787036649,-6.16297582203915E-33,
0.422618261740701));
#21793=DIRECTION('ref_axis',(-1.00929365875014E-16,1.,-1.00929365875014E-16));
#21794=DIRECTION('center_axis',(0.90630778703665,0.,0.422618261740699));
#21795=DIRECTION('ref_axis',(-5.17558101501966E-17,1.,1.10990693043675E-16));
#21796=DIRECTION('',(-0.90630778703665,0.,-0.422618261740699));
#21797=DIRECTION('center_axis',(0.906307787036649,0.,0.422618261740702));
#21798=DIRECTION('ref_axis',(0.422618261740702,0.,-0.906307787036649));
#21799=DIRECTION('center_axis',(0.906307787036649,0.,0.422618261740702));
#21800=DIRECTION('ref_axis',(0.422618261740702,0.,-0.906307787036649));
#21801=DIRECTION('center_axis',(-0.906307787036649,6.16297582203915E-33,
-0.422618261740701));
#21802=DIRECTION('ref_axis',(-5.17558101501968E-17,1.,1.10990693043675E-16));
#21803=DIRECTION('center_axis',(-0.906307787036649,6.16297582203915E-33,
-0.422618261740701));
#21804=DIRECTION('ref_axis',(-5.17558101501968E-17,1.,1.10990693043675E-16));
#21805=DIRECTION('center_axis',(-0.906307787036649,0.,-0.422618261740702));
#21806=DIRECTION('ref_axis',(0.422618261740701,0.,-0.906307787036649));
#21807=DIRECTION('center_axis',(0.,-1.,0.));
#21808=DIRECTION('ref_axis',(0.,0.,-1.));
#21809=DIRECTION('center_axis',(1.,0.,0.));
#21810=DIRECTION('ref_axis',(0.,0.,-1.));
#21811=DIRECTION('center_axis',(0.,-1.,0.));
#21812=DIRECTION('ref_axis',(0.,0.,-1.));
#21813=DIRECTION('center_axis',(1.,0.,0.));
#21814=DIRECTION('ref_axis',(0.,0.,-1.));
#21815=DIRECTION('',(1.,0.,0.));
#21816=DIRECTION('center_axis',(0.,-1.,0.));
#21817=DIRECTION('ref_axis',(0.,0.,-1.));
#21818=DIRECTION('center_axis',(0.,1.,0.));
#21819=DIRECTION('ref_axis',(0.,0.,-1.));
#21820=DIRECTION('axis',(0.,0.,1.));
#21821=DIRECTION('refdir',(1.,0.,0.));
#21822=DIRECTION('center_axis',(0.,1.,0.));
#21823=DIRECTION('ref_axis',(1.,0.,0.));
#21824=DIRECTION('',(-0.707106781186548,0.707106781186548,-8.65956056235495E-17));
#21825=DIRECTION('center_axis',(0.,-1.,0.));
#21826=DIRECTION('ref_axis',(1.,0.,0.));
#21827=DIRECTION('',(-0.707106781186548,-0.707106781186548,0.));
#21828=DIRECTION('center_axis',(0.,1.,0.));
#21829=DIRECTION('ref_axis',(1.,0.,0.));
#21830=DIRECTION('center_axis',(-0.707106781186548,-0.707106781186548,0.));
#21831=DIRECTION('ref_axis',(0.,0.,1.));
#21832=DIRECTION('',(-0.707106781186548,0.707106781186548,0.));
#21833=DIRECTION('',(0.,0.,-1.));
#21834=DIRECTION('',(0.,0.,1.));
#21835=DIRECTION('center_axis',(0.,1.,0.));
#21836=DIRECTION('ref_axis',(-1.,0.,0.));
#21837=DIRECTION('',(0.707106781186548,0.707106781186548,0.));
#21838=DIRECTION('center_axis',(0.,-1.,0.));
#21839=DIRECTION('ref_axis',(-1.,0.,0.));
#21840=DIRECTION('center_axis',(0.,1.,0.));
#21841=DIRECTION('ref_axis',(-1.,0.,0.));
#21842=DIRECTION('center_axis',(0.707106781186548,-0.707106781186548,0.));
#21843=DIRECTION('ref_axis',(0.,0.,-1.));
#21844=DIRECTION('',(0.,0.,1.));
#21845=DIRECTION('',(0.,0.,-1.));
#21846=DIRECTION('center_axis',(1.,0.,0.));
#21847=DIRECTION('ref_axis',(0.,0.,-1.));
#21848=DIRECTION('',(0.,1.,0.));
#21849=DIRECTION('',(0.,0.,-1.));
#21850=DIRECTION('',(0.,1.,0.));
#21851=DIRECTION('center_axis',(0.,1.,0.));
#21852=DIRECTION('ref_axis',(1.,0.,0.));
#21853=DIRECTION('',(0.,1.,0.));
#21854=DIRECTION('center_axis',(0.,1.,0.));
#21855=DIRECTION('ref_axis',(1.,0.,0.));
#21856=DIRECTION('center_axis',(0.,1.,0.));
#21857=DIRECTION('ref_axis',(1.,0.,0.));
#21858=DIRECTION('center_axis',(0.,1.,0.));
#21859=DIRECTION('ref_axis',(1.,0.,0.));
#21860=DIRECTION('center_axis',(0.,1.,0.));
#21861=DIRECTION('ref_axis',(1.,0.,0.));
#21862=DIRECTION('center_axis',(0.923879532511287,0.382683432365089,0.));
#21863=DIRECTION('ref_axis',(0.,0.,-1.));
#21864=DIRECTION('',(-0.382683432365089,0.923879532511287,0.));
#21865=DIRECTION('',(0.,0.,1.));
#21866=DIRECTION('',(0.382683432365089,-0.923879532511287,0.));
#21867=DIRECTION('center_axis',(0.,-1.,-1.0507089630694E-15));
#21868=DIRECTION('ref_axis',(1.,0.,-3.02510519985914E-17));
#21869=DIRECTION('',(0.382683432365089,0.923879532511287,4.68652040532631E-17));
#21870=DIRECTION('center_axis',(0.,-1.,0.));
#21871=DIRECTION('ref_axis',(1.,0.,-6.12323399573676E-17));
#21872=DIRECTION('center_axis',(-0.923879532511287,0.382683432365089,0.));
#21873=DIRECTION('ref_axis',(0.,0.,1.));
#21874=DIRECTION('',(0.382683432365089,0.923879532511287,0.));
#21875=DIRECTION('',(0.,0.,-1.));
#21876=DIRECTION('',(0.,0.,1.));
#21877=DIRECTION('center_axis',(0.,-1.,0.));
#21878=DIRECTION('ref_axis',(-1.,0.,0.));
#21879=DIRECTION('center_axis',(0.,-1.,0.));
#21880=DIRECTION('ref_axis',(-1.,0.,0.));
#21881=DIRECTION('center_axis',(0.,1.,0.));
#21882=DIRECTION('ref_axis',(-1.,0.,0.));
#21883=DIRECTION('center_axis',(0.,-1.,0.));
#21884=DIRECTION('ref_axis',(-1.,0.,0.));
#21885=DIRECTION('',(0.707106781186548,-0.707106781186548,0.));
#21886=DIRECTION('center_axis',(0.,1.,0.));
#21887=DIRECTION('ref_axis',(-1.,0.,0.));
#21888=DIRECTION('',(0.707106781186548,0.707106781186548,0.));
#21889=DIRECTION('center_axis',(0.707106781186548,0.707106781186548,0.));
#21890=DIRECTION('ref_axis',(0.,0.,-1.));
#21891=DIRECTION('',(-0.707106781186548,0.707106781186548,0.));
#21892=DIRECTION('',(0.,0.,-1.));
#21893=DIRECTION('center_axis',(0.382683432365093,0.923879532511286,0.));
#21894=DIRECTION('ref_axis',(0.,0.,1.));
#21895=DIRECTION('',(0.923879532511286,-0.382683432365093,0.));
#21896=DIRECTION('',(-0.923879532511286,0.382683432365093,0.));
#21897=DIRECTION('',(0.,0.,1.));
#21898=DIRECTION('center_axis',(0.,-1.,0.));
#21899=DIRECTION('ref_axis',(-1.,0.,0.));
#21900=DIRECTION('',(-0.923879532511286,-0.38268343236509,-6.00848371219648E-15));
#21901=DIRECTION('center_axis',(0.,-1.,0.));
#21902=DIRECTION('ref_axis',(-1.,0.,0.));
#21903=DIRECTION('center_axis',(-0.382683432365093,0.923879532511286,0.));
#21904=DIRECTION('ref_axis',(0.,0.,1.));
#21905=DIRECTION('',(-0.923879532511286,-0.382683432365093,1.10160925113079E-15));
#21906=DIRECTION('',(0.,0.,1.));
#21907=DIRECTION('',(0.,0.,-1.));
#21908=DIRECTION('center_axis',(0.,-1.,2.48590929741676E-15));
#21909=DIRECTION('ref_axis',(1.,0.,-3.15543818946224E-17));
#21910=DIRECTION('center_axis',(0.,1.,0.));
#21911=DIRECTION('ref_axis',(1.,0.,-6.12323399573677E-17));
#21912=DIRECTION('center_axis',(0.,-1.,0.));
#21913=DIRECTION('ref_axis',(1.,0.,0.));
#21914=DIRECTION('center_axis',(0.,-1.,0.));
#21915=DIRECTION('ref_axis',(1.,0.,0.));
#21916=DIRECTION('',(0.707106781186548,0.707106781186548,8.65956056235493E-17));
#21917=DIRECTION('center_axis',(0.,1.,0.));
#21918=DIRECTION('ref_axis',(1.,0.,0.));
#21919=DIRECTION('center_axis',(0.,-1.,0.));
#21920=DIRECTION('ref_axis',(1.,0.,0.));
#21921=DIRECTION('center_axis',(0.,-1.,0.));
#21922=DIRECTION('ref_axis',(1.,0.,0.));
#21923=DIRECTION('center_axis',(-0.707106781186548,0.707106781186548,0.));
#21924=DIRECTION('ref_axis',(0.,0.,1.));
#21925=DIRECTION('center_axis',(0.,1.,0.));
#21926=DIRECTION('ref_axis',(1.,0.,0.));
#21927=DIRECTION('',(0.,1.,0.));
#21928=DIRECTION('center_axis',(0.,1.,0.));
#21929=DIRECTION('ref_axis',(1.,0.,0.));
#21930=DIRECTION('',(0.,1.,0.));
#21931=DIRECTION('center_axis',(0.,1.,0.));
#21932=DIRECTION('ref_axis',(-1.,0.,0.));
#21933=DIRECTION('',(0.,1.,0.));
#21934=DIRECTION('center_axis',(-1.,0.,0.));
#21935=DIRECTION('ref_axis',(0.,0.,1.));
#21936=DIRECTION('axis',(0.,0.,1.));
#21937=DIRECTION('refdir',(1.,0.,0.));
#21938=DIRECTION('center_axis',(-1.,0.,0.));
#21939=DIRECTION('ref_axis',(0.,0.,1.));
#21940=DIRECTION('center_axis',(1.,0.,0.));
#21941=DIRECTION('ref_axis',(0.,0.,-1.));
#21942=DIRECTION('center_axis',(1.,0.,0.));
#21943=DIRECTION('ref_axis',(0.,1.,0.));
#21944=DIRECTION('center_axis',(1.,0.,0.));
#21945=DIRECTION('ref_axis',(0.,0.,-1.));
#21946=DIRECTION('',(-0.707106781186548,0.707106781186547,8.65956056235493E-17));
#21947=DIRECTION('center_axis',(1.,0.,0.));
#21948=DIRECTION('ref_axis',(0.,1.,0.));
#21949=DIRECTION('center_axis',(1.,0.,0.));
#21950=DIRECTION('ref_axis',(0.,0.,-1.));
#21951=DIRECTION('',(-1.,0.,0.));
#21952=DIRECTION('center_axis',(1.,0.,0.));
#21953=DIRECTION('ref_axis',(0.,0.,-1.));
#21954=DIRECTION('center_axis',(1.,0.,0.));
#21955=DIRECTION('ref_axis',(0.,0.,-1.));
#21956=DIRECTION('center_axis',(1.,0.,0.));
#21957=DIRECTION('ref_axis',(0.,1.,0.));
#21958=DIRECTION('center_axis',(1.,0.,0.));
#21959=DIRECTION('ref_axis',(0.,0.,-1.));
#21960=DIRECTION('',(-1.,0.,0.));
#21961=DIRECTION('center_axis',(-1.,0.,0.));
#21962=DIRECTION('ref_axis',(0.,0.,1.));
#21963=DIRECTION('center_axis',(1.,0.,0.));
#21964=DIRECTION('ref_axis',(0.,0.,-1.));
#21965=DIRECTION('center_axis',(1.,0.,0.));
#21966=DIRECTION('ref_axis',(0.,1.,0.));
#21967=DIRECTION('center_axis',(1.,0.,0.));
#21968=DIRECTION('ref_axis',(0.,0.,-1.));
#21969=DIRECTION('',(-1.,0.,0.));
#21970=DIRECTION('center_axis',(1.,0.,0.));
#21971=DIRECTION('ref_axis',(0.,0.,-1.));
#21972=DIRECTION('center_axis',(1.,0.,0.));
#21973=DIRECTION('ref_axis',(0.,0.,-1.));
#21974=DIRECTION('center_axis',(1.,0.,0.));
#21975=DIRECTION('ref_axis',(0.,1.,0.));
#21976=DIRECTION('center_axis',(1.,0.,0.));
#21977=DIRECTION('ref_axis',(0.,0.,-1.));
#21978=DIRECTION('',(-1.,0.,0.));
#21979=DIRECTION('center_axis',(-1.,0.,0.));
#21980=DIRECTION('ref_axis',(0.,0.,1.));
#21981=DIRECTION('center_axis',(1.,0.,0.));
#21982=DIRECTION('ref_axis',(0.,0.,-1.));
#21983=DIRECTION('center_axis',(1.,0.,0.));
#21984=DIRECTION('ref_axis',(0.,1.,0.));
#21985=DIRECTION('center_axis',(1.,0.,0.));
#21986=DIRECTION('ref_axis',(0.,0.,-1.));
#21987=DIRECTION('',(-1.,0.,0.));
#21988=DIRECTION('center_axis',(-1.,0.,0.));
#21989=DIRECTION('ref_axis',(0.,1.,0.));
#21990=DIRECTION('center_axis',(1.,0.,0.));
#21991=DIRECTION('ref_axis',(0.,0.,-1.));
#21992=DIRECTION('',(-0.707106781186548,-0.707106781186547,-8.65956056235493E-17));
#21993=DIRECTION('center_axis',(1.,0.,0.));
#21994=DIRECTION('ref_axis',(0.,0.,-1.));
#21995=DIRECTION('axis',(0.,0.,1.));
#21996=DIRECTION('refdir',(1.,0.,0.));
#21997=DIRECTION('center_axis',(0.,-1.,0.));
#21998=DIRECTION('ref_axis',(1.,0.,0.));
#21999=DIRECTION('center_axis',(0.,-1.,0.));
#22000=DIRECTION('ref_axis',(1.,0.,0.));
#22001=DIRECTION('center_axis',(0.,1.,0.));
#22002=DIRECTION('ref_axis',(1.,0.,0.));
#22003=DIRECTION('center_axis',(0.,0.707106781186548,0.707106781186547));
#22004=DIRECTION('ref_axis',(1.,0.,0.));
#22005=DIRECTION('',(-1.,0.,0.));
#22006=DIRECTION('',(-0.577350269189626,-0.577350269189626,0.577350269189626));
#22007=DIRECTION('',(1.,0.,0.));
#22008=DIRECTION('center_axis',(-0.707106781186547,0.707106781186548,0.));
#22009=DIRECTION('ref_axis',(0.,0.,1.));
#22010=DIRECTION('',(0.,0.,-1.));
#22011=DIRECTION('',(-0.577350269189626,-0.577350269189626,-0.577350269189626));
#22012=DIRECTION('',(0.,0.,1.));
#22013=DIRECTION('center_axis',(0.,0.707106781186548,-0.707106781186547));
#22014=DIRECTION('ref_axis',(-1.,0.,0.));
#22015=DIRECTION('',(-1.,0.,0.));
#22016=DIRECTION('',(1.,0.,0.));
#22017=DIRECTION('center_axis',(0.,0.,-1.));
#22018=DIRECTION('ref_axis',(-1.,0.,0.));
#22019=DIRECTION('',(0.,1.,0.));
#22020=DIRECTION('',(1.,0.,0.));
#22021=DIRECTION('',(0.,1.,0.));
#22022=DIRECTION('center_axis',(0.,1.,0.));
#22023=DIRECTION('ref_axis',(1.,0.,0.));
#22024=DIRECTION('',(0.,1.,0.));
#22025=DIRECTION('center_axis',(0.,-1.,0.));
#22026=DIRECTION('ref_axis',(1.,0.,0.));
#22027=DIRECTION('center_axis',(0.,1.,0.));
#22028=DIRECTION('ref_axis',(1.,0.,0.));
#22029=DIRECTION('center_axis',(0.,-1.,0.));
#22030=DIRECTION('ref_axis',(1.,0.,0.));
#22031=DIRECTION('center_axis',(0.,1.,0.));
#22032=DIRECTION('ref_axis',(1.,0.,0.));
#22033=DIRECTION('center_axis',(0.,1.,0.));
#22034=DIRECTION('ref_axis',(1.,0.,0.));
#22035=DIRECTION('center_axis',(0.,-0.707106781186548,-0.707106781186547));
#22036=DIRECTION('ref_axis',(-1.,0.,0.));
#22037=DIRECTION('',(-1.,0.,0.));
#22038=DIRECTION('',(-0.577350269189626,0.577350269189625,-0.577350269189626));
#22039=DIRECTION('center_axis',(-0.707106781186547,-0.707106781186548,0.));
#22040=DIRECTION('ref_axis',(0.,0.,1.));
#22041=DIRECTION('',(0.,0.,1.));
#22042=DIRECTION('',(-0.577350269189626,0.577350269189625,0.577350269189626));
#22043=DIRECTION('',(0.,0.,-1.));
#22044=DIRECTION('center_axis',(0.,-0.707106781186548,0.707106781186547));
#22045=DIRECTION('ref_axis',(1.,0.,0.));
#22046=DIRECTION('',(-1.,0.,0.));
#22047=DIRECTION('',(1.,0.,0.));
#22048=DIRECTION('center_axis',(0.,0.,1.));
#22049=DIRECTION('ref_axis',(1.,0.,0.));
#22050=DIRECTION('',(0.,1.,0.));
#22051=DIRECTION('center_axis',(0.,1.,0.));
#22052=DIRECTION('ref_axis',(1.,0.,0.));
#22053=DIRECTION('center_axis',(0.,1.,0.));
#22054=DIRECTION('ref_axis',(1.,0.,0.));
#22055=DIRECTION('center_axis',(0.,1.,0.));
#22056=DIRECTION('ref_axis',(1.,0.,0.));
#22057=DIRECTION('',(0.,1.,0.));
#22058=DIRECTION('center_axis',(-1.,0.,0.));
#22059=DIRECTION('ref_axis',(0.,0.,1.));
#22060=DIRECTION('center_axis',(-1.,0.,0.));
#22061=DIRECTION('ref_axis',(0.,1.,0.));
#22062=DIRECTION('center_axis',(-1.,0.,0.));
#22063=DIRECTION('ref_axis',(0.,0.,1.));
#22064=DIRECTION('center_axis',(1.,0.,0.));
#22065=DIRECTION('ref_axis',(0.,0.,-1.));
#22066=DIRECTION('center_axis',(1.,0.,0.));
#22067=DIRECTION('ref_axis',(0.,1.,0.));
#22068=DIRECTION('center_axis',(1.,0.,0.));
#22069=DIRECTION('ref_axis',(0.,0.,-1.));
#22070=DIRECTION('',(-0.707106781186546,0.707106781186549,8.65956056235495E-17));
#22071=DIRECTION('center_axis',(1.,0.,0.));
#22072=DIRECTION('ref_axis',(0.,1.,0.));
#22073=DIRECTION('',(-1.,0.,0.));
#22074=DIRECTION('axis',(0.,0.,1.));
#22075=DIRECTION('refdir',(1.,0.,0.));
#22076=DIRECTION('center_axis',(1.,0.,0.));
#22077=DIRECTION('ref_axis',(0.,-8.07434927000114E-16,-1.));
#22078=DIRECTION('center_axis',(1.,0.,0.));
#22079=DIRECTION('ref_axis',(0.,-0.418181818181818,0.908363345221586));
#22080=DIRECTION('',(1.,0.,0.));
#22081=DIRECTION('center_axis',(1.,0.,0.));
#22082=DIRECTION('ref_axis',(0.,-0.418181818181818,0.908363345221586));
#22083=DIRECTION('',(1.,0.,0.));
#22084=DIRECTION('center_axis',(0.,1.,0.));
#22085=DIRECTION('ref_axis',(0.,0.,1.));
#22086=DIRECTION('',(0.,0.,-1.));
#22087=DIRECTION('',(0.,0.,1.));
#22088=DIRECTION('',(1.,0.,0.));
#22089=DIRECTION('center_axis',(1.,0.,0.));
#22090=DIRECTION('ref_axis',(0.,-1.11022302462516E-16,-1.));
#22091=DIRECTION('center_axis',(1.,0.,0.));
#22092=DIRECTION('ref_axis',(0.,-0.92,0.391918358845309));
#22093=DIRECTION('center_axis',(-1.,0.,0.));
#22094=DIRECTION('ref_axis',(0.,-0.92,0.391918358845309));
#22095=DIRECTION('',(1.,0.,0.));
#22096=DIRECTION('center_axis',(0.,-1.,0.));
#22097=DIRECTION('ref_axis',(0.,0.,-1.));
#22098=DIRECTION('',(0.,0.,-1.));
#22099=DIRECTION('',(0.,0.,-1.));
#22100=DIRECTION('center_axis',(1.,0.,0.));
#22101=DIRECTION('ref_axis',(0.,0.,-1.));
#22102=DIRECTION('center_axis',(1.,0.,0.));
#22103=DIRECTION('ref_axis',(0.,0.,-1.));
#22104=DIRECTION('',(0.,0.,1.));
#22105=DIRECTION('',(1.,0.,0.));
#22106=DIRECTION('',(0.,0.,1.));
#22107=DIRECTION('',(1.,0.,0.));
#22108=DIRECTION('',(0.,0.,1.));
#22109=DIRECTION('',(1.,0.,0.));
#22110=DIRECTION('',(0.,0.,1.));
#22111=DIRECTION('',(1.,0.,0.));
#22112=DIRECTION('',(0.,0.,1.));
#22113=DIRECTION('',(1.,0.,0.));
#22114=DIRECTION('',(0.,0.,1.));
#22115=DIRECTION('',(1.,0.,0.));
#22116=DIRECTION('',(0.,0.,1.));
#22117=DIRECTION('',(1.,0.,0.));
#22118=DIRECTION('',(0.,0.,1.));
#22119=DIRECTION('',(1.,0.,0.));
#22120=DIRECTION('',(0.,0.,1.));
#22121=DIRECTION('',(1.,0.,0.));
#22122=DIRECTION('',(0.,0.,1.));
#22123=DIRECTION('',(1.,0.,0.));
#22124=DIRECTION('',(0.,0.,1.));
#22125=DIRECTION('',(-1.,0.,0.));
#22126=DIRECTION('',(1.,0.,0.));
#22127=DIRECTION('',(0.,1.,0.));
#22128=DIRECTION('',(1.,0.,0.));
#22129=DIRECTION('',(0.,1.,0.));
#22130=DIRECTION('',(-1.,0.,0.));
#22131=DIRECTION('',(0.,-1.,0.));
#22132=DIRECTION('',(0.,0.,1.));
#22133=DIRECTION('',(1.,0.,0.));
#22134=DIRECTION('',(0.,0.,1.));
#22135=DIRECTION('',(1.,0.,0.));
#22136=DIRECTION('',(0.,0.,1.));
#22137=DIRECTION('',(1.,0.,0.));
#22138=DIRECTION('',(0.,0.,1.));
#22139=DIRECTION('',(1.,0.,0.));
#22140=DIRECTION('',(0.,0.,1.));
#22141=DIRECTION('',(0.,-1.,0.));
#22142=DIRECTION('',(-0.207911690817759,0.,0.978147600733806));
#22143=DIRECTION('',(0.978147600733806,0.,0.207911690817759));
#22144=DIRECTION('',(-0.207911690817759,0.,0.978147600733806));
#22145=DIRECTION('',(0.978147600733806,0.,0.207911690817759));
#22146=DIRECTION('',(-0.00367694407646724,0.,0.99999324001828));
#22147=DIRECTION('',(0.99999324001828,0.,0.00367694407646724));
#22148=DIRECTION('',(-0.00367694407646724,0.,0.99999324001828));
#22149=DIRECTION('',(-0.99999324001828,0.,-0.00367694407646724));
#22150=DIRECTION('',(1.,0.,0.));
#22151=DIRECTION('',(0.,1.,0.));
#22152=DIRECTION('',(1.,0.,0.));
#22153=DIRECTION('',(0.,1.,0.));
#22154=DIRECTION('',(-1.,0.,0.));
#22155=DIRECTION('',(0.,0.,1.));
#22156=DIRECTION('',(1.,0.,0.));
#22157=DIRECTION('',(0.,1.,0.));
#22158=DIRECTION('',(-1.,0.,0.));
#22159=DIRECTION('',(0.,-1.,0.));
#22160=DIRECTION('',(1.,0.,0.));
#22161=DIRECTION('',(0.,1.,0.));
#22162=DIRECTION('',(-1.,0.,0.));
#22163=DIRECTION('',(0.,-1.,0.));
#22164=CARTESIAN_POINT('',(0.,0.,0.));
#22165=CARTESIAN_POINT('',(0.,0.,0.));
#22166=CARTESIAN_POINT('Origin',(67.75,0.,0.));
#22167=CARTESIAN_POINT('',(67.5,15.2,-1.86146313470398E-15));
#22168=CARTESIAN_POINT('',(67.5,-15.2,-1.86146313470398E-15));
#22169=CARTESIAN_POINT('Origin',(67.5,0.,0.));
#22170=CARTESIAN_POINT('Origin',(67.5,0.,0.));
#22171=CARTESIAN_POINT('',(68.,15.7,1.92269547466134E-15));
#22172=CARTESIAN_POINT('',(67.75,15.45,-1.89207930468266E-15));
#22173=CARTESIAN_POINT('Origin',(68.,0.,0.));
#22174=CARTESIAN_POINT('Origin',(63.95,0.,0.));
#22175=CARTESIAN_POINT('',(60.5,-15.2,-1.86146313470398E-15));
#22176=CARTESIAN_POINT('Origin',(60.5,0.,0.));
#22177=CARTESIAN_POINT('',(63.95,-15.2,-1.86146313470398E-15));
#22178=CARTESIAN_POINT('Origin',(68.,21.05,0.));
#22179=CARTESIAN_POINT('',(68.,-21.05,-2.57788151220518E-15));
#22180=CARTESIAN_POINT('Origin',(68.,0.,0.));
#22181=CARTESIAN_POINT('Origin',(60.25,0.,0.));
#22182=CARTESIAN_POINT('',(60.,-15.7,1.92269547466134E-15));
#22183=CARTESIAN_POINT('Origin',(60.,0.,0.));
#22184=CARTESIAN_POINT('',(60.25,-15.45,1.89207930468266E-15));
#22185=CARTESIAN_POINT('Origin',(60.,-22.,21.));
#22186=CARTESIAN_POINT('',(60.,-20.5,15.1657508881031));
#22187=CARTESIAN_POINT('',(60.,-20.5,-15.1657508881031));
#22188=CARTESIAN_POINT('Origin',(60.,0.,0.));
#22189=CARTESIAN_POINT('',(60.,-20.5,18.));
#22190=CARTESIAN_POINT('',(60.,-20.5,14.75));
#22191=CARTESIAN_POINT('',(60.,20.5,18.));
#22192=CARTESIAN_POINT('',(60.,-22.,18.));
#22193=CARTESIAN_POINT('',(60.,20.5,15.1657508881031));
#22194=CARTESIAN_POINT('',(60.,20.5,14.75));
#22195=CARTESIAN_POINT('',(60.,20.5,-15.1657508881031));
#22196=CARTESIAN_POINT('Origin',(60.,0.,0.));
#22197=CARTESIAN_POINT('',(60.,20.5,-23.5));
#22198=CARTESIAN_POINT('',(60.,20.5,14.75));
#22199=CARTESIAN_POINT('',(60.,9.89949493661168,-23.5));
#22200=CARTESIAN_POINT('',(60.,-22.,-23.5));
#22201=CARTESIAN_POINT('',(60.,-9.89949493661168,-23.5));
#22202=CARTESIAN_POINT('Origin',(60.,0.,0.));
#22203=CARTESIAN_POINT('',(60.,-20.5,-23.5));
#22204=CARTESIAN_POINT('',(60.,-22.,-23.5));
#22205=CARTESIAN_POINT('',(60.,-20.5,14.75));
#22206=CARTESIAN_POINT('Ctrl Pts',(82.590926702435,-21.9972415752925,20.7125564066551));
#22207=CARTESIAN_POINT('Ctrl Pts',(82.5858557493431,-21.9975495316373,20.7099530188172));
#22208=CARTESIAN_POINT('Ctrl Pts',(82.5486931024459,-21.9996721521972,20.6909216201026));
#22209=CARTESIAN_POINT('Ctrl Pts',(82.50785454155,-21.9999804809794,20.67010294536));
#22210=CARTESIAN_POINT('Ctrl Pts',(82.501271349331,-22.,20.6667379107389));
#22211=CARTESIAN_POINT('Ctrl Pts',(82.5,-22.,20.6660888779603));
#22212=CARTESIAN_POINT('Ctrl Pts',(82.4384034141267,-21.9972415752925,21.0089380321363));
#22213=CARTESIAN_POINT('Ctrl Pts',(82.4333341469195,-21.9975495316373,21.0063313683053));
#22214=CARTESIAN_POINT('Ctrl Pts',(82.3962094533413,-21.9996721521972,20.9872262191064));
#22215=CARTESIAN_POINT('Ctrl Pts',(82.3554097305465,-21.9999804809794,20.9663320745804));
#22216=CARTESIAN_POINT('Ctrl Pts',(82.3488347923165,-22.,20.9629510008961));
#22217=CARTESIAN_POINT('Ctrl Pts',(82.3475648606009,-22.,20.9622992134222));
#22218=CARTESIAN_POINT('Ctrl Pts',(82.2858801258184,-21.9972415752925,21.3053196576175));
#22219=CARTESIAN_POINT('Ctrl Pts',(82.2808125444959,-21.9975495316373,21.3027097177933));
#22220=CARTESIAN_POINT('Ctrl Pts',(82.2435888727419,-21.9998742837272,21.2834663188746));
#22221=CARTESIAN_POINT('Ctrl Pts',(82.2029573746821,-21.9998618848641,21.2625298670686));
#22222=CARTESIAN_POINT('Ctrl Pts',(82.1963982353019,-22.,21.2591640910533));
#22223=CARTESIAN_POINT('Ctrl Pts',(82.1951297212018,-22.,21.2585095488841));
#22224=CARTESIAN_POINT('Ctrl Pts',(82.1333568375101,-21.9972415752925,21.6017012830987));
#22225=CARTESIAN_POINT('Ctrl Pts',(82.1282909420722,-21.9975495316373,21.5990880672814));
#22226=CARTESIAN_POINT('Ctrl Pts',(82.091204106178,-21.9996721521972,21.5799093534353));
#22227=CARTESIAN_POINT('Ctrl Pts',(82.0505263223446,-21.9999804809794,21.5587782584214));
#22228=CARTESIAN_POINT('Ctrl Pts',(82.0439616782873,-22.,21.5553771812105));
#22229=CARTESIAN_POINT('Ctrl Pts',(82.0426945818027,-22.,21.5547198843461));
#22230=CARTESIAN_POINT('',(82.5,-22.,20.6660888779603));
#22231=CARTESIAN_POINT('',(82.590926702435,-21.9972415752925,20.7125564066551));
#22232=CARTESIAN_POINT('Ctrl Pts',(82.5,-22.,20.6660888779603));
#22233=CARTESIAN_POINT('Ctrl Pts',(82.5004067990554,-22.,20.6662965517403));
#22234=CARTESIAN_POINT('Ctrl Pts',(82.5008176675242,-21.9999998627569,20.6665063022388));
#22235=CARTESIAN_POINT('Ctrl Pts',(82.5013244717933,-21.999999415258,20.6667650014162));
#22236=CARTESIAN_POINT('Ctrl Pts',(82.5018565166204,-21.9999989454723,20.6670365846832));
#22237=CARTESIAN_POINT('Ctrl Pts',(82.5024940302811,-21.999998138627,20.66736198041));
#22238=CARTESIAN_POINT('Ctrl Pts',(82.5032915692446,-21.9999963885196,20.6677690202808));
#22239=CARTESIAN_POINT('Ctrl Pts',(82.5041416635429,-21.9999945230856,20.6682028828117));
#22240=CARTESIAN_POINT('Ctrl Pts',(82.5051732101651,-21.9999915806081,20.6687293210895));
#22241=CARTESIAN_POINT('Ctrl Pts',(82.5063995751958,-21.999986348417,20.6693551496543));
#22242=CARTESIAN_POINT('Ctrl Pts',(82.507755571728,-21.9999805631631,20.670047130706));
#22243=CARTESIAN_POINT('Ctrl Pts',(82.5093492283813,-21.9999719358723,20.6708603579249));
#22244=CARTESIAN_POINT('Ctrl Pts',(82.5111426325031,-21.9999586133427,20.6717754884718));
#22245=CARTESIAN_POINT('Ctrl Pts',(82.513410125303,-21.9999417689853,20.6729325349515));
#22246=CARTESIAN_POINT('Ctrl Pts',(82.5159957629321,-21.9999172338468,20.6742518848847));
#22247=CARTESIAN_POINT('Ctrl Pts',(82.5187474241439,-21.9998828401205,20.6756559568456));
#22248=CARTESIAN_POINT('Ctrl Pts',(82.5215924246102,-21.9998472797227,20.6771076564103));
#22249=CARTESIAN_POINT('Ctrl Pts',(82.5246090085712,-21.9998011397234,20.6786469157951));
#22250=CARTESIAN_POINT('Ctrl Pts',(82.5276188168876,-21.9997457120971,20.6801828101603));
#22251=CARTESIAN_POINT('Ctrl Pts',(82.5299271169217,-21.9997032032135,20.6813607273707));
#22252=CARTESIAN_POINT('Ctrl Pts',(82.5322304291706,-21.9996553791226,20.682536154127));
#22253=CARTESIAN_POINT('Ctrl Pts',(82.5344785448382,-21.9996036909617,20.683683526565));
#22254=CARTESIAN_POINT('Ctrl Pts',(82.5365092227467,-21.99955700208,20.6847199251347));
#22255=CARTESIAN_POINT('Ctrl Pts',(82.5384943595416,-21.999507235319,20.6857331752724));
#22256=CARTESIAN_POINT('Ctrl Pts',(82.5404338840481,-21.9994549346415,20.6867233017257));
#22257=CARTESIAN_POINT('Ctrl Pts',(82.5422858572142,-21.999404994849,20.6876687332562));
#22258=CARTESIAN_POINT('Ctrl Pts',(82.5440957471635,-21.9993528090371,20.688592827636));
#22259=CARTESIAN_POINT('Ctrl Pts',(82.5459062201873,-21.9992973750888,20.6895174394503));
#22260=CARTESIAN_POINT('Ctrl Pts',(82.5477357383858,-21.9992413580059,20.6904517776694));
#22261=CARTESIAN_POINT('Ctrl Pts',(82.5495738565317,-21.9991817713915,20.6913907373888));
#22262=CARTESIAN_POINT('Ctrl Pts',(82.5514571369584,-21.9991171278643,20.6923530411313));
#22263=CARTESIAN_POINT('Ctrl Pts',(82.5534832655573,-21.9990475810791,20.6933883363034));
#22264=CARTESIAN_POINT('Ctrl Pts',(82.5555612172577,-21.9989721343396,20.6944504217446));
#22265=CARTESIAN_POINT('Ctrl Pts',(82.5576829436322,-21.9988904823282,20.6955351931789));
#22266=CARTESIAN_POINT('Ctrl Pts',(82.5601126519442,-21.9987969780133,20.6967774260145));
#22267=CARTESIAN_POINT('Ctrl Pts',(82.5625990820839,-21.9986952571646,20.6980490614586));
#22268=CARTESIAN_POINT('Ctrl Pts',(82.5650703996693,-21.9985879497336,20.6993133319474));
#22269=CARTESIAN_POINT('Ctrl Pts',(82.5684481340624,-21.99844128465,20.7010413048868));
#22270=CARTESIAN_POINT('Ctrl Pts',(82.5717937906446,-21.9982840158667,20.7027535614366));
#22271=CARTESIAN_POINT('Ctrl Pts',(82.5748462193364,-21.998131517408,20.7043162728701));
#22272=CARTESIAN_POINT('Ctrl Pts',(82.5771355408552,-21.9980171435639,20.7054883064452));
#22273=CARTESIAN_POINT('Ctrl Pts',(82.5792567661969,-21.9979058195173,20.7065745992276));
#22274=CARTESIAN_POINT('Ctrl Pts',(82.5811192797532,-21.9978049480664,20.7075286386024));
#22275=CARTESIAN_POINT('Ctrl Pts',(82.582693322036,-21.9977196998661,20.7083349137086));
#22276=CARTESIAN_POINT('Ctrl Pts',(82.5840820935019,-21.9976420140725,20.7090464755551));
#22277=CARTESIAN_POINT('Ctrl Pts',(82.5852637181514,-21.9975747388251,20.7096520455423));
#22278=CARTESIAN_POINT('Ctrl Pts',(82.5863746838264,-21.9975114865134,20.7102214035612));
#22279=CARTESIAN_POINT('Ctrl Pts',(82.5873020179414,-21.9974574931031,20.7106968005571));
#22280=CARTESIAN_POINT('Ctrl Pts',(82.5880661954622,-21.9974125501066,20.7110886716049));
#22281=CARTESIAN_POINT('Ctrl Pts',(82.5887787608894,-21.9973706425333,20.711454075916));
#22282=CARTESIAN_POINT('Ctrl Pts',(82.5893492752058,-21.9973366162764,20.7117467587141));
#22283=CARTESIAN_POINT('Ctrl Pts',(82.5898336070652,-21.9973075579325,20.7119953098446));
#22284=CARTESIAN_POINT('Ctrl Pts',(82.5902384964647,-21.997283265879,20.7122030924137));
#22285=CARTESIAN_POINT('Ctrl Pts',(82.5905836515537,-21.9972624085941,20.7123802870035));
#22286=CARTESIAN_POINT('Ctrl Pts',(82.590926702435,-21.9972415752925,20.7125564066551));
#22287=CARTESIAN_POINT('',(82.1333568375101,-21.9972415752925,21.6017012830987));
#22288=CARTESIAN_POINT('Ctrl Pts',(82.1333568375101,-21.9972415752925,21.6017012830987));
#22289=CARTESIAN_POINT('Ctrl Pts',(82.2858801258184,-21.9972415752925,21.3053196576175));
#22290=CARTESIAN_POINT('Ctrl Pts',(82.4384034141267,-21.9972415752925,21.0089380321363));
#22291=CARTESIAN_POINT('Ctrl Pts',(82.590926702435,-21.9972415752925,20.7125564066551));
#22292=CARTESIAN_POINT('',(82.0426945818027,-22.,21.5547198843461));
#22293=CARTESIAN_POINT('Ctrl Pts',(82.1333568375101,-21.9972415752925,21.6017012830988));
#22294=CARTESIAN_POINT('Ctrl Pts',(82.1329515455134,-21.9972662130379,21.6014922153299));
#22295=CARTESIAN_POINT('Ctrl Pts',(82.132542196012,-21.9972909606082,21.6012810461369));
#22296=CARTESIAN_POINT('Ctrl Pts',(82.1320373185083,-21.9973212113064,21.6010204716646));
#22297=CARTESIAN_POINT('Ctrl Pts',(82.1315072911072,-21.9973529689088,21.600746916972));
#22298=CARTESIAN_POINT('Ctrl Pts',(82.1308722414686,-21.9973907806112,21.6004190467318));
#22299=CARTESIAN_POINT('Ctrl Pts',(82.1300778406803,-21.9974373473525,21.6000087380818));
#22300=CARTESIAN_POINT('Ctrl Pts',(82.1292310768093,-21.9974869835496,21.5995713838573));
#22301=CARTESIAN_POINT('Ctrl Pts',(82.1282036189947,-21.9975465399409,21.5990405492434));
#22302=CARTESIAN_POINT('Ctrl Pts',(82.1269821372123,-21.9976156171537,21.5984092814532));
#22303=CARTESIAN_POINT('Ctrl Pts',(82.1256314653394,-21.9976920003218,21.5977112475893));
#22304=CARTESIAN_POINT('Ctrl Pts',(82.1240440752437,-21.9977799506085,21.5968906785504));
#22305=CARTESIAN_POINT('Ctrl Pts',(82.1222576842232,-21.9978753225515,21.595966985438));
#22306=CARTESIAN_POINT('Ctrl Pts',(82.1199983913686,-21.9979959418039,21.5947987679398));
#22307=CARTESIAN_POINT('Ctrl Pts',(82.1174219500873,-21.998128176573,21.5934661935896));
#22308=CARTESIAN_POINT('Ctrl Pts',(82.1146799296805,-21.9982606384566,21.5920475040685));
#22309=CARTESIAN_POINT('Ctrl Pts',(82.1118475151583,-21.9983974671111,21.5905820456815));
#22310=CARTESIAN_POINT('Ctrl Pts',(82.1088442875541,-21.998534141336,21.5890277313331));
#22311=CARTESIAN_POINT('Ctrl Pts',(82.1058475042565,-21.9986611634475,21.5874761936605));
#22312=CARTESIAN_POINT('Ctrl Pts',(82.1035482402478,-21.9987586204005,21.5862857856882));
#22313=CARTESIAN_POINT('Ctrl Pts',(82.1012537725383,-21.9988504816478,21.5850975349178));
#22314=CARTESIAN_POINT('Ctrl Pts',(82.0990140514947,-21.9989351541171,21.5839372918622));
#22315=CARTESIAN_POINT('Ctrl Pts',(82.0969908768119,-21.999011640069,21.5828892263531));
#22316=CARTESIAN_POINT('Ctrl Pts',(82.0950128805348,-21.9990823041441,21.5818642778784));
#22317=CARTESIAN_POINT('Ctrl Pts',(82.0930800673691,-21.9991476850095,21.5808624629178));
#22318=CARTESIAN_POINT('Ctrl Pts',(82.0912338430709,-21.9992101368514,21.579905528665));
#22319=CARTESIAN_POINT('Ctrl Pts',(82.0894293434669,-21.999267802336,21.5789699607435));
#22320=CARTESIAN_POINT('Ctrl Pts',(82.0876238971944,-21.9993222687543,21.578033687473));
#22321=CARTESIAN_POINT('Ctrl Pts',(82.0858002202754,-21.9993772851519,21.5770879601041));
#22322=CARTESIAN_POINT('Ctrl Pts',(82.0839675997984,-21.999429270298,21.5761373812524));
#22323=CARTESIAN_POINT('Ctrl Pts',(82.0820895966761,-21.9994789506814,21.5751631199948));
#22324=CARTESIAN_POINT('Ctrl Pts',(82.0800690672747,-21.9995324014313,21.5741149196525));
#22325=CARTESIAN_POINT('Ctrl Pts',(82.0779964515735,-21.9995831102254,21.5730395364255));
#22326=CARTESIAN_POINT('Ctrl Pts',(82.0758798035365,-21.9996302780206,21.5719412139833));
#22327=CARTESIAN_POINT('Ctrl Pts',(82.0734556422703,-21.9996842985002,21.5706833238307));
#22328=CARTESIAN_POINT('Ctrl Pts',(82.0709744016171,-21.999733553745,21.5693956953634));
#22329=CARTESIAN_POINT('Ctrl Pts',(82.0685078519499,-21.9997763068706,21.5681156411538));
#22330=CARTESIAN_POINT('Ctrl Pts',(82.0651377481162,-21.9998347214545,21.5663666734941));
#22331=CARTESIAN_POINT('Ctrl Pts',(82.0617988953356,-21.999880596871,21.564633832814));
#22332=CARTESIAN_POINT('Ctrl Pts',(82.0587521179753,-21.9999134453804,21.5630525919056));
#22333=CARTESIAN_POINT('Ctrl Pts',(82.056467034955,-21.9999380817625,21.5618666612243));
#22334=CARTESIAN_POINT('Ctrl Pts',(82.0543494020555,-21.9999555654168,21.5607676431849));
#22335=CARTESIAN_POINT('Ctrl Pts',(82.0524898204502,-21.9999677944424,21.5598025786458));
#22336=CARTESIAN_POINT('Ctrl Pts',(82.0509182388138,-21.9999781295156,21.5589869770592));
#22337=CARTESIAN_POINT('Ctrl Pts',(82.0495314630858,-21.999984778476,21.5582673069337));
#22338=CARTESIAN_POINT('Ctrl Pts',(82.0483514248692,-21.9999892597033,21.5576549502537));
#22339=CARTESIAN_POINT('Ctrl Pts',(82.0472419209927,-21.9999934730746,21.5570791959257));
#22340=CARTESIAN_POINT('Ctrl Pts',(82.0463156975305,-21.9999957948245,21.5565985785096));
#22341=CARTESIAN_POINT('Ctrl Pts',(82.045552362205,-21.9999972591221,21.5562025087274));
#22342=CARTESIAN_POINT('Ctrl Pts',(82.0448405655344,-21.9999986245536,21.5558331806708));
#22343=CARTESIAN_POINT('Ctrl Pts',(82.0442705930571,-21.9999992450545,21.5555374666851));
#22344=CARTESIAN_POINT('Ctrl Pts',(82.0437866674028,-21.999999599766,21.5552864132347));
#22345=CARTESIAN_POINT('Ctrl Pts',(82.0433821974482,-21.9999998962375,21.5550765802226));
#22346=CARTESIAN_POINT('Ctrl Pts',(82.0430373427831,-22.,21.5548976890519));
#22347=CARTESIAN_POINT('Ctrl Pts',(82.0426945818027,-22.,21.5547198843461));
#22348=CARTESIAN_POINT('',(82.2713472909014,-22.,21.1104043811532));
#22349=CARTESIAN_POINT('Ctrl Pts',(82.1333568375101,-21.9972415752925,21.6017012830987));
#22350=CARTESIAN_POINT('Ctrl Pts',(82.4926054015329,-21.9754028152909,21.7870177866389));
#22351=CARTESIAN_POINT('Ctrl Pts',(83.2880029902013,-21.6082743755756,22.1691719458688));
#22352=CARTESIAN_POINT('Ctrl Pts',(83.5931332643966,-20.8935561866066,22.2906190968596));
#22353=CARTESIAN_POINT('Ctrl Pts',(83.5931332643966,-20.5,22.2906190968596));
#22354=CARTESIAN_POINT('Ctrl Pts',(82.2858801258184,-21.9972415752925,21.3053196576175));
#22355=CARTESIAN_POINT('Ctrl Pts',(82.6452482445491,-21.9754028152909,21.4904038437257));
#22356=CARTESIAN_POINT('Ctrl Pts',(83.4332756664122,-21.6082743755756,21.8868796324069));
#22357=CARTESIAN_POINT('Ctrl Pts',(83.7287555095978,-20.8935561866066,22.0270793979064));
#22358=CARTESIAN_POINT('Ctrl Pts',(83.7287555095978,-20.5,22.0270793979064));
#22359=CARTESIAN_POINT('Ctrl Pts',(82.4384034141267,-21.9972415752925,21.0089380321363));
#22360=CARTESIAN_POINT('Ctrl Pts',(82.7978910875653,-21.9754028152909,21.1937899008126));
#22361=CARTESIAN_POINT('Ctrl Pts',(83.578548342623,-21.6082743755756,21.6045873189449));
#22362=CARTESIAN_POINT('Ctrl Pts',(83.8643777547989,-20.8935561866066,21.7635396989532));
#22363=CARTESIAN_POINT('Ctrl Pts',(83.8643777547989,-20.5,21.7635396989532));
#22364=CARTESIAN_POINT('Ctrl Pts',(82.590926702435,-21.9972415752925,20.7125564066551));
#22365=CARTESIAN_POINT('Ctrl Pts',(82.9505339305815,-21.9754028152909,20.8971759578994));
#22366=CARTESIAN_POINT('Ctrl Pts',(83.7238210188338,-21.6082743755756,21.322295005483));
#22367=CARTESIAN_POINT('Ctrl Pts',(84.,-20.8935561866066,21.5));
#22368=CARTESIAN_POINT('Ctrl Pts',(84.,-20.5,21.5));
#22369=CARTESIAN_POINT('',(84.,-20.5,21.5));
#22370=CARTESIAN_POINT('Ctrl Pts',(82.590926702435,-21.9972415752925,20.7125564066551));
#22371=CARTESIAN_POINT('Ctrl Pts',(82.9505339305815,-21.9754028152909,20.8971759578994));
#22372=CARTESIAN_POINT('Ctrl Pts',(83.7238210188338,-21.6082743755756,21.322295005483));
#22373=CARTESIAN_POINT('Ctrl Pts',(84.,-20.8935561866066,21.5));
#22374=CARTESIAN_POINT('Ctrl Pts',(84.,-20.5,21.5));
#22375=CARTESIAN_POINT('',(83.5931332643966,-20.5,22.2906190968596));
#22376=CARTESIAN_POINT('',(84.,-20.5,21.5));
#22377=CARTESIAN_POINT('Ctrl Pts',(83.5931332643966,-20.5,22.2906190968596));
#22378=CARTESIAN_POINT('Ctrl Pts',(83.5931332643966,-20.8935561866066,22.2906190968596));
#22379=CARTESIAN_POINT('Ctrl Pts',(83.2880029902013,-21.6082743755756,22.1691719458688));
#22380=CARTESIAN_POINT('Ctrl Pts',(82.4926054015329,-21.9754028152909,21.7870177866389));
#22381=CARTESIAN_POINT('Ctrl Pts',(82.1333568375101,-21.9972415752925,21.6017012830987));
#22382=CARTESIAN_POINT('Origin',(83.7965666321983,-22.,21.8953095484298));
#22383=CARTESIAN_POINT('',(84.,-16.3324829710611,21.5));
#22384=CARTESIAN_POINT('',(83.5931332643966,-15.2357572925904,22.2906190968596));
#22385=CARTESIAN_POINT('Origin',(95.0642847487739,0.,0.));
#22386=CARTESIAN_POINT('',(83.5931332643966,-22.,22.2906190968596));
#22387=CARTESIAN_POINT('',(84.,-22.,21.5));
#22388=CARTESIAN_POINT('Origin',(42.,-22.,8.5));
#22389=CARTESIAN_POINT('',(55.5193024198872,-22.,40.5));
#22390=CARTESIAN_POINT('',(58.4153048715835,-22.,38.4314268202169));
#22391=CARTESIAN_POINT('',(6.62132034355964,-22.,40.5));
#22392=CARTESIAN_POINT('',(24.,-22.,40.5));
#22393=CARTESIAN_POINT('',(1.5,-22.,35.3786796564404));
#22394=CARTESIAN_POINT('',(4.68566017177982,-22.,38.5643398282202));
#22395=CARTESIAN_POINT('',(1.5,-22.,-20.3786796564404));
#22396=CARTESIAN_POINT('',(1.5,-22.,-6.25));
#22397=CARTESIAN_POINT('',(4.62132034355965,-22.,-23.5));
#22398=CARTESIAN_POINT('',(6.18566017177982,-22.,-25.0643398282202));
#22399=CARTESIAN_POINT('',(13.5,-22.,-23.5));
#22400=CARTESIAN_POINT('',(56.,-22.,-23.5));
#22401=CARTESIAN_POINT('',(13.5,-22.,18.));
#22402=CARTESIAN_POINT('',(13.5,-22.,-10.75));
#22403=CARTESIAN_POINT('',(18.,-22.,22.5));
#22404=CARTESIAN_POINT('Origin',(18.,-22.,18.));
#22405=CARTESIAN_POINT('',(57.,-22.,22.5));
#22406=CARTESIAN_POINT('',(28.5,-22.,22.5));
#22407=CARTESIAN_POINT('',(61.5,-22.,18.));
#22408=CARTESIAN_POINT('Origin',(57.,-22.,18.));
#22409=CARTESIAN_POINT('',(61.5,-22.,15.6524758424985));
#22410=CARTESIAN_POINT('',(61.5,-22.,14.75));
#22411=CARTESIAN_POINT('',(82.5,-22.,15.6524758424985));
#22412=CARTESIAN_POINT('',(75.5,-22.,15.6524758424985));
#22413=CARTESIAN_POINT('',(82.5,-22.,15.25));
#22414=CARTESIAN_POINT('Origin',(58.4153048715835,-20.5,38.4314268202169));
#22415=CARTESIAN_POINT('',(56.3911597104659,-20.5,41.7206002068101));
#22416=CARTESIAN_POINT('',(59.2871621621622,-20.5,39.652027027027));
#22417=CARTESIAN_POINT('Origin',(55.5193024198872,-20.5,40.5));
#22418=CARTESIAN_POINT('Origin',(56.,-22.,42.));
#22419=CARTESIAN_POINT('',(83.3718572905786,15.0019020194829,22.4486733638724));
#22420=CARTESIAN_POINT('Origin',(114.8,0.,0.));
#22421=CARTESIAN_POINT('',(83.3718572905786,20.5,22.4486733638724));
#22422=CARTESIAN_POINT('',(83.3718572905786,-22.,22.4486733638724));
#22423=CARTESIAN_POINT('',(56.3911597104659,20.5,41.7206002068101));
#22424=CARTESIAN_POINT('',(59.2871621621622,20.5,39.652027027027));
#22425=CARTESIAN_POINT('',(56.3911597104659,-22.,41.7206002068101));
#22426=CARTESIAN_POINT('Ctrl Pts',(4.54678558986685,19.8682455202995,-24.9981470456841));
#22427=CARTESIAN_POINT('Ctrl Pts',(4.55093583868358,19.8641612816606,-24.9983535259319));
#22428=CARTESIAN_POINT('Ctrl Pts',(4.58143737374893,19.8342243880485,-24.9997804759391));
#22429=CARTESIAN_POINT('Ctrl Pts',(4.61489089919229,19.8015972979556,-24.9999871969247));
#22430=CARTESIAN_POINT('Ctrl Pts',(4.62027734084719,19.7963354971355,-25.));
#22431=CARTESIAN_POINT('Ctrl Pts',(4.62132034355965,19.7953186364093,-25.));
#22432=CARTESIAN_POINT('Ctrl Pts',(4.7822153343313,20.1036752647639,-24.9981470456841));
#22433=CARTESIAN_POINT('Ctrl Pts',(4.78634357975541,20.0995690227324,-24.9983535259319));
#22434=CARTESIAN_POINT('Ctrl Pts',(4.81661719703365,20.0694042113332,-24.9997804759391));
#22435=CARTESIAN_POINT('Ctrl Pts',(4.8498425300617,20.036548928825,-24.9999871969247));
#22436=CARTESIAN_POINT('Ctrl Pts',(4.85517984270618,20.0312379989945,-25.));
#22437=CARTESIAN_POINT('Ctrl Pts',(4.85621413142322,20.0302124242728,-25.));
#22438=CARTESIAN_POINT('Ctrl Pts',(5.01764507879574,20.3391050092283,-24.9981470456841));
#22439=CARTESIAN_POINT('Ctrl Pts',(5.02175132082723,20.3349767638042,-24.9983535259319));
#22440=CARTESIAN_POINT('Ctrl Pts',(5.05191613222637,20.304526175821,-25.0000202744737));
#22441=CARTESIAN_POINT('Ctrl Pts',(5.08477141473465,20.271453204594,-24.9998345971494));
#22442=CARTESIAN_POINT('Ctrl Pts',(5.09008234456518,20.2661405008535,-25.));
#22443=CARTESIAN_POINT('Ctrl Pts',(5.0911079192868,20.2651062121364,-25.));
#22444=CARTESIAN_POINT('Ctrl Pts',(5.25307482326019,20.5745347536928,-24.9981470456841));
#22445=CARTESIAN_POINT('Ctrl Pts',(5.25715906189905,20.5703845048761,-24.9983535259319));
#22446=CARTESIAN_POINT('Ctrl Pts',(5.28709595551109,20.5398829698107,-24.9997804759391));
#22447=CARTESIAN_POINT('Ctrl Pts',(5.31972304560406,20.5064294443674,-24.9999871969247));
#22448=CARTESIAN_POINT('Ctrl Pts',(5.32498484642417,20.5010430027125,-25.));
#22449=CARTESIAN_POINT('Ctrl Pts',(5.32600170715038,20.5,-25.));
#22450=CARTESIAN_POINT('',(4.62132034355965,19.7953186364093,-25.));
#22451=CARTESIAN_POINT('',(4.54678558986685,19.8682455202995,-24.9981470456841));
#22452=CARTESIAN_POINT('Ctrl Pts',(4.62132034355965,19.7953186364093,-25.));
#22453=CARTESIAN_POINT('Ctrl Pts',(4.62098833704959,19.7956423214552,-25.));
#22454=CARTESIAN_POINT('Ctrl Pts',(4.62065306038901,19.7959691994142,-24.9999999083843));
#22455=CARTESIAN_POINT('Ctrl Pts',(4.62024024126657,19.7963717921936,-24.9999996111263));
#22456=CARTESIAN_POINT('Ctrl Pts',(4.61980697903812,19.7967943216629,-24.9999992991479));
#22457=CARTESIAN_POINT('Ctrl Pts',(4.61928851221717,19.7973000472878,-24.9999987638439));
#22458=CARTESIAN_POINT('Ctrl Pts',(4.61864053809611,19.7979322315752,-24.9999976062123));
#22459=CARTESIAN_POINT('Ctrl Pts',(4.61795018430504,19.7986057628248,-24.9999963728678));
#22460=CARTESIAN_POINT('Ctrl Pts',(4.61711311377486,19.7994225566992,-24.9999944297595));
#22461=CARTESIAN_POINT('Ctrl Pts',(4.61611808610815,19.8003936022613,-24.999990978812));
#22462=CARTESIAN_POINT('Ctrl Pts',(4.61501963958223,19.8014655740868,-24.999987169188));
#22463=CARTESIAN_POINT('Ctrl Pts',(4.61372910964003,19.8027251227113,-24.9999814945831));
#22464=CARTESIAN_POINT('Ctrl Pts',(4.61227623408374,19.8041432486014,-24.9999727344468));
#22465=CARTESIAN_POINT('Ctrl Pts',(4.61045329055158,19.8059225912354,-24.9999617429798));
#22466=CARTESIAN_POINT('Ctrl Pts',(4.60837566715098,19.8079507006083,-24.9999457782408));
#22467=CARTESIAN_POINT('Ctrl Pts',(4.60616166416588,19.8101121911254,-24.9999234028573));
#22468=CARTESIAN_POINT('Ctrl Pts',(4.60381355266282,19.8124046093294,-24.9998996721325));
#22469=CARTESIAN_POINT('Ctrl Pts',(4.60131688796196,19.8148423226041,-24.9998686879986));
#22470=CARTESIAN_POINT('Ctrl Pts',(4.59882328102637,19.817277508365,-24.9998312845708));
#22471=CARTESIAN_POINT('Ctrl Pts',(4.59693379067582,19.8191227310148,-24.999802942728));
#22472=CARTESIAN_POINT('Ctrl Pts',(4.59504687759637,19.8209657010644,-24.9997710160886));
#22473=CARTESIAN_POINT('Ctrl Pts',(4.59320445521053,19.8227656108414,-24.9997364757924));
#22474=CARTESIAN_POINT('Ctrl Pts',(4.59154190291722,19.8243898009026,-24.9997053075603));
#22475=CARTESIAN_POINT('Ctrl Pts',(4.5899159891667,19.8259785263526,-24.9996720606843));
#22476=CARTESIAN_POINT('Ctrl Pts',(4.58832795537129,19.8275306848797,-24.9996371235474));
#22477=CARTESIAN_POINT('Ctrl Pts',(4.58676097332109,19.8290622672415,-24.9996026495542));
#22478=CARTESIAN_POINT('Ctrl Pts',(4.58523154624858,19.8305575877079,-24.9995665836662));
#22479=CARTESIAN_POINT('Ctrl Pts',(4.58370227592527,19.8320533055383,-24.9995282194702));
#22480=CARTESIAN_POINT('Ctrl Pts',(4.58221111704353,19.8335117480997,-24.9994908113608));
#22481=CARTESIAN_POINT('Ctrl Pts',(4.58071342303859,19.8349771101062,-24.999451043943));
#22482=CARTESIAN_POINT('Ctrl Pts',(4.57917937054696,19.8364785839886,-24.9994079292819));
#22483=CARTESIAN_POINT('Ctrl Pts',(4.57753054138005,19.8380923970388,-24.9993615888138));
#22484=CARTESIAN_POINT('Ctrl Pts',(4.5758400682372,19.8397475771906,-24.999311351025));
#22485=CARTESIAN_POINT('Ctrl Pts',(4.57411385800763,19.8414382892535,-24.9992569985569));
#22486=CARTESIAN_POINT('Ctrl Pts',(4.57214165480933,19.8433699356316,-24.9991949006098));
#22487=CARTESIAN_POINT('Ctrl Pts',(4.57012334014877,19.8453474383937,-24.9991273806813));
#22488=CARTESIAN_POINT('Ctrl Pts',(4.56811545869005,19.8473152862887,-24.9990561164366));
#22489=CARTESIAN_POINT('Ctrl Pts',(4.56533443804158,19.8500408583613,-24.9989574117372));
#22490=CARTESIAN_POINT('Ctrl Pts',(4.562576391132,19.852745017667,-24.9988513941288));
#22491=CARTESIAN_POINT('Ctrl Pts',(4.5600578537522,19.855215144939,-24.9987484469859));
#22492=CARTESIAN_POINT('Ctrl Pts',(4.55816895071736,19.8570677403929,-24.9986712366287));
#22493=CARTESIAN_POINT('Ctrl Pts',(4.55641746154057,19.8587860498669,-24.9985960052401));
#22494=CARTESIAN_POINT('Ctrl Pts',(4.55487916244497,19.8602955926206,-24.9985278006938));
#22495=CARTESIAN_POINT('Ctrl Pts',(4.55359016866188,19.8615604904745,-24.9984706497558));
#22496=CARTESIAN_POINT('Ctrl Pts',(4.55245123366914,19.8626784402,-24.9984184962121));
#22497=CARTESIAN_POINT('Ctrl Pts',(4.55148064564489,19.8636314053933,-24.9983732567672));
#22498=CARTESIAN_POINT('Ctrl Pts',(4.55056811294028,19.8645273693692,-24.9983307233009));
#22499=CARTESIAN_POINT('Ctrl Pts',(4.54980480757313,19.865277085181,-24.9982943388109));
#22500=CARTESIAN_POINT('Ctrl Pts',(4.54917498181042,19.8658959318917,-24.9982640110401));
#22501=CARTESIAN_POINT('Ctrl Pts',(4.54858795079092,19.8664727298523,-24.9982357439491));
#22502=CARTESIAN_POINT('Ctrl Pts',(4.54811702674687,19.8669356913585,-24.9982127465679));
#22503=CARTESIAN_POINT('Ctrl Pts',(4.54771804473987,19.8673281021022,-24.9981931456286));
#22504=CARTESIAN_POINT('Ctrl Pts',(4.54737031074586,19.8676701088915,-24.9981760623697));
#22505=CARTESIAN_POINT('Ctrl Pts',(4.54707695328725,19.8679587910473,-24.9981615413912));
#22506=CARTESIAN_POINT('Ctrl Pts',(4.54678558986685,19.8682455202995,-24.9981470456841));
#22507=CARTESIAN_POINT('',(5.25307482326019,20.5745347536928,-24.9981470456841));
#22508=CARTESIAN_POINT('Ctrl Pts',(5.25307482326019,20.5745347536928,-24.9981470456841));
#22509=CARTESIAN_POINT('Ctrl Pts',(5.01764507879574,20.3391050092283,-24.9981470456841));
#22510=CARTESIAN_POINT('Ctrl Pts',(4.7822153343313,20.1036752647639,-24.9981470456841));
#22511=CARTESIAN_POINT('Ctrl Pts',(4.54678558986685,19.8682455202995,-24.9981470456841));
#22512=CARTESIAN_POINT('',(5.32600170715038,20.5,-25.));
#22513=CARTESIAN_POINT('Ctrl Pts',(5.25307482326019,20.5745347536928,-24.9981470456841));
#22514=CARTESIAN_POINT('Ctrl Pts',(5.25339985886691,20.5742044648039,-24.9981634779836));
#22515=CARTESIAN_POINT('Ctrl Pts',(5.2537280933634,20.5738709111413,-24.9981799817513));
#22516=CARTESIAN_POINT('Ctrl Pts',(5.25413216335514,20.5734600252166,-24.9982001283858));
#22517=CARTESIAN_POINT('Ctrl Pts',(5.25455624459622,20.5730287904889,-24.9982212727665));
#22518=CARTESIAN_POINT('Ctrl Pts',(5.25506365516221,20.572512581772,-24.9982464226455));
#22519=CARTESIAN_POINT('Ctrl Pts',(5.2556977141089,20.5718671927797,-24.9982773797271));
#22520=CARTESIAN_POINT('Ctrl Pts',(5.25637324645706,20.5711795892946,-24.9983103616922));
#22521=CARTESIAN_POINT('Ctrl Pts',(5.25719225799349,20.5703456377491,-24.9983499179323));
#22522=CARTESIAN_POINT('Ctrl Pts',(5.25816572676123,20.5693540673989,-24.9983958133068));
#22523=CARTESIAN_POINT('Ctrl Pts',(5.25924039301158,20.5682594178061,-24.9984464797602));
#22524=CARTESIAN_POINT('Ctrl Pts',(5.26050289280568,20.5669730879005,-24.9985048239997));
#22525=CARTESIAN_POINT('Ctrl Pts',(5.26192412261039,20.5655246259075,-24.9985681577425));
#22526=CARTESIAN_POINT('Ctrl Pts',(5.26370752556061,20.5637070511684,-24.9986476308744));
#22527=CARTESIAN_POINT('Ctrl Pts',(5.26573998138134,20.5616350783528,-24.9987348006106));
#22528=CARTESIAN_POINT('Ctrl Pts',(5.26790573837352,20.5594265093687,-24.9988223677222));
#22529=CARTESIAN_POINT('Ctrl Pts',(5.27020197977311,20.5570848766032,-24.998915210653));
#22530=CARTESIAN_POINT('Ctrl Pts',(5.27264332828516,20.5545945239351,-24.9990082175786));
#22531=CARTESIAN_POINT('Ctrl Pts',(5.2750816169699,20.5521063655077,-24.9990947023699));
#22532=CARTESIAN_POINT('Ctrl Pts',(5.27692945702648,20.5502207320148,-24.9991602442652));
#22533=CARTESIAN_POINT('Ctrl Pts',(5.27877473625192,20.548337181907,-24.9992220998817));
#22534=CARTESIAN_POINT('Ctrl Pts',(5.28057649496845,20.5464974338248,-24.999279156344));
#22535=CARTESIAN_POINT('Ctrl Pts',(5.28220237330072,20.5448372744947,-24.9993306431857));
#22536=CARTESIAN_POINT('Ctrl Pts',(5.28379241057199,20.5432131948601,-24.9993782510764));
#22537=CARTESIAN_POINT('Ctrl Pts',(5.28534543187148,20.5416263520351,-24.9994223043613));
#22538=CARTESIAN_POINT('Ctrl Pts',(5.28687822685119,20.5400601760164,-24.9994657839028));
#22539=CARTESIAN_POINT('Ctrl Pts',(5.28837430276488,20.5385309483966,-24.9995058211122));
#22540=CARTESIAN_POINT('Ctrl Pts',(5.28987033506272,20.5370012069583,-24.999543567451));
#22541=CARTESIAN_POINT('Ctrl Pts',(5.29132872010489,20.5355099610573,-24.9995803639132));
#22542=CARTESIAN_POINT('Ctrl Pts',(5.29279360477615,20.5340115437723,-24.9996151417452));
#22543=CARTESIAN_POINT('Ctrl Pts',(5.29429419368321,20.5324761755474,-24.9996483914644));
#22544=CARTESIAN_POINT('Ctrl Pts',(5.29590707598065,20.5308259112954,-24.9996841293559));
#22545=CARTESIAN_POINT('Ctrl Pts',(5.29756085615442,20.5291333163862,-24.9997180535011));
#22546=CARTESIAN_POINT('Ctrl Pts',(5.29924977607504,20.5274044083941,-24.999749645241));
#22547=CARTESIAN_POINT('Ctrl Pts',(5.30117946913945,20.5254290265417,-24.9997857407128));
#22548=CARTESIAN_POINT('Ctrl Pts',(5.30315451227523,20.5234067749386,-24.9998187134049));
#22549=CARTESIAN_POINT('Ctrl Pts',(5.30511956577291,20.5213944706428,-24.9998474177815));
#22550=CARTESIAN_POINT('Ctrl Pts',(5.30784086271432,20.5186077386114,-24.9998871689295));
#22551=CARTESIAN_POINT('Ctrl Pts',(5.31054011508801,20.5158430430512,-24.9999184562551));
#22552=CARTESIAN_POINT('Ctrl Pts',(5.3130053286776,20.5133177855987,-24.9999408776971));
#22553=CARTESIAN_POINT('Ctrl Pts',(5.31485423886979,20.5114238425093,-24.9999576937786));
#22554=CARTESIAN_POINT('Ctrl Pts',(5.31656886411985,20.5096672835416,-24.9999696412555));
#22555=CARTESIAN_POINT('Ctrl Pts',(5.31807494917383,20.5081242380259,-24.9999779987575));
#22556=CARTESIAN_POINT('Ctrl Pts',(5.31933697354538,20.5068312426256,-24.9999850019285));
#22557=CARTESIAN_POINT('Ctrl Pts',(5.32045220380261,20.5056885414075,-24.9999895296818));
#22558=CARTESIAN_POINT('Ctrl Pts',(5.32140268042815,20.5047145553013,-24.9999925909711));
#22559=CARTESIAN_POINT('Ctrl Pts',(5.32229631396741,20.5037988182617,-24.9999954691806));
#22560=CARTESIAN_POINT('Ctrl Pts',(5.32304390109983,20.5030326389375,-24.9999970676595));
#22561=CARTESIAN_POINT('Ctrl Pts',(5.32366082469884,20.5024002743131,-24.9999980795598));
#22562=CARTESIAN_POINT('Ctrl Pts',(5.32423583584433,20.501810871172,-24.9999990227139));
#22563=CARTESIAN_POINT('Ctrl Pts',(5.32469718707828,20.5013378687583,-24.9999994569353));
#22564=CARTESIAN_POINT('Ctrl Pts',(5.32508810907333,20.5009369959301,-24.9999997073462));
#22565=CARTESIAN_POINT('Ctrl Pts',(5.32542876905438,20.5005876645244,-24.999999925561));
#22566=CARTESIAN_POINT('Ctrl Pts',(5.3257162121543,20.5002928346505,-25.));
#22567=CARTESIAN_POINT('Ctrl Pts',(5.32600170715039,20.5,-25.));
#22568=CARTESIAN_POINT('',(4.97366102535501,20.1476593182046,-25.));
#22569=CARTESIAN_POINT('Ctrl Pts',(0.00185295431591348,20.5745347536928,
-19.7469251767398));
#22570=CARTESIAN_POINT('Ctrl Pts',(0.00164647406805663,20.5703845048761,
-19.742840938101));
#22571=CARTESIAN_POINT('Ctrl Pts',(0.000218999411820001,20.5398627220639,
-19.7128841548999));
#22572=CARTESIAN_POINT('Ctrl Pts',(1.27370737248938E-5,20.5064246274686,
-19.6802722284864));
#22573=CARTESIAN_POINT('Ctrl Pts',(-9.64971355100933E-20,20.5010430027125,
-19.6750151535758));
#22574=CARTESIAN_POINT('Ctrl Pts',(0.,20.5,-19.6739982928496));
#22575=CARTESIAN_POINT('Ctrl Pts',(0.00185295431591376,20.3391050092284,
-19.9823549212043));
#22576=CARTESIAN_POINT('Ctrl Pts',(0.00164647406805682,20.3349767638042,
-19.9782486791728));
#22577=CARTESIAN_POINT('Ctrl Pts',(0.000218999411820078,20.3046828987792,
-19.9480639781846));
#22578=CARTESIAN_POINT('Ctrl Pts',(1.27370737249021E-5,20.2714729965992,
-19.9152238593558));
#22579=CARTESIAN_POINT('Ctrl Pts',(-6.62449705573466E-20,20.2661405008535,
-19.9099176554348));
#22580=CARTESIAN_POINT('Ctrl Pts',(0.,20.2651062121364,-19.9088920807132));
#22581=CARTESIAN_POINT('Ctrl Pts',(0.00185295431591403,20.1036752647639,
-20.2177846656687));
#22582=CARTESIAN_POINT('Ctrl Pts',(0.00164647406805702,20.0995690227324,
-20.2136564202446));
#22583=CARTESIAN_POINT('Ctrl Pts',(-1.76372974816777E-5,20.0693843217443,
-20.1831854192229));
#22584=CARTESIAN_POINT('Ctrl Pts',(0.000166089722694393,20.0365442029154,
-20.150128023312));
#22585=CARTESIAN_POINT('Ctrl Pts',(-2.83060097038847E-20,20.0312379989945,
-20.1448201572938));
#22586=CARTESIAN_POINT('Ctrl Pts',(0.,20.0302124242728,-20.1437858685768));
#22587=CARTESIAN_POINT('Ctrl Pts',(0.00185295431591431,19.8682455202995,
-20.4532144101331));
#22588=CARTESIAN_POINT('Ctrl Pts',(0.00164647406805721,19.8641612816606,
-20.4490641613164));
#22589=CARTESIAN_POINT('Ctrl Pts',(0.00021899941182044,19.8342044984596,
-20.4185423785043));
#22590=CARTESIAN_POINT('Ctrl Pts',(1.27370737248456E-5,19.801592572046,
-20.385104283909));
#22591=CARTESIAN_POINT('Ctrl Pts',(0.,19.7963354971355,-20.3797226591528));
#22592=CARTESIAN_POINT('Ctrl Pts',(0.,19.7953186364093,-20.3786796564404));
#22593=CARTESIAN_POINT('',(0.,20.5,-19.6739982928496));
#22594=CARTESIAN_POINT('',(0.00185295431591348,20.5745347536928,-19.7469251767398));
#22595=CARTESIAN_POINT('Ctrl Pts',(-1.33226762955019E-15,20.5,-19.6739982928496));
#22596=CARTESIAN_POINT('Ctrl Pts',(-1.33226762955019E-15,20.5003320065101,
-19.6743219778956));
#22597=CARTESIAN_POINT('Ctrl Pts',(9.16157061043807E-8,20.5006672831706,
-19.6746488558546));
#22598=CARTESIAN_POINT('Ctrl Pts',(3.88873703682791E-7,20.5010801022931,
-19.6750514486339));
#22599=CARTESIAN_POINT('Ctrl Pts',(7.00852135530467E-7,20.5015133645215,
-19.6754739781033));
#22600=CARTESIAN_POINT('Ctrl Pts',(1.2361561089926E-6,20.5020318313425,
-19.6759797037281));
#22601=CARTESIAN_POINT('Ctrl Pts',(2.39378768296383E-6,20.5026798054635,
-19.6766118880155));
#22602=CARTESIAN_POINT('Ctrl Pts',(3.62713222530517E-6,20.5033701592546,
-19.6772854192651));
#22603=CARTESIAN_POINT('Ctrl Pts',(5.57024050657816E-6,20.5042072297849,
-19.6781022131396));
#22604=CARTESIAN_POINT('Ctrl Pts',(9.02118799039897E-6,20.5052022574516,
-19.6790732587018));
#22605=CARTESIAN_POINT('Ctrl Pts',(1.28308119852926E-5,20.5063007039776,
-19.6801452305273));
#22606=CARTESIAN_POINT('Ctrl Pts',(1.85054169170547E-5,20.5075912339199,
-19.6814047791519));
#22607=CARTESIAN_POINT('Ctrl Pts',(2.72655532085331E-5,20.5090441094763,
-19.6828229050421));
#22608=CARTESIAN_POINT('Ctrl Pts',(3.82570202503681E-5,20.5108670530085,
-19.6846022476762));
#22609=CARTESIAN_POINT('Ctrl Pts',(5.42217591519492E-5,20.5129446764091,
-19.6866303570491));
#22610=CARTESIAN_POINT('Ctrl Pts',(7.65971426985868E-5,20.5151586793942,
-19.6887918475662));
#22611=CARTESIAN_POINT('Ctrl Pts',(0.000100327867472851,20.5175067908972,
-19.6910842657702));
#22612=CARTESIAN_POINT('Ctrl Pts',(0.000131312001377887,20.520003455598,
-19.6935219790447));
#22613=CARTESIAN_POINT('Ctrl Pts',(0.000168715429175847,20.5224970625335,
-19.6959571648056));
#22614=CARTESIAN_POINT('Ctrl Pts',(0.00019705727202824,20.524386552884,
-19.6978023874553));
#22615=CARTESIAN_POINT('Ctrl Pts',(0.000228983911360227,20.5262734659634,
-19.6996453575049));
#22616=CARTESIAN_POINT('Ctrl Pts',(0.000263524207557708,20.5281158883493,
-19.701445267282));
#22617=CARTESIAN_POINT('Ctrl Pts',(0.000294692439715454,20.5297784406426,
-19.7030694573431));
#22618=CARTESIAN_POINT('Ctrl Pts',(0.000327939315699018,20.5314043543931,
-19.704658182793));
#22619=CARTESIAN_POINT('Ctrl Pts',(0.00036287645256472,20.5329923881885,
-19.7062103413201));
#22620=CARTESIAN_POINT('Ctrl Pts',(0.000397350445821907,20.5345593702387,
-19.707741923682));
#22621=CARTESIAN_POINT('Ctrl Pts',(0.00043341633385059,20.5360887973112,
-19.7092372441484));
#22622=CARTESIAN_POINT('Ctrl Pts',(0.000471780529807564,20.5376180676346,
-19.7107329619788));
#22623=CARTESIAN_POINT('Ctrl Pts',(0.000509188639198179,20.5391092265163,
-19.7121914045402));
#22624=CARTESIAN_POINT('Ctrl Pts',(0.000548956057017146,20.5406069205213,
-19.7136567665468));
#22625=CARTESIAN_POINT('Ctrl Pts',(0.000592070718070437,20.542140973013,
-19.7151582404293));
#22626=CARTESIAN_POINT('Ctrl Pts',(0.000638411186244535,20.5437898021799,
-19.7167720534795));
#22627=CARTESIAN_POINT('Ctrl Pts',(0.000688648974965052,20.5454802753228,
-19.7184272336313));
#22628=CARTESIAN_POINT('Ctrl Pts',(0.000743001443115787,20.5472064855524,
-19.7201179456942));
#22629=CARTESIAN_POINT('Ctrl Pts',(0.000805099390218029,20.5491786887507,
-19.7220495920723));
#22630=CARTESIAN_POINT('Ctrl Pts',(0.000872619318741684,20.5511970034113,
-19.7240270948345));
#22631=CARTESIAN_POINT('Ctrl Pts',(0.000943883563405024,20.5532048848701,
-19.7259949427295));
#22632=CARTESIAN_POINT('Ctrl Pts',(0.0010425882628478,20.5559859055185,
-19.7287205148021));
#22633=CARTESIAN_POINT('Ctrl Pts',(0.00114860587122066,20.558743952428,
-19.7314246741078));
#22634=CARTESIAN_POINT('Ctrl Pts',(0.00125155301412994,20.5612624898078,
-19.7338948013796));
#22635=CARTESIAN_POINT('Ctrl Pts',(0.00132876337131189,20.5631513928426,
-19.7357473968336));
#22636=CARTESIAN_POINT('Ctrl Pts',(0.00140399475990964,20.5649028820193,
-19.7374657063075));
#22637=CARTESIAN_POINT('Ctrl Pts',(0.00147219930624476,20.5664411811149,
-19.7389752490611));
#22638=CARTESIAN_POINT('Ctrl Pts',(0.00152935024422438,20.567730174898,
-19.7402401469151));
#22639=CARTESIAN_POINT('Ctrl Pts',(0.00158150378788142,20.5688691098907,
-19.7413580966406));
#22640=CARTESIAN_POINT('Ctrl Pts',(0.00162674323279743,20.5698396979149,
-19.7423110618338));
#22641=CARTESIAN_POINT('Ctrl Pts',(0.00166927669910059,20.5707522306195,
-19.7432070258097));
#22642=CARTESIAN_POINT('Ctrl Pts',(0.00170566118909408,20.5715155359867,
-19.7439567416215));
#22643=CARTESIAN_POINT('Ctrl Pts',(0.00173598895987004,20.5721453617494,
-19.7445755883322));
#22644=CARTESIAN_POINT('Ctrl Pts',(0.00176425605094743,20.5727323927688,
-19.7451523862928));
#22645=CARTESIAN_POINT('Ctrl Pts',(0.001787253432131,20.5732033168129,-19.7456153477989));
#22646=CARTESIAN_POINT('Ctrl Pts',(0.0018068543714278,20.5736022988199,
-19.7460077585426));
#22647=CARTESIAN_POINT('Ctrl Pts',(0.0018239376302916,20.5739500328138,
-19.7463497653319));
#22648=CARTESIAN_POINT('Ctrl Pts',(0.00183845860880921,20.5742433902724,
-19.7466384474877));
#22649=CARTESIAN_POINT('Ctrl Pts',(0.00185295431591337,20.5745347536928,
-19.7469251767398));
#22650=CARTESIAN_POINT('',(0.00185295431591431,19.8682455202995,-20.4532144101331));
#22651=CARTESIAN_POINT('Ctrl Pts',(0.00185295431591431,19.8682455202995,
-20.4532144101331));
#22652=CARTESIAN_POINT('Ctrl Pts',(0.00185295431591403,20.1036752647639,
-20.2177846656687));
#22653=CARTESIAN_POINT('Ctrl Pts',(0.00185295431591376,20.3391050092284,
-19.9823549212043));
#22654=CARTESIAN_POINT('Ctrl Pts',(0.00185295431591348,20.5745347536928,
-19.7469251767398));
#22655=CARTESIAN_POINT('',(0.,19.7953186364093,-20.3786796564404));
#22656=CARTESIAN_POINT('Ctrl Pts',(0.00185295431591403,19.8682455202995,
-20.4532144101332));
#22657=CARTESIAN_POINT('Ctrl Pts',(0.0018365220163917,19.8679204846928,
-20.4528841212442));
#22658=CARTESIAN_POINT('Ctrl Pts',(0.0018200182487141,19.8675922501963,
-20.4525505675817));
#22659=CARTESIAN_POINT('Ctrl Pts',(0.00179987161422024,19.8671881802045,
-20.452139681657));
#22660=CARTESIAN_POINT('Ctrl Pts',(0.00177872723345861,19.8667640989635,
-20.4517084469293));
#22661=CARTESIAN_POINT('Ctrl Pts',(0.00175357735450232,19.8662566883975,
-20.4511922382125));
#22662=CARTESIAN_POINT('Ctrl Pts',(0.00172262027288483,19.8656226294509,
-20.4505468492202));
#22663=CARTESIAN_POINT('Ctrl Pts',(0.00168963830780533,19.8649470971028,
-20.4498592457351));
#22664=CARTESIAN_POINT('Ctrl Pts',(0.00165008206768198,19.8641280855664,
-20.4490252941897));
#22665=CARTESIAN_POINT('Ctrl Pts',(0.00160418669325102,19.8631546167987,
-20.4480337238395));
#22666=CARTESIAN_POINT('Ctrl Pts',(0.00155352023986771,19.8620799505485,
-20.4469390742469));
#22667=CARTESIAN_POINT('Ctrl Pts',(0.00149517600032736,19.8608174507546,
-20.4456527443415));
#22668=CARTESIAN_POINT('Ctrl Pts',(0.00143184225756587,19.8593962209502,
-20.4442042823488));
#22669=CARTESIAN_POINT('Ctrl Pts',(0.00135236912569878,19.8576128180005,
-20.4423867076102));
#22670=CARTESIAN_POINT('Ctrl Pts',(0.0012651993894486,19.8555803621803,
-20.4403147347952));
#22671=CARTESIAN_POINT('Ctrl Pts',(0.00117763227794754,19.8534146051887,
-20.4381061658117));
#22672=CARTESIAN_POINT('Ctrl Pts',(0.00108478934705518,19.8511183637887,
-20.4357645330458));
#22673=CARTESIAN_POINT('Ctrl Pts',(0.000991782421426017,19.8486770152762,
-20.4332741803772));
#22674=CARTESIAN_POINT('Ctrl Pts',(0.000905297630115376,19.8462387265909,
-20.4307860219493));
#22675=CARTESIAN_POINT('Ctrl Pts',(0.00083975573483102,19.8443908865342,
-20.4289003884562));
#22676=CARTESIAN_POINT('Ctrl Pts',(0.000777900118314327,19.8425456073086,
-20.4270168383482));
#22677=CARTESIAN_POINT('Ctrl Pts',(0.000720843655976244,19.8407438485919,
-20.4251770902658));
#22678=CARTESIAN_POINT('Ctrl Pts',(0.000669356814273844,19.8391179702596,
-20.4235169309357));
#22679=CARTESIAN_POINT('Ctrl Pts',(0.000621748923652178,19.8375279329883,
-20.4218928513011));
#22680=CARTESIAN_POINT('Ctrl Pts',(0.000577695638684927,19.8359749116888,
-20.4203060084761));
#22681=CARTESIAN_POINT('Ctrl Pts',(0.000534216097193185,19.8344421167093,
-20.4187398324576));
#22682=CARTESIAN_POINT('Ctrl Pts',(0.000494178887846744,19.8329460407958,
-20.417210604838));
#22683=CARTESIAN_POINT('Ctrl Pts',(0.000456432549044816,19.8314500084981,
-20.4156808633999));
#22684=CARTESIAN_POINT('Ctrl Pts',(0.000419636086835154,19.829991623456,
-20.4141896174989));
#22685=CARTESIAN_POINT('Ctrl Pts',(0.000384858254870382,19.8285267387848,
-20.412691200214));
#22686=CARTESIAN_POINT('Ctrl Pts',(0.000351608535610337,19.8270261498778,
-20.411155831989));
#22687=CARTESIAN_POINT('Ctrl Pts',(0.000315870644081551,19.8254132675804,
-20.4095055677372));
#22688=CARTESIAN_POINT('Ctrl Pts',(0.000281946498895475,19.8237594874066,
-20.407812972828));
#22689=CARTESIAN_POINT('Ctrl Pts',(0.000250354759005367,19.822070567486,
-20.4060840648359));
#22690=CARTESIAN_POINT('Ctrl Pts',(0.000214259287211671,19.8201408744217,
-20.4041086829836));
#22691=CARTESIAN_POINT('Ctrl Pts',(0.000181286595136419,19.818165831286,
-20.4020864313805));
#22692=CARTESIAN_POINT('Ctrl Pts',(0.000152582218496233,19.8162007777884,
-20.4000741270848));
#22693=CARTESIAN_POINT('Ctrl Pts',(0.000112831070522241,19.8134794808468,
-20.3972873950533));
#22694=CARTESIAN_POINT('Ctrl Pts',(8.15437448740462E-5,19.810780228473,
-20.3945226994929));
#22695=CARTESIAN_POINT('Ctrl Pts',(5.91223029096088E-5,19.8083150148832,
-20.3919974420402));
#22696=CARTESIAN_POINT('Ctrl Pts',(4.23062214362809E-5,19.8064661046908,
-20.3901034989507));
#22697=CARTESIAN_POINT('Ctrl Pts',(3.03587444767948E-5,19.8047514794406,
-20.3883469399828));
#22698=CARTESIAN_POINT('Ctrl Pts',(2.20012425220517E-5,19.8032453943865,
-20.386803894467));
#22699=CARTESIAN_POINT('Ctrl Pts',(1.49980715364258E-5,19.8019833700149,
-20.3855108990666));
#22700=CARTESIAN_POINT('Ctrl Pts',(1.04703182236286E-5,19.8008681397575,
-20.3843681978484));
#22701=CARTESIAN_POINT('Ctrl Pts',(7.40902886198214E-6,19.7999176631319,
-20.3833942117421));
#22702=CARTESIAN_POINT('Ctrl Pts',(4.53081936859977E-6,19.7990240295926,
-20.3824784747024));
#22703=CARTESIAN_POINT('Ctrl Pts',(2.93234049434048E-6,19.7982764424602,
-20.3817122953783));
#22704=CARTESIAN_POINT('Ctrl Pts',(1.92044015556725E-6,19.7976595188611,
-20.3810799307538));
#22705=CARTESIAN_POINT('Ctrl Pts',(9.7728613478454E-7,19.7970845077156,
-20.3804905276126));
#22706=CARTESIAN_POINT('Ctrl Pts',(5.43064674007645E-7,19.7966231564816,
-20.3800175251989));
#22707=CARTESIAN_POINT('Ctrl Pts',(2.92653819400357E-7,19.7962322344865,
-20.3796166523707));
#22708=CARTESIAN_POINT('Ctrl Pts',(7.44390397725664E-8,19.7958915745054,
-20.3792673209648));
#22709=CARTESIAN_POINT('Ctrl Pts',(-2.22066279043125E-16,19.7956041314054,
-20.3789724910909));
#22710=CARTESIAN_POINT('Ctrl Pts',(-2.22044604925031E-16,19.7953186364093,
-20.3786796564404));
#22711=CARTESIAN_POINT('',(0.,20.1476593182046,-20.026338974645));
#22712=CARTESIAN_POINT('Ctrl Pts',(0.00185295431591431,19.8682455202995,
-20.4532144101331));
#22713=CARTESIAN_POINT('Ctrl Pts',(0.0210291123338008,20.2475554365488,
-20.8386547994645));
#22714=CARTESIAN_POINT('Ctrl Pts',(0.19417406045939,20.6353433627736,-21.1941740604579));
#22715=CARTESIAN_POINT('Ctrl Pts',(0.439339828216959,20.9273329823489,-21.439339828217));
#22716=CARTESIAN_POINT('Ctrl Pts',(0.00185295431591403,20.1036752647639,
-20.2177846656687));
#22717=CARTESIAN_POINT('Ctrl Pts',(0.0210291123338009,20.4850286720406,
-20.6011815639727));
#22718=CARTESIAN_POINT('Ctrl Pts',(0.194174060459389,20.8620603765216,-20.9674570467099));
#22719=CARTESIAN_POINT('Ctrl Pts',(0.439339828216958,21.1384420454914,-21.2282307650744));
#22720=CARTESIAN_POINT('Ctrl Pts',(0.00185295431591376,20.3391050092284,
-19.9823549212043));
#22721=CARTESIAN_POINT('Ctrl Pts',(0.021029112333801,20.7225019075324,-20.3637083284809));
#22722=CARTESIAN_POINT('Ctrl Pts',(0.194174060459389,21.0887773902696,-20.740740032962));
#22723=CARTESIAN_POINT('Ctrl Pts',(0.439339828216957,21.349551108634,-21.0171217019318));
#22724=CARTESIAN_POINT('Ctrl Pts',(0.00185295431591348,20.5745347536928,
-19.7469251767398));
#22725=CARTESIAN_POINT('Ctrl Pts',(0.0210291123338011,20.9599751430241,
-20.1262350929892));
#22726=CARTESIAN_POINT('Ctrl Pts',(0.194174060459389,21.3154944040175,-20.514023019214));
#22727=CARTESIAN_POINT('Ctrl Pts',(0.439339828216956,21.5606601717766,-20.8060126387892));
#22728=CARTESIAN_POINT('',(0.439339828216882,21.5606601717765,-20.8060126387891));
#22729=CARTESIAN_POINT('Ctrl Pts',(0.00185295431591348,20.5745347536928,
-19.7469251767398));
#22730=CARTESIAN_POINT('Ctrl Pts',(0.0210291123338011,20.9599751430241,
-20.1262350929892));
#22731=CARTESIAN_POINT('Ctrl Pts',(0.194174060459389,21.3154944040175,-20.514023019214));
#22732=CARTESIAN_POINT('Ctrl Pts',(0.439339828216956,21.5606601717766,-20.8060126387892));
#22733=CARTESIAN_POINT('',(0.439339828217853,20.9273329823471,-21.4393398282178));
#22734=CARTESIAN_POINT('',(0.439339828216882,21.5606601717765,-20.8060126387891));
#22735=CARTESIAN_POINT('Ctrl Pts',(0.439339828216959,20.9273329823489,-21.439339828217));
#22736=CARTESIAN_POINT('Ctrl Pts',(0.19417406045939,20.6353433627736,-21.1941740604579));
#22737=CARTESIAN_POINT('Ctrl Pts',(0.0210291123338008,20.2475554365488,
-20.8386547994645));
#22738=CARTESIAN_POINT('Ctrl Pts',(0.00185295431591431,19.8682455202995,
-20.4532144101331));
#22739=CARTESIAN_POINT('Ctrl Pts',(1.49999999999999,22.,-21.7953186364092));
#22740=CARTESIAN_POINT('Ctrl Pts',(1.21626217779757,22.,-21.5192990451721));
#22741=CARTESIAN_POINT('Ctrl Pts',(0.921462981006754,21.9185839147642,-21.2520540356058));
#22742=CARTESIAN_POINT('Ctrl Pts',(0.662909388853527,21.7447004895678,-21.0317299497988));
#22743=CARTESIAN_POINT('Ctrl Pts',(1.40374142648193,21.8220460536244,-21.9339538507548));
#22744=CARTESIAN_POINT('Ctrl Pts',(1.1406737996242,21.8044458905108,-21.6760317112072));
#22745=CARTESIAN_POINT('Ctrl Pts',(0.877124322932673,21.7115209147256,-21.4308516926654));
#22746=CARTESIAN_POINT('Ctrl Pts',(0.65642758371972,21.5472709534839,-21.2356412910166));
#22747=CARTESIAN_POINT('Ctrl Pts',(1.30748285296387,21.6440921072489,-22.0725890651003));
#22748=CARTESIAN_POINT('Ctrl Pts',(1.06508542145083,21.6088917810216,-21.8327643772423));
#22749=CARTESIAN_POINT('Ctrl Pts',(0.832785664858593,21.504457914687,-21.6096493497249));
#22750=CARTESIAN_POINT('Ctrl Pts',(0.649945778585914,21.3498414173999,-21.4395526322343));
#22751=CARTESIAN_POINT('Ctrl Pts',(1.21122427944581,21.4661381608733,-22.2112242794458));
#22752=CARTESIAN_POINT('Ctrl Pts',(0.989497043277452,21.4133376715324,-21.9894970432775));
#22753=CARTESIAN_POINT('Ctrl Pts',(0.788447006784511,21.2973949146484,-21.7884470067845));
#22754=CARTESIAN_POINT('Ctrl Pts',(0.643463973452107,21.152411881316,-21.6434639734521));
#22755=CARTESIAN_POINT('',(1.49999999999999,22.,-21.7953186364092));
#22756=CARTESIAN_POINT('',(1.21122427944581,21.4661381608733,-22.2112242794458));
#22757=CARTESIAN_POINT('',(1.49999999999999,22.,-21.7953186364092));
#22758=CARTESIAN_POINT('',(0.643463973452109,21.152411881316,-21.6434639734521));
#22759=CARTESIAN_POINT('Ctrl Pts',(1.21122427944581,21.4661381608733,-22.2112242794458));
#22760=CARTESIAN_POINT('Ctrl Pts',(0.989497043277452,21.4133376715324,-21.9894970432775));
#22761=CARTESIAN_POINT('Ctrl Pts',(0.788447006784511,21.2973949146484,-21.7884470067845));
#22762=CARTESIAN_POINT('Ctrl Pts',(0.643463973452107,21.152411881316,-21.6434639734521));
#22763=CARTESIAN_POINT('',(0.662909388853531,21.7447004895678,-21.0317299497988));
#22764=CARTESIAN_POINT('',(0.643463973452109,21.152411881316,-21.6434639734521));
#22765=CARTESIAN_POINT('Ctrl Pts',(0.662909388853527,21.7447004895678,-21.0317299497988));
#22766=CARTESIAN_POINT('Ctrl Pts',(0.921462981006754,21.9185839147642,-21.2520540356058));
#22767=CARTESIAN_POINT('Ctrl Pts',(1.21626217779757,22.,-21.5192990451721));
#22768=CARTESIAN_POINT('Ctrl Pts',(1.49999999999999,22.,-21.7953186364092));
#22769=CARTESIAN_POINT('Ctrl Pts',(0.43933982821688,20.9273329823488,-21.4393398282169));
#22770=CARTESIAN_POINT('Ctrl Pts',(0.509453252888523,21.0108372675684,-21.5094532528885));
#22771=CARTESIAN_POINT('Ctrl Pts',(0.576934137750669,21.0858820456145,-21.5769341377507));
#22772=CARTESIAN_POINT('Ctrl Pts',(0.643463973452108,21.152411881316,-21.6434639734521));
#22773=CARTESIAN_POINT('Ctrl Pts',(0.43933982821688,21.1384420454913,-21.2282307650743));
#22774=CARTESIAN_POINT('Ctrl Pts',(0.509453252888438,21.2174827105284,-21.3028078099286));
#22775=CARTESIAN_POINT('Ctrl Pts',(0.579610088542197,21.2880143685876,-21.3730586867583));
#22776=CARTESIAN_POINT('Ctrl Pts',(0.649945778585916,21.3498414173999,-21.4395526322343));
#22777=CARTESIAN_POINT('Ctrl Pts',(0.439339828216881,21.3495511086339,-21.0171217019317));
#22778=CARTESIAN_POINT('Ctrl Pts',(0.509453252888354,21.4241281534884,-21.0961623669687));
#22779=CARTESIAN_POINT('Ctrl Pts',(0.582286039333725,21.4901466915607,-21.169183235766));
#22780=CARTESIAN_POINT('Ctrl Pts',(0.656427583719724,21.5472709534839,-21.2356412910166));
#22781=CARTESIAN_POINT('Ctrl Pts',(0.439339828216881,21.5606601717765,-20.8060126387891));
#22782=CARTESIAN_POINT('Ctrl Pts',(0.509453252888269,21.6307735964483,-20.8895169240087));
#22783=CARTESIAN_POINT('Ctrl Pts',(0.584961990125253,21.6922790145338,-20.9653077847737));
#22784=CARTESIAN_POINT('Ctrl Pts',(0.662909388853532,21.7447004895678,-21.0317299497988));
#22785=CARTESIAN_POINT('Ctrl Pts',(0.643463973452108,21.152411881316,-21.6434639734521));
#22786=CARTESIAN_POINT('Ctrl Pts',(0.576934137750669,21.0858820456145,-21.5769341377507));
#22787=CARTESIAN_POINT('Ctrl Pts',(0.509453252888523,21.0108372675684,-21.5094532528885));
#22788=CARTESIAN_POINT('Ctrl Pts',(0.43933982821688,20.9273329823488,-21.4393398282169));
#22789=CARTESIAN_POINT('Ctrl Pts',(0.439339828216881,21.5606601717765,-20.8060126387891));
#22790=CARTESIAN_POINT('Ctrl Pts',(0.509453252888269,21.6307735964483,-20.8895169240087));
#22791=CARTESIAN_POINT('Ctrl Pts',(0.584961990125253,21.6922790145338,-20.9653077847737));
#22792=CARTESIAN_POINT('Ctrl Pts',(0.662909388853532,21.7447004895678,-21.0317299497988));
#22793=CARTESIAN_POINT('Origin',(5.30177669529664,21.75,-25.9482233047034));
#22794=CARTESIAN_POINT('',(1.5,21.5,-22.5));
#22795=CARTESIAN_POINT('',(1.85355339059327,22.,-22.1464466094067));
#22796=CARTESIAN_POINT('',(1.5,21.5,-22.5));
#22797=CARTESIAN_POINT('',(2.85355339059327,22.,-23.1464466094067));
#22798=CARTESIAN_POINT('',(5.47855339059327,22.,-25.7714466094067));
#22799=CARTESIAN_POINT('',(2.5,21.5,-23.5));
#22800=CARTESIAN_POINT('',(2.85355339059327,22.,-23.1464466094067));
#22801=CARTESIAN_POINT('',(5.12500000000001,21.5,-26.125));
#22802=CARTESIAN_POINT('Ctrl Pts',(1.21122427944581,21.4661381608733,-22.2112242794458));
#22803=CARTESIAN_POINT('Ctrl Pts',(1.30519315757561,21.4885152167272,-22.3051931575756));
#22804=CARTESIAN_POINT('Ctrl Pts',(1.40259226494897,21.5,-22.402592264949));
#22805=CARTESIAN_POINT('Ctrl Pts',(1.5,21.5,-22.5));
#22806=CARTESIAN_POINT('Ctrl Pts',(1.30748285296387,21.6440921072489,-22.0725890651003));
#22807=CARTESIAN_POINT('Ctrl Pts',(1.4102118414925,21.6590101444848,-22.17422771471));
#22808=CARTESIAN_POINT('Ctrl Pts',(1.51394954614333,21.6666666666667,-22.2782472857478));
#22809=CARTESIAN_POINT('Ctrl Pts',(1.61785113019775,21.6666666666667,-22.3821488698022));
#22810=CARTESIAN_POINT('Ctrl Pts',(1.40374142648192,21.8220460536244,-21.9339538507548));
#22811=CARTESIAN_POINT('Ctrl Pts',(1.5152305254094,21.8295050722424,-22.0432622718444));
#22812=CARTESIAN_POINT('Ctrl Pts',(1.62530682733768,21.8333333333333,-22.1539023065467));
#22813=CARTESIAN_POINT('Ctrl Pts',(1.73570226039551,21.8333333333333,-22.2642977396045));
#22814=CARTESIAN_POINT('Ctrl Pts',(1.49999999999998,22.,-21.7953186364092));
#22815=CARTESIAN_POINT('Ctrl Pts',(1.62024920932629,22.,-21.9122968289787));
#22816=CARTESIAN_POINT('Ctrl Pts',(1.73666410853204,22.,-22.0295573273455));
#22817=CARTESIAN_POINT('Ctrl Pts',(1.85355339059327,22.,-22.1464466094067));
#22818=CARTESIAN_POINT('Ctrl Pts',(1.5,21.5,-22.5));
#22819=CARTESIAN_POINT('Ctrl Pts',(1.40259226494897,21.5,-22.402592264949));
#22820=CARTESIAN_POINT('Ctrl Pts',(1.30519315757561,21.4885152167272,-22.3051931575756));
#22821=CARTESIAN_POINT('Ctrl Pts',(1.21122427944581,21.4661381608733,-22.2112242794458));
#22822=CARTESIAN_POINT('Ctrl Pts',(1.49999999999998,22.,-21.7953186364092));
#22823=CARTESIAN_POINT('Ctrl Pts',(1.62024920932629,22.,-21.9122968289787));
#22824=CARTESIAN_POINT('Ctrl Pts',(1.73666410853204,22.,-22.0295573273455));
#22825=CARTESIAN_POINT('Ctrl Pts',(1.85355339059327,22.,-22.1464466094067));
#22826=CARTESIAN_POINT('Ctrl Pts',(3.96827005020121,21.7447004895678,-24.3370906111465));
#22827=CARTESIAN_POINT('Ctrl Pts',(3.74794596439424,21.9185839147642,-24.0785370189932));
#22828=CARTESIAN_POINT('Ctrl Pts',(3.48070095482788,22.,-23.7837378222024));
#22829=CARTESIAN_POINT('Ctrl Pts',(3.20468136359074,22.,-23.5));
#22830=CARTESIAN_POINT('Ctrl Pts',(3.76435870898344,21.5472709534839,-24.3435724162803));
#22831=CARTESIAN_POINT('Ctrl Pts',(3.56914830733465,21.7115209147256,-24.1228756770673));
#22832=CARTESIAN_POINT('Ctrl Pts',(3.32396828879277,21.8044458905108,-23.8593262003758));
#22833=CARTESIAN_POINT('Ctrl Pts',(3.06604614924522,21.8220460536244,-23.5962585735181));
#22834=CARTESIAN_POINT('Ctrl Pts',(3.56044736776567,21.3498414173999,-24.3500542214141));
#22835=CARTESIAN_POINT('Ctrl Pts',(3.39035065027507,21.504457914687,-24.1672143351414));
#22836=CARTESIAN_POINT('Ctrl Pts',(3.16723562275766,21.6088917810216,-23.9349145785492));
#22837=CARTESIAN_POINT('Ctrl Pts',(2.9274109348997,21.6440921072489,-23.6925171470361));
#22838=CARTESIAN_POINT('Ctrl Pts',(3.35653602654789,21.152411881316,-24.3565360265479));
#22839=CARTESIAN_POINT('Ctrl Pts',(3.21155299321549,21.2973949146484,-24.2115529932155));
#22840=CARTESIAN_POINT('Ctrl Pts',(3.01050295672254,21.4133376715324,-24.0105029567225));
#22841=CARTESIAN_POINT('Ctrl Pts',(2.78877572055418,21.4661381608733,-23.7887757205542));
#22842=CARTESIAN_POINT('',(2.78877572055418,21.4661381608733,-23.7887757205542));
#22843=CARTESIAN_POINT('',(3.20468136359075,22.,-23.5));
#22844=CARTESIAN_POINT('',(2.78877572055418,21.4661381608733,-23.7887757205542));
#22845=CARTESIAN_POINT('',(3.96827005020121,21.7447004895678,-24.3370906111465));
#22846=CARTESIAN_POINT('Ctrl Pts',(3.20468136359074,22.,-23.5));
#22847=CARTESIAN_POINT('Ctrl Pts',(3.48070095482788,22.,-23.7837378222024));
#22848=CARTESIAN_POINT('Ctrl Pts',(3.74794596439424,21.9185839147642,-24.0785370189932));
#22849=CARTESIAN_POINT('Ctrl Pts',(3.96827005020121,21.7447004895678,-24.3370906111465));
#22850=CARTESIAN_POINT('',(3.35653602654789,21.152411881316,-24.3565360265479));
#22851=CARTESIAN_POINT('',(3.96827005020121,21.7447004895678,-24.3370906111465));
#22852=CARTESIAN_POINT('Ctrl Pts',(3.35653602654789,21.152411881316,-24.3565360265479));
#22853=CARTESIAN_POINT('Ctrl Pts',(3.21155299321549,21.2973949146484,-24.2115529932155));
#22854=CARTESIAN_POINT('Ctrl Pts',(3.01050295672254,21.4133376715324,-24.0105029567225));
#22855=CARTESIAN_POINT('Ctrl Pts',(2.78877572055418,21.4661381608733,-23.7887757205542));
#22856=CARTESIAN_POINT('Ctrl Pts',(2.5,21.5,-23.5));
#22857=CARTESIAN_POINT('Ctrl Pts',(2.59740773505102,21.5,-23.597407735051));
#22858=CARTESIAN_POINT('Ctrl Pts',(2.69480684242438,21.4885152167272,-23.6948068424244));
#22859=CARTESIAN_POINT('Ctrl Pts',(2.78877572055418,21.4661381608733,-23.7887757205542));
#22860=CARTESIAN_POINT('Ctrl Pts',(2.61785113019776,21.6666666666667,-23.3821488698022));
#22861=CARTESIAN_POINT('Ctrl Pts',(2.72175271425219,21.6666666666667,-23.4860504538567));
#22862=CARTESIAN_POINT('Ctrl Pts',(2.82577228529002,21.6590101444848,-23.5897881585075));
#22863=CARTESIAN_POINT('Ctrl Pts',(2.92741093489971,21.6440921072489,-23.6925171470361));
#22864=CARTESIAN_POINT('Ctrl Pts',(2.73570226039552,21.8333333333333,-23.2642977396045));
#22865=CARTESIAN_POINT('Ctrl Pts',(2.84609769345335,21.8333333333333,-23.3746931726623));
#22866=CARTESIAN_POINT('Ctrl Pts',(2.95673772815565,21.8295050722424,-23.4847694745906));
#22867=CARTESIAN_POINT('Ctrl Pts',(3.06604614924523,21.8220460536244,-23.5962585735181));
#22868=CARTESIAN_POINT('Ctrl Pts',(2.85355339059328,22.,-23.1464466094067));
#22869=CARTESIAN_POINT('Ctrl Pts',(2.97044267265451,22.,-23.263335891468));
#22870=CARTESIAN_POINT('Ctrl Pts',(3.08770317102128,22.,-23.3797507906737));
#22871=CARTESIAN_POINT('Ctrl Pts',(3.20468136359075,22.,-23.5));
#22872=CARTESIAN_POINT('Ctrl Pts',(2.78877572055418,21.4661381608733,-23.7887757205542));
#22873=CARTESIAN_POINT('Ctrl Pts',(2.69480684242438,21.4885152167272,-23.6948068424244));
#22874=CARTESIAN_POINT('Ctrl Pts',(2.59740773505102,21.5,-23.597407735051));
#22875=CARTESIAN_POINT('Ctrl Pts',(2.5,21.5,-23.5));
#22876=CARTESIAN_POINT('Ctrl Pts',(2.85355339059328,22.,-23.1464466094067));
#22877=CARTESIAN_POINT('Ctrl Pts',(2.97044267265451,22.,-23.263335891468));
#22878=CARTESIAN_POINT('Ctrl Pts',(3.08770317102128,22.,-23.3797507906737));
#22879=CARTESIAN_POINT('Ctrl Pts',(3.20468136359075,22.,-23.5));
#22880=CARTESIAN_POINT('Ctrl Pts',(3.56066017178304,20.9273329823489,-24.560660171783));
#22881=CARTESIAN_POINT('Ctrl Pts',(3.8058259395421,20.6353433627736,-24.8058259395406));
#22882=CARTESIAN_POINT('Ctrl Pts',(4.16134520053552,20.2475554365488,-24.9789708876662));
#22883=CARTESIAN_POINT('Ctrl Pts',(4.54678558986685,19.8682455202995,-24.9981470456841));
#22884=CARTESIAN_POINT('Ctrl Pts',(3.77176923492562,21.1384420454914,-24.560660171783));
#22885=CARTESIAN_POINT('Ctrl Pts',(4.03254295329006,20.8620603765216,-24.8058259395406));
#22886=CARTESIAN_POINT('Ctrl Pts',(4.39881843602729,20.4850286720406,-24.9789708876662));
#22887=CARTESIAN_POINT('Ctrl Pts',(4.7822153343313,20.1036752647639,-24.9981470456841));
#22888=CARTESIAN_POINT('Ctrl Pts',(3.9828782980682,21.349551108634,-24.560660171783));
#22889=CARTESIAN_POINT('Ctrl Pts',(4.25925996703803,21.0887773902696,-24.8058259395406));
#22890=CARTESIAN_POINT('Ctrl Pts',(4.63629167151906,20.7225019075324,-24.9789708876662));
#22891=CARTESIAN_POINT('Ctrl Pts',(5.01764507879574,20.3391050092283,-24.9981470456841));
#22892=CARTESIAN_POINT('Ctrl Pts',(4.19398736121078,21.5606601717766,-24.560660171783));
#22893=CARTESIAN_POINT('Ctrl Pts',(4.48597698078599,21.3154944040175,-24.8058259395406));
#22894=CARTESIAN_POINT('Ctrl Pts',(4.87376490701083,20.9599751430241,-24.9789708876662));
#22895=CARTESIAN_POINT('Ctrl Pts',(5.25307482326019,20.5745347536928,-24.9981470456841));
#22896=CARTESIAN_POINT('',(3.56066017178215,20.9273329823471,-24.5606601717821));
#22897=CARTESIAN_POINT('Ctrl Pts',(4.54678558986685,19.8682455202995,-24.9981470456841));
#22898=CARTESIAN_POINT('Ctrl Pts',(4.16134520053552,20.2475554365488,-24.9789708876662));
#22899=CARTESIAN_POINT('Ctrl Pts',(3.8058259395421,20.6353433627736,-24.8058259395406));
#22900=CARTESIAN_POINT('Ctrl Pts',(3.56066017178304,20.9273329823489,-24.560660171783));
#22901=CARTESIAN_POINT('',(4.19398736121088,21.5606601717765,-24.5606601717831));
#22902=CARTESIAN_POINT('',(3.56066017178215,20.9273329823471,-24.5606601717821));
#22903=CARTESIAN_POINT('Ctrl Pts',(4.19398736121078,21.5606601717766,-24.560660171783));
#22904=CARTESIAN_POINT('Ctrl Pts',(4.48597698078599,21.3154944040175,-24.8058259395406));
#22905=CARTESIAN_POINT('Ctrl Pts',(4.87376490701083,20.9599751430241,-24.9789708876662));
#22906=CARTESIAN_POINT('Ctrl Pts',(5.25307482326019,20.5745347536928,-24.9981470456841));
#22907=CARTESIAN_POINT('Ctrl Pts',(3.35653602654789,21.1524118813159,-24.3565360265479));
#22908=CARTESIAN_POINT('Ctrl Pts',(3.42306586224933,21.0858820456145,-24.4230658622493));
#22909=CARTESIAN_POINT('Ctrl Pts',(3.49054674711148,21.0108372675684,-24.4905467471115));
#22910=CARTESIAN_POINT('Ctrl Pts',(3.56066017178311,20.9273329823488,-24.5606601717831));
#22911=CARTESIAN_POINT('Ctrl Pts',(3.56044736776567,21.3498414173999,-24.3500542214141));
#22912=CARTESIAN_POINT('Ctrl Pts',(3.62694131324166,21.2880143685876,-24.4203899114578));
#22913=CARTESIAN_POINT('Ctrl Pts',(3.6971921900714,21.2174827105284,-24.4905467471116));
#22914=CARTESIAN_POINT('Ctrl Pts',(3.7717692349257,21.1384420454914,-24.5606601717831));
#22915=CARTESIAN_POINT('Ctrl Pts',(3.76435870898344,21.5472709534839,-24.3435724162803));
#22916=CARTESIAN_POINT('Ctrl Pts',(3.830816764234,21.4901466915607,-24.4177139606663));
#22917=CARTESIAN_POINT('Ctrl Pts',(3.90383763303133,21.4241281534884,-24.4905467471116));
#22918=CARTESIAN_POINT('Ctrl Pts',(3.98287829806829,21.3495511086339,-24.5606601717831));
#22919=CARTESIAN_POINT('Ctrl Pts',(3.96827005020121,21.7447004895678,-24.3370906111465));
#22920=CARTESIAN_POINT('Ctrl Pts',(4.03469221522633,21.6922790145338,-24.4150380098747));
#22921=CARTESIAN_POINT('Ctrl Pts',(4.11048307599125,21.6307735964483,-24.4905467471117));
#22922=CARTESIAN_POINT('Ctrl Pts',(4.19398736121087,21.5606601717765,-24.5606601717831));
#22923=CARTESIAN_POINT('Ctrl Pts',(3.56066017178311,20.9273329823488,-24.5606601717831));
#22924=CARTESIAN_POINT('Ctrl Pts',(3.49054674711148,21.0108372675684,-24.4905467471115));
#22925=CARTESIAN_POINT('Ctrl Pts',(3.42306586224933,21.0858820456145,-24.4230658622493));
#22926=CARTESIAN_POINT('Ctrl Pts',(3.35653602654789,21.1524118813159,-24.3565360265479));
#22927=CARTESIAN_POINT('Ctrl Pts',(3.96827005020121,21.7447004895678,-24.3370906111465));
#22928=CARTESIAN_POINT('Ctrl Pts',(4.03469221522633,21.6922790145338,-24.4150380098747));
#22929=CARTESIAN_POINT('Ctrl Pts',(4.11048307599125,21.6307735964483,-24.4905467471117));
#22930=CARTESIAN_POINT('Ctrl Pts',(4.19398736121087,21.5606601717765,-24.5606601717831));
#22931=CARTESIAN_POINT('Origin',(1.5,20.5,-6.25));
#22932=CARTESIAN_POINT('',(0.,20.5,35.3786796564404));
#22933=CARTESIAN_POINT('',(0.,20.5,-6.25));
#22934=CARTESIAN_POINT('',(1.5,22.,35.3786796564404));
#22935=CARTESIAN_POINT('Origin',(1.5,20.5,35.3786796564404));
#22936=CARTESIAN_POINT('',(1.5,22.,-6.25));
#22937=CARTESIAN_POINT('Origin',(0.,-22.,-21.));
#22938=CARTESIAN_POINT('',(0.,-20.5,-20.3786796564404));
#22939=CARTESIAN_POINT('',(0.,-22.,-20.3786796564404));
#22940=CARTESIAN_POINT('',(0.,-20.5,35.3786796564404));
#22941=CARTESIAN_POINT('',(0.,-20.5,-6.25));
#22942=CARTESIAN_POINT('',(0.,-22.,35.3786796564404));
#22943=CARTESIAN_POINT('Origin',(1.5,-22.,-20.3786796564404));
#22944=CARTESIAN_POINT('',(0.439339828220176,-20.5,-21.4393398282202));
#22945=CARTESIAN_POINT('',(0.439339828220176,-22.,-21.4393398282202));
#22946=CARTESIAN_POINT('Origin',(1.5,-20.5,-20.3786796564404));
#22947=CARTESIAN_POINT('Origin',(4.,-22.,-25.));
#22948=CARTESIAN_POINT('',(3.56066017177982,-20.5,-24.5606601717798));
#22949=CARTESIAN_POINT('',(3.56066017177982,-22.,-24.5606601717798));
#22950=CARTESIAN_POINT('',(5.125,-20.5,-26.125));
#22951=CARTESIAN_POINT('Origin',(56.,-20.5,-23.5));
#22952=CARTESIAN_POINT('',(61.5,-22.,-23.5));
#22953=CARTESIAN_POINT('',(61.5,-20.5,-25.));
#22954=CARTESIAN_POINT('Origin',(61.5,-20.5,-23.5));
#22955=CARTESIAN_POINT('',(68.5,-20.5,-25.));
#22956=CARTESIAN_POINT('',(56.,-20.5,-25.));
#22957=CARTESIAN_POINT('',(68.5,-22.,-23.5));
#22958=CARTESIAN_POINT('Origin',(68.5,-20.5,-23.5));
#22959=CARTESIAN_POINT('',(56.,-22.,-23.5));
#22960=CARTESIAN_POINT('Origin',(68.5,-20.5,-23.5));
#22961=CARTESIAN_POINT('',(70.,-20.5,-23.5));
#22962=CARTESIAN_POINT('Origin',(68.5,-20.5,-23.5));
#22963=CARTESIAN_POINT('Origin',(68.5,-20.5,-23.5));
#22964=CARTESIAN_POINT('Origin',(61.5,-20.5,-23.5));
#22965=CARTESIAN_POINT('Origin',(61.5,-20.5,-23.5));
#22966=CARTESIAN_POINT('Origin',(61.5,-20.5,-23.5));
#22967=CARTESIAN_POINT('Origin',(68.5,-20.5,4.25));
#22968=CARTESIAN_POINT('',(70.,-20.5,-17.5712833908056));
#22969=CARTESIAN_POINT('',(70.,-20.5,4.25));
#22970=CARTESIAN_POINT('',(68.5,-22.,-15.6524758424985));
#22971=CARTESIAN_POINT('Ctrl Pts',(68.5,-22.,-15.6524758424985));
#22972=CARTESIAN_POINT('Ctrl Pts',(68.5946178513885,-22.,-15.6524758424985));
#22973=CARTESIAN_POINT('Ctrl Pts',(68.6889643978921,-21.9909261474626,-15.665250854624));
#22974=CARTESIAN_POINT('Ctrl Pts',(68.8710686191993,-21.9563375109926,-15.7136914161295));
#22975=CARTESIAN_POINT('Ctrl Pts',(68.9588244922017,-21.9308152339295,-15.7493583883479));
#22976=CARTESIAN_POINT('Ctrl Pts',(69.2051881089356,-21.8355590404292,-15.88144036437));
#22977=CARTESIAN_POINT('Ctrl Pts',(69.3468785813891,-21.7463710185311,-16.0037159774975));
#22978=CARTESIAN_POINT('Ctrl Pts',(69.6391148171733,-21.5040391092436,-16.3291117577357));
#22979=CARTESIAN_POINT('Ctrl Pts',(69.7765132729404,-21.3178359703858,-16.572666547787));
#22980=CARTESIAN_POINT('Ctrl Pts',(69.9575260447372,-20.9170846786411,-17.0756837501162));
#22981=CARTESIAN_POINT('Ctrl Pts',(70.,-20.7022477383282,-17.3353257465337));
#22982=CARTESIAN_POINT('Ctrl Pts',(70.,-20.5,-17.5712833908056));
#22983=CARTESIAN_POINT('',(68.5,-22.,4.25));
#22984=CARTESIAN_POINT('Origin',(68.5,-22.,-23.5));
#22985=CARTESIAN_POINT('',(68.5,-10.1980390271856,-25.));
#22986=CARTESIAN_POINT('',(68.5,-22.,-25.));
#22987=CARTESIAN_POINT('',(70.,-13.2947358003083,-23.5));
#22988=CARTESIAN_POINT('Ctrl Pts',(70.,-13.2947358003083,-23.5));
#22989=CARTESIAN_POINT('Ctrl Pts',(70.,-12.5253526611459,-23.9352657686969));
#22990=CARTESIAN_POINT('Ctrl Pts',(69.8122976763679,-11.5896482415098,-24.3983540225569));
#22991=CARTESIAN_POINT('Ctrl Pts',(69.2682778073745,-10.6853817343331,-24.7965377420129));
#22992=CARTESIAN_POINT('Ctrl Pts',(69.099996626182,-10.4648018594106,-24.889928820497));
#22993=CARTESIAN_POINT('Ctrl Pts',(68.8470061948633,-10.2945164376804,-24.9604604345961));
#22994=CARTESIAN_POINT('Ctrl Pts',(68.7815873963742,-10.2591413018302,-24.97500159694));
#22995=CARTESIAN_POINT('Ctrl Pts',(68.64269539724,-10.2107026186997,-24.9948442089972));
#22996=CARTESIAN_POINT('Ctrl Pts',(68.5690622745619,-10.1980390271856,-25.));
#22997=CARTESIAN_POINT('Ctrl Pts',(68.5,-10.1980390271856,-25.));
#22998=CARTESIAN_POINT('',(70.,-22.,-23.5));
#22999=CARTESIAN_POINT('Origin',(70.,-22.,-25.));
#23000=CARTESIAN_POINT('',(61.5,-10.1980390271856,-25.));
#23001=CARTESIAN_POINT('',(61.5,-22.,-25.));
#23002=CARTESIAN_POINT('',(75.5,-10.1980390271856,-25.));
#23003=CARTESIAN_POINT('Origin',(82.5,20.5,21.2280731570623));
#23004=CARTESIAN_POINT('',(82.5,22.,21.2280731570623));
#23005=CARTESIAN_POINT('Origin',(82.5,20.5,21.2280731570623));
#23006=CARTESIAN_POINT('',(84.,20.5,21.2280731570623));
#23007=CARTESIAN_POINT('Origin',(82.5,20.5,21.2280731570623));
#23008=CARTESIAN_POINT('Origin',(82.5,20.5,21.2280731570623));
#23009=CARTESIAN_POINT('Origin',(82.5,-22.,21.2280731570623));
#23010=CARTESIAN_POINT('',(84.,16.6843912097029,21.2280731570623));
#23011=CARTESIAN_POINT('Ctrl Pts',(84.,16.6843912097029,21.2280731570623));
#23012=CARTESIAN_POINT('Ctrl Pts',(84.,16.424239791648,21.4325414571512));
#23013=CARTESIAN_POINT('Ctrl Pts',(83.9566902724278,16.1377744699131,21.6492625703158));
#23014=CARTESIAN_POINT('Ctrl Pts',(83.7720906996842,15.5809736161534,22.053380597491));
#23015=CARTESIAN_POINT('Ctrl Pts',(83.6323380105135,15.3103686972935,22.2411069388649));
#23016=CARTESIAN_POINT('Ctrl Pts',(83.4216450393869,15.0568236851315,22.4118978779271));
#23017=CARTESIAN_POINT('Ctrl Pts',(83.3973987301277,15.0292019594189,22.4304294784802));
#23018=CARTESIAN_POINT('Ctrl Pts',(83.3718572905786,15.0019020194829,22.4486733638724));
#23019=CARTESIAN_POINT('',(84.,-22.,21.2280731570623));
#23020=CARTESIAN_POINT('Origin',(82.5,20.5,15.25));
#23021=CARTESIAN_POINT('',(84.,20.5,17.5712833908056));
#23022=CARTESIAN_POINT('',(82.5,22.,15.6524758424985));
#23023=CARTESIAN_POINT('Ctrl Pts',(82.5,22.,15.6524758424985));
#23024=CARTESIAN_POINT('Ctrl Pts',(82.5946178513885,22.,15.6524758424985));
#23025=CARTESIAN_POINT('Ctrl Pts',(82.6889643978921,21.9909261474626,15.665250854624));
#23026=CARTESIAN_POINT('Ctrl Pts',(82.8710686191993,21.9563375109926,15.7136914161295));
#23027=CARTESIAN_POINT('Ctrl Pts',(82.9588244922017,21.9308152339295,15.7493583883479));
#23028=CARTESIAN_POINT('Ctrl Pts',(83.2051881089356,21.8355590404292,15.88144036437));
#23029=CARTESIAN_POINT('Ctrl Pts',(83.3468785813891,21.7463710185311,16.0037159774975));
#23030=CARTESIAN_POINT('Ctrl Pts',(83.6391148171733,21.5040391092436,16.3291117577357));
#23031=CARTESIAN_POINT('Ctrl Pts',(83.7765132729403,21.3178359703858,16.572666547787));
#23032=CARTESIAN_POINT('Ctrl Pts',(83.9575260447373,20.9170846786411,17.0756837501162));
#23033=CARTESIAN_POINT('Ctrl Pts',(84.,20.7022477383282,17.3353257465337));
#23034=CARTESIAN_POINT('Ctrl Pts',(84.,20.5,17.5712833908056));
#23035=CARTESIAN_POINT('',(82.5,22.,15.25));
#23036=CARTESIAN_POINT('',(84.,20.5,15.25));
#23037=CARTESIAN_POINT('Origin',(55.5193024198872,20.5,40.5));
#23038=CARTESIAN_POINT('',(55.5193024198872,20.5,42.));
#23039=CARTESIAN_POINT('',(55.5193024198872,22.,40.5));
#23040=CARTESIAN_POINT('Origin',(55.5193024198872,20.5,40.5));
#23041=CARTESIAN_POINT('Origin',(55.5193024198872,20.5,40.5));
#23042=CARTESIAN_POINT('Origin',(55.5193024198872,20.5,40.5));
#23043=CARTESIAN_POINT('Origin',(55.5193024198872,-20.5,40.5));
#23044=CARTESIAN_POINT('',(55.5193024198872,-20.5,42.));
#23045=CARTESIAN_POINT('Origin',(55.5193024198872,-20.5,40.5));
#23046=CARTESIAN_POINT('Origin',(55.5193024198872,-20.5,40.5));
#23047=CARTESIAN_POINT('Origin',(55.5193024198872,-22.,40.5));
#23048=CARTESIAN_POINT('',(55.5193024198872,-22.,42.));
#23049=CARTESIAN_POINT('Origin',(58.4153048715835,20.5,38.4314268202169));
#23050=CARTESIAN_POINT('',(58.4153048715835,22.,38.4314268202169));
#23051=CARTESIAN_POINT('Origin',(6.62132034355964,20.5,40.5));
#23052=CARTESIAN_POINT('',(5.56066017177982,20.5,41.5606601717798));
#23053=CARTESIAN_POINT('',(6.62132034355964,22.,40.5));
#23054=CARTESIAN_POINT('Origin',(6.62132034355965,20.5,40.5));
#23055=CARTESIAN_POINT('',(6.62132034355964,20.5,42.));
#23056=CARTESIAN_POINT('Origin',(6.62132034355964,20.5,40.5));
#23057=CARTESIAN_POINT('Origin',(6.62132034355964,20.5,40.5));
#23058=CARTESIAN_POINT('Origin',(6.62132034355964,-20.5,40.5));
#23059=CARTESIAN_POINT('',(6.62132034355964,-20.5,42.));
#23060=CARTESIAN_POINT('',(5.56066017177982,-20.5,41.5606601717798));
#23061=CARTESIAN_POINT('Origin',(6.62132034355964,-20.5,40.5));
#23062=CARTESIAN_POINT('Origin',(6.62132034355965,-20.5,40.5));
#23063=CARTESIAN_POINT('Origin',(6.62132034355964,-20.5,40.5));
#23064=CARTESIAN_POINT('Origin',(6.62132034355964,-22.,40.5));
#23065=CARTESIAN_POINT('',(6.62132034355964,-22.,42.));
#23066=CARTESIAN_POINT('',(5.56066017177982,-22.,41.5606601717798));
#23067=CARTESIAN_POINT('Origin',(24.,20.5,40.5));
#23068=CARTESIAN_POINT('',(24.,22.,40.5));
#23069=CARTESIAN_POINT('',(24.,20.5,42.));
#23070=CARTESIAN_POINT('Origin',(1.5,20.5,35.3786796564404));
#23071=CARTESIAN_POINT('',(0.439339828220176,20.5,36.4393398282202));
#23072=CARTESIAN_POINT('Origin',(1.5,20.5,35.3786796564404));
#23073=CARTESIAN_POINT('Origin',(1.5,20.5,35.3786796564404));
#23074=CARTESIAN_POINT('Origin',(1.5,-20.5,35.3786796564404));
#23075=CARTESIAN_POINT('',(0.439339828220176,-20.5,36.4393398282202));
#23076=CARTESIAN_POINT('Origin',(1.5,-20.5,35.3786796564404));
#23077=CARTESIAN_POINT('Origin',(1.5,-20.5,35.3786796564404));
#23078=CARTESIAN_POINT('Origin',(1.5,-20.5,35.3786796564404));
#23079=CARTESIAN_POINT('Origin',(1.5,-22.,35.3786796564404));
#23080=CARTESIAN_POINT('',(0.439339828220176,-22.,36.4393398282202));
#23081=CARTESIAN_POINT('Origin',(4.68566017177982,20.5,38.5643398282202));
#23082=CARTESIAN_POINT('',(4.68566017177982,22.,38.5643398282202));
#23083=CARTESIAN_POINT('',(3.625,20.5,39.625));
#23084=CARTESIAN_POINT('Origin',(4.62132034355965,-20.5,-23.5));
#23085=CARTESIAN_POINT('',(4.62132034355965,-20.5,-25.));
#23086=CARTESIAN_POINT('Origin',(4.62132034355965,-20.5,-23.5));
#23087=CARTESIAN_POINT('Origin',(4.62132034355965,-20.5,-23.5));
#23088=CARTESIAN_POINT('Origin',(4.62132034355964,-20.5,-23.5));
#23089=CARTESIAN_POINT('Origin',(56.,-20.5,-23.5));
#23090=CARTESIAN_POINT('',(13.5,-20.5,-25.));
#23091=CARTESIAN_POINT('Origin',(13.5,-20.5,-23.5));
#23092=CARTESIAN_POINT('',(56.,-20.5,-25.));
#23093=CARTESIAN_POINT('Origin',(13.5,-20.5,-23.5));
#23094=CARTESIAN_POINT('',(15.,-20.5,-23.5));
#23095=CARTESIAN_POINT('Origin',(13.5,-20.5,-23.5));
#23096=CARTESIAN_POINT('Origin',(13.5,-20.5,-23.5));
#23097=CARTESIAN_POINT('Origin',(6.18566017177982,-20.5,-25.0643398282202));
#23098=CARTESIAN_POINT('Origin',(1.5,-20.5,-20.3786796564404));
#23099=CARTESIAN_POINT('Origin',(4.62132034355965,-22.,-23.5));
#23100=CARTESIAN_POINT('',(4.62132034355965,-22.,-25.));
#23101=CARTESIAN_POINT('Origin',(13.5,20.5,-23.5));
#23102=CARTESIAN_POINT('',(13.5,20.5,-25.));
#23103=CARTESIAN_POINT('',(13.5,22.,-23.5));
#23104=CARTESIAN_POINT('Origin',(13.5,20.5,-23.5));
#23105=CARTESIAN_POINT('',(15.,20.5,-23.5));
#23106=CARTESIAN_POINT('Origin',(13.5,20.5,-23.5));
#23107=CARTESIAN_POINT('Origin',(13.5,20.5,-23.5));
#23108=CARTESIAN_POINT('Origin',(56.,20.5,-23.5));
#23109=CARTESIAN_POINT('',(56.,22.,-23.5));
#23110=CARTESIAN_POINT('',(56.,20.5,-25.));
#23111=CARTESIAN_POINT('Origin',(1.5,-20.5,-20.3786796564404));
#23112=CARTESIAN_POINT('Origin',(1.5,-20.5,-20.3786796564404));
#23113=CARTESIAN_POINT('Origin',(6.,-22.,42.));
#23114=CARTESIAN_POINT('',(24.,-20.5,42.));
#23115=CARTESIAN_POINT('',(32.5358115136623,-2.58526623249054,42.));
#23116=CARTESIAN_POINT('',(31.2738743424416,-2.24420189857483,42.));
#23117=CARTESIAN_POINT('Ctrl Pts',(32.5358115136623,-2.58526623249054,42.));
#23118=CARTESIAN_POINT('Ctrl Pts',(31.8298088014126,-2.58526623249054,42.));
#23119=CARTESIAN_POINT('Ctrl Pts',(31.2738743424416,-2.24420189857483,42.));
#23120=CARTESIAN_POINT('',(30.4314459860325,-1.31309688091278,42.));
#23121=CARTESIAN_POINT('Ctrl Pts',(31.2738743424416,-2.24420189857483,42.));
#23122=CARTESIAN_POINT('Ctrl Pts',(30.7179398834705,-1.90313756465912,42.));
#23123=CARTESIAN_POINT('Ctrl Pts',(30.4314459860325,-1.31309688091278,42.));
#23124=CARTESIAN_POINT('',(30.1449521258473,-0.0648021697998047,42.));
#23125=CARTESIAN_POINT('Ctrl Pts',(30.4314459860325,-1.31309688091278,42.));
#23126=CARTESIAN_POINT('Ctrl Pts',(30.1449521258473,-0.723056197166443,
42.));
#23127=CARTESIAN_POINT('Ctrl Pts',(30.1449521258473,-0.0648021697998047,
42.));
#23128=CARTESIAN_POINT('',(30.8134378492832,1.88437908887863,42.));
#23129=CARTESIAN_POINT('Ctrl Pts',(30.1449521258473,-0.0648021697998047,
42.));
#23130=CARTESIAN_POINT('Ctrl Pts',(30.1449521258473,1.1800816655159,42.));
#23131=CARTESIAN_POINT('Ctrl Pts',(30.8134378492832,1.88437908887863,42.));
#23132=CARTESIAN_POINT('',(32.5392223894596,2.58867621421814,42.));
#23133=CARTESIAN_POINT('Ctrl Pts',(30.8134378492832,1.88437908887863,42.));
#23134=CARTESIAN_POINT('Ctrl Pts',(31.4819234609604,2.58867621421814,42.));
#23135=CARTESIAN_POINT('Ctrl Pts',(32.5392223894596,2.58867621421814,42.));
#23136=CARTESIAN_POINT('',(33.7875168025494,2.25784420967102,42.));
#23137=CARTESIAN_POINT('Ctrl Pts',(32.5392223894596,2.58867621421814,42.));
#23138=CARTESIAN_POINT('Ctrl Pts',(33.23158249259,2.58867621421814,42.));
#23139=CARTESIAN_POINT('Ctrl Pts',(33.7875168025494,2.25784420967102,42.));
#23140=CARTESIAN_POINT('',(34.6350611746311,1.33526593446732,42.));
#23141=CARTESIAN_POINT('Ctrl Pts',(33.7875168025494,2.25784420967102,42.));
#23142=CARTESIAN_POINT('Ctrl Pts',(34.343451410532,1.92701190710068,42.));
#23143=CARTESIAN_POINT('Ctrl Pts',(34.6350611746311,1.33526593446732,42.));
#23144=CARTESIAN_POINT('',(34.9266712367535,-0.00682175159454346,42.));
#23145=CARTESIAN_POINT('Ctrl Pts',(34.6350611746311,1.33526593446732,42.));
#23146=CARTESIAN_POINT('Ctrl Pts',(34.9266712367535,0.74351966381073,42.));
#23147=CARTESIAN_POINT('Ctrl Pts',(34.9266712367535,-0.00682175159454346,
42.));
#23148=CARTESIAN_POINT('',(34.6197132766247,-1.36766731739044,42.));
#23149=CARTESIAN_POINT('Ctrl Pts',(34.9266712367535,-0.00682175159454346,
42.));
#23150=CARTESIAN_POINT('Ctrl Pts',(34.9266712367535,-0.767394304275513,
42.));
#23151=CARTESIAN_POINT('Ctrl Pts',(34.6197132766247,-1.36766731739044,42.));
#23152=CARTESIAN_POINT('',(33.7499998509884,-2.27660298347473,42.));
#23153=CARTESIAN_POINT('Ctrl Pts',(34.6197132766247,-1.36766731739044,42.));
#23154=CARTESIAN_POINT('Ctrl Pts',(34.3127556145191,-1.96793973445892,42.));
#23155=CARTESIAN_POINT('Ctrl Pts',(33.7499998509884,-2.27660298347473,42.));
#23156=CARTESIAN_POINT('Ctrl Pts',(33.7499998509884,-2.27660298347473,42.));
#23157=CARTESIAN_POINT('Ctrl Pts',(33.1872440874577,-2.58526623249054,42.));
#23158=CARTESIAN_POINT('Ctrl Pts',(32.5358115136623,-2.58526623249054,42.));
#23159=CARTESIAN_POINT('',(29.667462259531,1.90995901823044,42.));
#23160=CARTESIAN_POINT('',(28.0133013427258,1.90995901823044,42.));
#23161=CARTESIAN_POINT('',(17.8337311297655,1.90995901823044,42.));
#23162=CARTESIAN_POINT('',(28.0133013427258,-2.5,42.));
#23163=CARTESIAN_POINT('',(28.0133013427258,-10.0450204908848,42.));
#23164=CARTESIAN_POINT('',(27.3516370356083,-2.5,42.));
#23165=CARTESIAN_POINT('',(17.0066506713629,-2.5,42.));
#23166=CARTESIAN_POINT('',(27.3516370356083,1.90995901823044,42.));
#23167=CARTESIAN_POINT('',(27.3516370356083,-12.25,42.));
#23168=CARTESIAN_POINT('',(25.7042973488569,1.90995901823044,42.));
#23169=CARTESIAN_POINT('',(16.6758185178041,1.90995901823044,42.));
#23170=CARTESIAN_POINT('',(25.7042973488569,2.5,42.));
#23171=CARTESIAN_POINT('',(25.7042973488569,-10.0450204908848,42.));
#23172=CARTESIAN_POINT('',(29.667462259531,2.5,42.));
#23173=CARTESIAN_POINT('',(15.8521486744285,2.5,42.));
#23174=CARTESIAN_POINT('',(29.667462259531,-9.75,42.));
#23175=CARTESIAN_POINT('',(20.4519100487232,-2.14699864387512,42.));
#23176=CARTESIAN_POINT('',(19.9982947669923,-1.05388820171356,42.));
#23177=CARTESIAN_POINT('Ctrl Pts',(20.4519100487232,-2.14699864387512,42.));
#23178=CARTESIAN_POINT('Ctrl Pts',(19.9982947669923,-1.7087310552597,42.));
#23179=CARTESIAN_POINT('Ctrl Pts',(19.9982947669923,-1.05388820171356,42.));
#23180=CARTESIAN_POINT('',(20.2455662563443,-0.237039625644684,42.));
#23181=CARTESIAN_POINT('Ctrl Pts',(19.9982947669923,-1.05388820171356,42.));
#23182=CARTESIAN_POINT('Ctrl Pts',(19.9982947669923,-0.566166639328003,
42.));
#23183=CARTESIAN_POINT('Ctrl Pts',(20.2455662563443,-0.237039625644684,
42.));
#23184=CARTESIAN_POINT('',(20.94986371696,0.211459994316101,42.));
#23185=CARTESIAN_POINT('Ctrl Pts',(20.2455662563443,-0.237039625644684,
42.));
#23186=CARTESIAN_POINT('Ctrl Pts',(20.4928377270699,0.0920873880386353,
42.));
#23187=CARTESIAN_POINT('Ctrl Pts',(20.94986371696,0.211459994316101,42.));
#23188=CARTESIAN_POINT('',(20.3836972266436,0.610504746437073,42.));
#23189=CARTESIAN_POINT('Ctrl Pts',(20.94986371696,0.211459994316101,42.));
#23190=CARTESIAN_POINT('Ctrl Pts',(20.5678718537092,0.351296067237854,42.));
#23191=CARTESIAN_POINT('Ctrl Pts',(20.3836972266436,0.610504746437073,42.));
#23192=CARTESIAN_POINT('',(20.1995225995779,1.23124152421951,42.));
#23193=CARTESIAN_POINT('Ctrl Pts',(20.3836972266436,0.610504746437073,42.));
#23194=CARTESIAN_POINT('Ctrl Pts',(20.1995225995779,0.869713723659515,42.));
#23195=CARTESIAN_POINT('Ctrl Pts',(20.1995225995779,1.23124152421951,42.));
#23196=CARTESIAN_POINT('',(20.5917463451624,2.14870393276215,42.));
#23197=CARTESIAN_POINT('Ctrl Pts',(20.1995225995779,1.23124152421951,42.));
#23198=CARTESIAN_POINT('Ctrl Pts',(20.1995225995779,1.77694410085678,42.));
#23199=CARTESIAN_POINT('Ctrl Pts',(20.5917463451624,2.14870393276215,42.));
#23200=CARTESIAN_POINT('',(21.6354024410248,2.52046346664429,42.));
#23201=CARTESIAN_POINT('Ctrl Pts',(20.5917463451624,2.14870393276215,42.));
#23202=CARTESIAN_POINT('Ctrl Pts',(20.9839700162411,2.52046346664429,42.));
#23203=CARTESIAN_POINT('Ctrl Pts',(21.6354024410248,2.52046346664429,42.));
#23204=CARTESIAN_POINT('',(22.68929079175,2.14017748832703,42.));
#23205=CARTESIAN_POINT('Ctrl Pts',(21.6354024410248,2.52046346664429,42.));
#23206=CARTESIAN_POINT('Ctrl Pts',(22.2902457416058,2.52046346664429,42.));
#23207=CARTESIAN_POINT('Ctrl Pts',(22.68929079175,2.14017748832703,42.));
#23208=CARTESIAN_POINT('',(23.0883358418941,1.21418833732605,42.));
#23209=CARTESIAN_POINT('Ctrl Pts',(22.68929079175,2.14017748832703,42.));
#23210=CARTESIAN_POINT('Ctrl Pts',(23.0883358418941,1.75989091396332,42.));
#23211=CARTESIAN_POINT('Ctrl Pts',(23.0883358418941,1.21418833732605,42.));
#23212=CARTESIAN_POINT('',(22.9058663547039,0.608799457550049,42.));
#23213=CARTESIAN_POINT('Ctrl Pts',(23.0883358418941,1.21418833732605,42.));
#23214=CARTESIAN_POINT('Ctrl Pts',(23.0883358418941,0.866302847862244,42.));
#23215=CARTESIAN_POINT('Ctrl Pts',(22.9058663547039,0.608799457550049,42.));
#23216=CARTESIAN_POINT('',(22.3516373336315,0.211459994316101,42.));
#23217=CARTESIAN_POINT('Ctrl Pts',(22.9058663547039,0.608799457550049,42.));
#23218=CARTESIAN_POINT('Ctrl Pts',(22.7233971655369,0.351296067237854,42.));
#23219=CARTESIAN_POINT('Ctrl Pts',(22.3516373336315,0.211459994316101,42.));
#23220=CARTESIAN_POINT('',(23.0525241792202,-0.272851288318634,42.));
#23221=CARTESIAN_POINT('Ctrl Pts',(22.3516373336315,0.211459994316101,42.));
#23222=CARTESIAN_POINT('Ctrl Pts',(22.8120739758015,0.0613915920257568,
42.));
#23223=CARTESIAN_POINT('Ctrl Pts',(23.0525241792202,-0.272851288318634,
42.));
#23224=CARTESIAN_POINT('',(23.2929743826389,-1.07094138860703,42.));
#23225=CARTESIAN_POINT('Ctrl Pts',(23.0525241792202,-0.272851288318634,
42.));
#23226=CARTESIAN_POINT('Ctrl Pts',(23.2929743826389,-0.607094168663025,
42.));
#23227=CARTESIAN_POINT('Ctrl Pts',(23.2929743826389,-1.07094138860703,42.));
#23228=CARTESIAN_POINT('',(22.8393588960171,-2.14870393276215,42.));
#23229=CARTESIAN_POINT('Ctrl Pts',(23.2929743826389,-1.07094138860703,42.));
#23230=CARTESIAN_POINT('Ctrl Pts',(23.2929743826389,-1.71214163303375,42.));
#23231=CARTESIAN_POINT('Ctrl Pts',(22.8393588960171,-2.14870393276215,42.));
#23232=CARTESIAN_POINT('',(21.6456344723701,-2.58526623249054,42.));
#23233=CARTESIAN_POINT('Ctrl Pts',(22.8393588960171,-2.14870393276215,42.));
#23234=CARTESIAN_POINT('Ctrl Pts',(22.3857437074184,-2.58526623249054,42.));
#23235=CARTESIAN_POINT('Ctrl Pts',(21.6456344723701,-2.58526623249054,42.));
#23236=CARTESIAN_POINT('Ctrl Pts',(21.6456344723701,-2.58526623249054,42.));
#23237=CARTESIAN_POINT('Ctrl Pts',(20.9055253863335,-2.58526623249054,42.));
#23238=CARTESIAN_POINT('Ctrl Pts',(20.4519100487232,-2.14699864387512,42.));
#23239=CARTESIAN_POINT('',(39.0330834686756,-2.5,42.));
#23240=CARTESIAN_POINT('',(36.4068896323442,1.42905861139297,42.));
#23241=CARTESIAN_POINT('',(38.437241915911,-1.60855918115101,42.));
#23242=CARTESIAN_POINT('',(36.4068896323442,-2.5,42.));
#23243=CARTESIAN_POINT('',(36.4068896323442,-10.2854706943035,42.));
#23244=CARTESIAN_POINT('',(35.772510394454,-2.5,42.));
#23245=CARTESIAN_POINT('',(21.2034448161721,-2.5,42.));
#23246=CARTESIAN_POINT('',(35.772510394454,2.5,42.));
#23247=CARTESIAN_POINT('',(35.772510394454,-12.25,42.));
#23248=CARTESIAN_POINT('',(36.4512279629707,2.5,42.));
#23249=CARTESIAN_POINT('',(20.886255197227,2.5,42.));
#23250=CARTESIAN_POINT('',(39.0774215757847,-1.42564833164215,42.));
#23251=CARTESIAN_POINT('',(37.4052567618647,1.07391262226716,42.));
#23252=CARTESIAN_POINT('',(39.0774215757847,2.5,42.));
#23253=CARTESIAN_POINT('',(39.0774215757847,-11.7128241658211,42.));
#23254=CARTESIAN_POINT('',(39.7118009626865,2.5,42.));
#23255=CARTESIAN_POINT('',(22.5387107878923,2.5,42.));
#23256=CARTESIAN_POINT('',(39.7118009626865,-2.5,42.));
#23257=CARTESIAN_POINT('',(39.7118009626865,-9.75,42.));
#23258=CARTESIAN_POINT('',(22.8559004813433,-2.5,42.));
#23259=CARTESIAN_POINT('Origin',(0.,-22.,36.));
#23260=CARTESIAN_POINT('',(3.625,-20.5,39.625));
#23261=CARTESIAN_POINT('Origin',(4.68566017177982,-20.5,38.5643398282202));
#23262=CARTESIAN_POINT('Origin',(1.5,-20.5,-6.25));
#23263=CARTESIAN_POINT('Origin',(13.5,-20.5,-10.75));
#23264=CARTESIAN_POINT('',(15.,-20.5,18.));
#23265=CARTESIAN_POINT('',(15.,-20.5,-10.75));
#23266=CARTESIAN_POINT('Origin',(13.5,-20.5,18.));
#23267=CARTESIAN_POINT('Origin',(70.,-22.,-25.));
#23268=CARTESIAN_POINT('',(13.5,-22.,-25.));
#23269=CARTESIAN_POINT('Origin',(13.5,-22.,-23.5));
#23270=CARTESIAN_POINT('',(15.,-22.,-23.5));
#23271=CARTESIAN_POINT('Origin',(13.5,20.5,-10.75));
#23272=CARTESIAN_POINT('',(13.5,22.,18.));
#23273=CARTESIAN_POINT('',(13.5,22.,-10.75));
#23274=CARTESIAN_POINT('',(15.,20.5,18.));
#23275=CARTESIAN_POINT('Origin',(13.5,20.5,18.));
#23276=CARTESIAN_POINT('',(15.,20.5,-10.75));
#23277=CARTESIAN_POINT('Origin',(24.,-20.5,40.5));
#23278=CARTESIAN_POINT('Origin',(82.5,-20.5,15.25));
#23279=CARTESIAN_POINT('',(84.,-20.5,17.5712833908056));
#23280=CARTESIAN_POINT('Ctrl Pts',(84.,-20.5,17.5712833908056));
#23281=CARTESIAN_POINT('Ctrl Pts',(84.,-20.7022477383282,17.3353257465337));
#23282=CARTESIAN_POINT('Ctrl Pts',(83.9575260447373,-20.9170846786411,17.0756837501162));
#23283=CARTESIAN_POINT('Ctrl Pts',(83.7765132729403,-21.3178359703858,16.572666547787));
#23284=CARTESIAN_POINT('Ctrl Pts',(83.6391148171733,-21.5040391092436,16.3291117577357));
#23285=CARTESIAN_POINT('Ctrl Pts',(83.3468785813891,-21.7463710185311,16.0037159774975));
#23286=CARTESIAN_POINT('Ctrl Pts',(83.2051881089356,-21.8355590404292,15.88144036437));
#23287=CARTESIAN_POINT('Ctrl Pts',(82.9588244922017,-21.9308152339295,15.7493583883479));
#23288=CARTESIAN_POINT('Ctrl Pts',(82.8710686191993,-21.9563375109926,15.7136914161295));
#23289=CARTESIAN_POINT('Ctrl Pts',(82.6889643978921,-21.9909261474626,15.665250854624));
#23290=CARTESIAN_POINT('Ctrl Pts',(82.5946178513886,-22.,15.6524758424985));
#23291=CARTESIAN_POINT('Ctrl Pts',(82.5,-22.,15.6524758424985));
#23292=CARTESIAN_POINT('',(84.,-20.5,15.25));
#23293=CARTESIAN_POINT('Origin',(84.,-22.,22.));
#23294=CARTESIAN_POINT('Origin',(84.,0.,0.));
#23295=CARTESIAN_POINT('Origin',(70.,-22.,0.));
#23296=CARTESIAN_POINT('Origin',(70.,0.,0.));
#23297=CARTESIAN_POINT('Origin',(61.5,-20.5,14.75));
#23298=CARTESIAN_POINT('',(61.5,-22.,-15.6524758424985));
#23299=CARTESIAN_POINT('',(61.5,-22.,14.75));
#23300=CARTESIAN_POINT('Ctrl Pts',(60.,-20.5,-15.1657508881031));
#23301=CARTESIAN_POINT('Ctrl Pts',(60.,-20.5020625379506,-15.1664308867282));
#23302=CARTESIAN_POINT('Ctrl Pts',(60.0000042540628,-20.5041250881598,-15.1671108436611));
#23303=CARTESIAN_POINT('Ctrl Pts',(60.000459532602,-20.6144922519149,-15.2034929264267));
#23304=CARTESIAN_POINT('Ctrl Pts',(60.0126356314555,-20.7225920605635,-15.2390001138621));
#23305=CARTESIAN_POINT('Ctrl Pts',(60.0601510385376,-20.9342353436599,-15.3082836950208));
#23306=CARTESIAN_POINT('Ctrl Pts',(60.0953241933879,-21.0373769241961,-15.3419294911594));
#23307=CARTESIAN_POINT('Ctrl Pts',(60.2231667795538,-21.310385626032,-15.4307183360865));
#23308=CARTESIAN_POINT('Ctrl Pts',(60.3382746523712,-21.4688874023992,-15.4819477371951));
#23309=CARTESIAN_POINT('Ctrl Pts',(60.6191603261817,-21.7283867354349,-15.5655237678324));
#23310=CARTESIAN_POINT('Ctrl Pts',(60.7797547588616,-21.8293573646189,-15.5978863073161));
#23311=CARTESIAN_POINT('Ctrl Pts',(61.129199035605,-21.9652152818212,-15.6413750983628));
#23312=CARTESIAN_POINT('Ctrl Pts',(61.3134705059138,-22.,-15.6524758424985));
#23313=CARTESIAN_POINT('Ctrl Pts',(61.5,-22.,-15.6524758424985));
#23314=CARTESIAN_POINT('Origin',(61.5,-22.,-23.5));
#23315=CARTESIAN_POINT('Ctrl Pts',(61.5,-10.1980390271856,-25.));
#23316=CARTESIAN_POINT('Ctrl Pts',(61.3081176819558,-10.1980390271856,-25.));
#23317=CARTESIAN_POINT('Ctrl Pts',(61.1182675528468,-10.1908261217545,-24.9631850847576));
#23318=CARTESIAN_POINT('Ctrl Pts',(60.7614154879323,-10.1626433260876,-24.8197797335775));
#23319=CARTESIAN_POINT('Ctrl Pts',(60.5983542509472,-10.1418364073688,-24.7140382945063));
#23320=CARTESIAN_POINT('Ctrl Pts',(60.3189691603886,-10.0886902105648,-24.4452375771159));
#23321=CARTESIAN_POINT('Ctrl Pts',(60.2063475813541,-10.0566512843893,-24.283743850747));
#23322=CARTESIAN_POINT('Ctrl Pts',(60.0861774650203,-10.0023374403617,-24.0115999983853));
#23323=CARTESIAN_POINT('Ctrl Pts',(60.054419379683,-9.98267886135603,-23.9133673884351));
#23324=CARTESIAN_POINT('Ctrl Pts',(60.0114978161663,-9.94226557571909,-23.7120589639788));
#23325=CARTESIAN_POINT('Ctrl Pts',(60.0004641001801,-9.92160226317557,-23.6094398880042));
#23326=CARTESIAN_POINT('Ctrl Pts',(60.0000047777623,-9.90037810810563,-23.504371622114));
#23327=CARTESIAN_POINT('Ctrl Pts',(60.,-9.8999365367755,-23.5021858092929));
#23328=CARTESIAN_POINT('Ctrl Pts',(60.,-9.89949493661168,-23.5));
#23329=CARTESIAN_POINT('Origin',(42.,-22.,8.5));
#23330=CARTESIAN_POINT('',(75.5,-22.,-15.6524758424985));
#23331=CARTESIAN_POINT('Origin',(61.5,20.5,-23.5));
#23332=CARTESIAN_POINT('',(61.5,20.5,-25.));
#23333=CARTESIAN_POINT('',(61.5,22.,-23.5));
#23334=CARTESIAN_POINT('Origin',(61.5,20.5,-23.5));
#23335=CARTESIAN_POINT('Origin',(61.5,20.5,-23.5));
#23336=CARTESIAN_POINT('Origin',(61.5,20.5,-23.5));
#23337=CARTESIAN_POINT('Origin',(61.5,-22.,-23.5));
#23338=CARTESIAN_POINT('',(61.5,10.1980390271856,-25.));
#23339=CARTESIAN_POINT('Ctrl Pts',(60.,9.89949493661168,-23.5));
#23340=CARTESIAN_POINT('Ctrl Pts',(60.,9.89993832731204,-23.5021946719966));
#23341=CARTESIAN_POINT('Ctrl Pts',(60.0000048165852,9.90038168894123,-23.5043893475508));
#23342=CARTESIAN_POINT('Ctrl Pts',(60.0004660319782,9.92160723858752,-23.6094645739685));
#23343=CARTESIAN_POINT('Ctrl Pts',(60.0115011689912,9.94227012456818,-23.7120815813529));
#23344=CARTESIAN_POINT('Ctrl Pts',(60.0544249797747,9.98268274401981,-23.9133867704278));
#23345=CARTESIAN_POINT('Ctrl Pts',(60.0861841059616,10.0023410769715,-24.0116181880972));
#23346=CARTESIAN_POINT('Ctrl Pts',(60.206355943955,10.0566538664141,-24.2837568481804));
#23347=CARTESIAN_POINT('Ctrl Pts',(60.3189770792875,10.0886920356348,-24.4452467916769));
#23348=CARTESIAN_POINT('Ctrl Pts',(60.5983596493521,10.1418371216814,-24.7140419232243));
#23349=CARTESIAN_POINT('Ctrl Pts',(60.7614191687488,10.1626436608923,-24.819781436362));
#23350=CARTESIAN_POINT('Ctrl Pts',(61.1182686232222,10.1908261625926,-24.9631852933862));
#23351=CARTESIAN_POINT('Ctrl Pts',(61.3081182257788,10.1980390271856,-25.));
#23352=CARTESIAN_POINT('Ctrl Pts',(61.5,10.1980390271856,-25.));
#23353=CARTESIAN_POINT('',(61.5,-22.,-25.));
#23354=CARTESIAN_POINT('Origin',(61.5,20.5,14.75));
#23355=CARTESIAN_POINT('',(61.5,22.,-15.6524758424985));
#23356=CARTESIAN_POINT('Ctrl Pts',(61.5,22.,-15.6524758424985));
#23357=CARTESIAN_POINT('Ctrl Pts',(61.3134858239941,22.,-15.6524758424985));
#23358=CARTESIAN_POINT('Ctrl Pts',(61.1292291179574,21.9652209916066,-15.6413769188859));
#23359=CARTESIAN_POINT('Ctrl Pts',(60.7798600570244,21.8294044226054,-15.5979013781792));
#23360=CARTESIAN_POINT('Ctrl Pts',(60.619315251053,21.7284875323288,-15.5655560876705));
#23361=CARTESIAN_POINT('Ctrl Pts',(60.3385094668615,21.4691487038552,-15.482032043976));
#23362=CARTESIAN_POINT('Ctrl Pts',(60.2234187980134,21.3107595052867,-15.4308393408124));
#23363=CARTESIAN_POINT('Ctrl Pts',(60.0954774955618,21.0377971691356,-15.3420664979276));
#23364=CARTESIAN_POINT('Ctrl Pts',(60.0602457537108,20.9345730436471,-15.3083940597981));
#23365=CARTESIAN_POINT('Ctrl Pts',(60.0126604270431,20.7227867271798,-15.239064024796));
#23366=CARTESIAN_POINT('Ctrl Pts',(60.0004657094814,20.6146288648013,-15.2035378999918));
#23367=CARTESIAN_POINT('Ctrl Pts',(60.0000043615329,20.5041768692451,-15.1671279142233));
#23368=CARTESIAN_POINT('Ctrl Pts',(60.,20.502088428345,-15.1664394225385));
#23369=CARTESIAN_POINT('Ctrl Pts',(60.,20.5,-15.1657508881031));
#23370=CARTESIAN_POINT('',(61.5,22.,14.75));
#23371=CARTESIAN_POINT('Origin',(68.5,20.5,-23.5));
#23372=CARTESIAN_POINT('',(68.5,20.5,-25.));
#23373=CARTESIAN_POINT('',(68.5,22.,-23.5));
#23374=CARTESIAN_POINT('Origin',(68.5,20.5,-23.5));
#23375=CARTESIAN_POINT('',(70.,20.5,-23.5));
#23376=CARTESIAN_POINT('Origin',(68.5,20.5,-23.5));
#23377=CARTESIAN_POINT('Origin',(68.5,20.5,-23.5));
#23378=CARTESIAN_POINT('Origin',(56.,20.5,-23.5));
#23379=CARTESIAN_POINT('',(56.,20.5,-25.));
#23380=CARTESIAN_POINT('',(56.,22.,-23.5));
#23381=CARTESIAN_POINT('Origin',(70.,-22.,-25.));
#23382=CARTESIAN_POINT('',(68.5,10.1980390271856,-25.));
#23383=CARTESIAN_POINT('',(68.5,-22.,-25.));
#23384=CARTESIAN_POINT('',(75.5,10.1980390271856,-25.));
#23385=CARTESIAN_POINT('Origin',(68.5,-22.,-23.5));
#23386=CARTESIAN_POINT('',(70.,13.2947358003083,-23.5));
#23387=CARTESIAN_POINT('',(70.,-22.,-23.5));
#23388=CARTESIAN_POINT('Ctrl Pts',(68.5,10.1980390271856,-25.));
#23389=CARTESIAN_POINT('Ctrl Pts',(68.5690622745619,10.1980390271856,-25.));
#23390=CARTESIAN_POINT('Ctrl Pts',(68.64269539724,10.2107026186997,-24.9948442089972));
#23391=CARTESIAN_POINT('Ctrl Pts',(68.7815873963742,10.2591413018302,-24.97500159694));
#23392=CARTESIAN_POINT('Ctrl Pts',(68.8470061948633,10.2945164376804,-24.9604604345961));
#23393=CARTESIAN_POINT('Ctrl Pts',(69.099996626182,10.4648018594106,-24.889928820497));
#23394=CARTESIAN_POINT('Ctrl Pts',(69.2682778073745,10.6853817343331,-24.7965377420129));
#23395=CARTESIAN_POINT('Ctrl Pts',(69.8122976763679,11.5896482415098,-24.3983540225569));
#23396=CARTESIAN_POINT('Ctrl Pts',(70.,12.5253526611459,-23.9352657686969));
#23397=CARTESIAN_POINT('Ctrl Pts',(70.,13.2947358003083,-23.5));
#23398=CARTESIAN_POINT('Origin',(68.5,20.5,4.25));
#23399=CARTESIAN_POINT('',(68.5,22.,-15.6524758424985));
#23400=CARTESIAN_POINT('',(68.5,22.,4.25));
#23401=CARTESIAN_POINT('',(70.,20.5,-17.5712833908056));
#23402=CARTESIAN_POINT('Ctrl Pts',(70.,20.5,-17.5712833908056));
#23403=CARTESIAN_POINT('Ctrl Pts',(70.,20.7022477383282,-17.3353257465337));
#23404=CARTESIAN_POINT('Ctrl Pts',(69.9575260447372,20.9170846786411,-17.0756837501162));
#23405=CARTESIAN_POINT('Ctrl Pts',(69.7765132729404,21.3178359703858,-16.572666547787));
#23406=CARTESIAN_POINT('Ctrl Pts',(69.6391148171733,21.5040391092436,-16.3291117577357));
#23407=CARTESIAN_POINT('Ctrl Pts',(69.3468785813891,21.7463710185311,-16.0037159774975));
#23408=CARTESIAN_POINT('Ctrl Pts',(69.2051881089356,21.8355590404292,-15.88144036437));
#23409=CARTESIAN_POINT('Ctrl Pts',(68.9588244922017,21.9308152339295,-15.7493583883479));
#23410=CARTESIAN_POINT('Ctrl Pts',(68.8710686191993,21.9563375109926,-15.7136914161295));
#23411=CARTESIAN_POINT('Ctrl Pts',(68.6889643978921,21.9909261474626,-15.665250854624));
#23412=CARTESIAN_POINT('Ctrl Pts',(68.5946178513885,22.,-15.6524758424985));
#23413=CARTESIAN_POINT('Ctrl Pts',(68.5,22.,-15.6524758424985));
#23414=CARTESIAN_POINT('',(70.,20.5,4.25));
#23415=CARTESIAN_POINT('Origin',(70.,-22.,0.));
#23416=CARTESIAN_POINT('Origin',(70.,0.,0.));
#23417=CARTESIAN_POINT('Origin',(90.5,0.,0.));
#23418=CARTESIAN_POINT('',(92.,-3.10799188078457E-15,25.3786796564404));
#23419=CARTESIAN_POINT('Origin',(92.,0.,0.));
#23420=CARTESIAN_POINT('',(91.5606601717798,-3.2378852892199E-15,26.4393398282202));
#23421=CARTESIAN_POINT('Origin',(90.5,-3.10799188078457E-15,25.3786796564404));
#23422=CARTESIAN_POINT('',(91.5606601717798,-26.4393398282202,-3.2378852892199E-15));
#23423=CARTESIAN_POINT('Origin',(91.5606601717798,0.,-4.04735661152487E-15));
#23424=CARTESIAN_POINT('Origin',(91.5606601717798,0.,-4.04735661152487E-15));
#23425=CARTESIAN_POINT('Origin',(91.5,0.,0.));
#23426=CARTESIAN_POINT('',(91.4393398282202,-26.5606601717798,-3.25274274626107E-15));
#23427=CARTESIAN_POINT('',(91.5,-26.5,-3.24531401774049E-15));
#23428=CARTESIAN_POINT('',(91.4393398282202,-3.25274274626107E-15,26.5606601717798));
#23429=CARTESIAN_POINT('Origin',(91.4393398282202,0.,-4.06592843282634E-15));
#23430=CARTESIAN_POINT('Origin',(91.4393398282202,0.,-4.06592843282634E-15));
#23431=CARTESIAN_POINT('Origin',(92.,0.,0.));
#23432=CARTESIAN_POINT('',(92.,-21.905,2.68258881353228E-15));
#23433=CARTESIAN_POINT('Origin',(92.,0.,0.));
#23434=CARTESIAN_POINT('Origin',(90.3786796564403,0.,0.));
#23435=CARTESIAN_POINT('',(90.3786796564403,-3.30654635769785E-15,27.));
#23436=CARTESIAN_POINT('Origin',(90.3786796564403,-3.12284933782575E-15,
25.5));
#23437=CARTESIAN_POINT('',(90.3786796564403,-27.,-3.30654635769785E-15));
#23438=CARTESIAN_POINT('Origin',(90.3786796564403,0.,0.));
#23439=CARTESIAN_POINT('Origin',(90.3786796564403,0.,0.));
#23440=CARTESIAN_POINT('Origin',(75.5,0.,0.));
#23441=CARTESIAN_POINT('',(61.5,-27.,-3.30654635769785E-15));
#23442=CARTESIAN_POINT('',(75.5,-27.,-3.30654635769785E-15));
#23443=CARTESIAN_POINT('Origin',(61.5,0.,0.));
#23444=CARTESIAN_POINT('Origin',(61.5,0.,0.));
#23445=CARTESIAN_POINT('',(75.5,22.,-15.6524758424985));
#23446=CARTESIAN_POINT('',(61.5,22.,15.6524758424985));
#23447=CARTESIAN_POINT('Origin',(61.5,0.,0.));
#23448=CARTESIAN_POINT('',(75.5,22.,15.6524758424985));
#23449=CARTESIAN_POINT('Origin',(84.,0.,0.));
#23450=CARTESIAN_POINT('Origin',(61.5,0.,0.));
#23451=CARTESIAN_POINT('Origin',(61.5,0.,0.));
#23452=CARTESIAN_POINT('Origin',(28.5,20.5,22.5));
#23453=CARTESIAN_POINT('',(57.,22.,22.5));
#23454=CARTESIAN_POINT('',(57.,20.5,21.));
#23455=CARTESIAN_POINT('Origin',(57.,20.5,22.5));
#23456=CARTESIAN_POINT('',(18.,20.5,21.));
#23457=CARTESIAN_POINT('',(28.5,20.5,21.));
#23458=CARTESIAN_POINT('',(18.,22.,22.5));
#23459=CARTESIAN_POINT('Origin',(18.,20.5,22.5));
#23460=CARTESIAN_POINT('',(28.5,22.,22.5));
#23461=CARTESIAN_POINT('Origin',(18.,20.5,18.));
#23462=CARTESIAN_POINT('Origin',(18.,22.,18.));
#23463=CARTESIAN_POINT('Origin',(18.,20.5,18.));
#23464=CARTESIAN_POINT('Origin',(28.5,-20.5,22.5));
#23465=CARTESIAN_POINT('',(18.,-20.5,21.));
#23466=CARTESIAN_POINT('Origin',(18.,-20.5,22.5));
#23467=CARTESIAN_POINT('',(57.,-20.5,21.));
#23468=CARTESIAN_POINT('',(28.5,-20.5,21.));
#23469=CARTESIAN_POINT('Origin',(57.,-20.5,22.5));
#23470=CARTESIAN_POINT('Origin',(57.,-20.5,18.));
#23471=CARTESIAN_POINT('Origin',(61.5,-20.5,18.));
#23472=CARTESIAN_POINT('Origin',(57.,-20.5,18.));
#23473=CARTESIAN_POINT('Origin',(61.5,-20.5,14.75));
#23474=CARTESIAN_POINT('Ctrl Pts',(60.,-20.5,15.1657508881031));
#23475=CARTESIAN_POINT('Ctrl Pts',(60.,-20.5018310939024,15.1663545818852));
#23476=CARTESIAN_POINT('Ctrl Pts',(60.0000033529049,-20.5036621975828,15.1669582428458));
#23477=CARTESIAN_POINT('Ctrl Pts',(60.0004057833521,-20.6135490452472,15.2031825380108));
#23478=CARTESIAN_POINT('Ctrl Pts',(60.0124770444123,-20.7214063029217,15.2386108915177));
#23479=CARTESIAN_POINT('Ctrl Pts',(60.0596389516904,-20.9324251256081,15.3076921352536));
#23480=CARTESIAN_POINT('Ctrl Pts',(60.0945262837795,-21.0351965386236,15.3412186660997));
#23481=CARTESIAN_POINT('Ctrl Pts',(60.2218896363614,-21.3084881625076,15.430104219162));
#23482=CARTESIAN_POINT('Ctrl Pts',(60.3370862252174,-21.4675640567846,15.4815207668313));
#23483=CARTESIAN_POINT('Ctrl Pts',(60.6183791948953,-21.7278782657557,15.5653607304813));
#23484=CARTESIAN_POINT('Ctrl Pts',(60.7792244100121,-21.8291204213603,15.5978104235522));
#23485=CARTESIAN_POINT('Ctrl Pts',(61.1290483151644,-21.9651866670112,15.6413659747481));
#23486=CARTESIAN_POINT('Ctrl Pts',(61.3133937576427,-22.,15.6524758424985));
#23487=CARTESIAN_POINT('Ctrl Pts',(61.5,-22.,15.6524758424985));
#23488=CARTESIAN_POINT('Origin',(18.,-20.5,18.));
#23489=CARTESIAN_POINT('Origin',(18.,-20.5,18.));
#23490=CARTESIAN_POINT('Origin',(61.5,0.,0.));
#23491=CARTESIAN_POINT('Origin',(57.,20.5,18.));
#23492=CARTESIAN_POINT('',(61.5,22.,18.));
#23493=CARTESIAN_POINT('Origin',(61.5,20.5,18.));
#23494=CARTESIAN_POINT('Origin',(57.,20.5,18.));
#23495=CARTESIAN_POINT('Origin',(57.,22.,18.));
#23496=CARTESIAN_POINT('Origin',(61.5,20.5,14.75));
#23497=CARTESIAN_POINT('',(61.5,22.,14.75));
#23498=CARTESIAN_POINT('Ctrl Pts',(61.5,22.,15.6524758424985));
#23499=CARTESIAN_POINT('Ctrl Pts',(61.3133937576427,22.,15.6524758424985));
#23500=CARTESIAN_POINT('Ctrl Pts',(61.1290483151644,21.9651866670112,15.6413659747481));
#23501=CARTESIAN_POINT('Ctrl Pts',(60.7792244100121,21.8291204213603,15.5978104235522));
#23502=CARTESIAN_POINT('Ctrl Pts',(60.6183791948954,21.7278782657557,15.5653607304813));
#23503=CARTESIAN_POINT('Ctrl Pts',(60.3370862252174,21.4675640567846,15.4815207668312));
#23504=CARTESIAN_POINT('Ctrl Pts',(60.2218896363614,21.3084881625076,15.430104219162));
#23505=CARTESIAN_POINT('Ctrl Pts',(60.0945262837793,21.0351965386233,15.3412186660996));
#23506=CARTESIAN_POINT('Ctrl Pts',(60.0596389516902,20.9324251256073,15.3076921352533));
#23507=CARTESIAN_POINT('Ctrl Pts',(60.0124770444122,20.7214063029204,15.2386108915173));
#23508=CARTESIAN_POINT('Ctrl Pts',(60.0004057833519,20.613549045247,15.2031825380104));
#23509=CARTESIAN_POINT('Ctrl Pts',(60.0000033529049,20.5036621975811,15.1669582428453));
#23510=CARTESIAN_POINT('Ctrl Pts',(60.,20.5018310939017,15.166354581885));
#23511=CARTESIAN_POINT('Ctrl Pts',(60.,20.5,15.1657508881031));
#23512=CARTESIAN_POINT('Origin',(61.5,0.,0.));
#23513=CARTESIAN_POINT('Origin',(15.,-22.,-30.));
#23514=CARTESIAN_POINT('',(15.,-22.,18.));
#23515=CARTESIAN_POINT('',(15.,-3.73517273739943E-16,3.05));
#23516=CARTESIAN_POINT('Origin',(15.,0.,0.));
#23517=CARTESIAN_POINT('Origin',(18.,-22.,18.));
#23518=CARTESIAN_POINT('',(18.,-22.,21.));
#23519=CARTESIAN_POINT('Origin',(15.,-22.,21.));
#23520=CARTESIAN_POINT('',(57.,-22.,21.));
#23521=CARTESIAN_POINT('Origin',(57.,-22.,18.));
#23522=CARTESIAN_POINT('Ctrl Pts',(32.5358115136623,-2.58526623249054,42.));
#23523=CARTESIAN_POINT('Ctrl Pts',(32.5358115136623,-2.58526623249054,41.7));
#23524=CARTESIAN_POINT('Ctrl Pts',(31.8298088014126,-2.58526623249054,42.));
#23525=CARTESIAN_POINT('Ctrl Pts',(31.8298088014126,-2.58526623249054,41.7));
#23526=CARTESIAN_POINT('Ctrl Pts',(31.2738743424416,-2.24420189857483,42.));
#23527=CARTESIAN_POINT('Ctrl Pts',(31.2738743424416,-2.24420189857483,41.7));
#23528=CARTESIAN_POINT('',(32.5358115136623,-2.58526623249054,41.7));
#23529=CARTESIAN_POINT('',(32.5358115136623,-2.58526623249054,42.));
#23530=CARTESIAN_POINT('',(31.2738743424416,-2.24420189857483,41.7));
#23531=CARTESIAN_POINT('Ctrl Pts',(32.5358115136623,-2.58526623249054,41.7));
#23532=CARTESIAN_POINT('Ctrl Pts',(31.8298088014126,-2.58526623249054,41.7));
#23533=CARTESIAN_POINT('Ctrl Pts',(31.2738743424416,-2.24420189857483,41.7));
#23534=CARTESIAN_POINT('',(31.2738743424416,-2.24420189857483,42.));
#23535=CARTESIAN_POINT('Ctrl Pts',(33.7499998509884,-2.27660298347473,42.));
#23536=CARTESIAN_POINT('Ctrl Pts',(33.7499998509884,-2.27660298347473,41.7));
#23537=CARTESIAN_POINT('Ctrl Pts',(33.1872440874577,-2.58526623249054,42.));
#23538=CARTESIAN_POINT('Ctrl Pts',(33.1872440874577,-2.58526623249054,41.7));
#23539=CARTESIAN_POINT('Ctrl Pts',(32.5358115136623,-2.58526623249054,42.));
#23540=CARTESIAN_POINT('Ctrl Pts',(32.5358115136623,-2.58526623249054,41.7));
#23541=CARTESIAN_POINT('',(33.7499998509884,-2.27660298347473,41.7));
#23542=CARTESIAN_POINT('',(33.7499998509884,-2.27660298347473,42.));
#23543=CARTESIAN_POINT('Ctrl Pts',(33.7499998509884,-2.27660298347473,41.7));
#23544=CARTESIAN_POINT('Ctrl Pts',(33.1872440874577,-2.58526623249054,41.7));
#23545=CARTESIAN_POINT('Ctrl Pts',(32.5358115136623,-2.58526623249054,41.7));
#23546=CARTESIAN_POINT('Ctrl Pts',(34.6197132766247,-1.36766731739044,42.));
#23547=CARTESIAN_POINT('Ctrl Pts',(34.6197132766247,-1.36766731739044,41.7));
#23548=CARTESIAN_POINT('Ctrl Pts',(34.3127556145191,-1.96793973445892,42.));
#23549=CARTESIAN_POINT('Ctrl Pts',(34.3127556145191,-1.96793973445892,41.7));
#23550=CARTESIAN_POINT('Ctrl Pts',(33.7499998509884,-2.27660298347473,42.));
#23551=CARTESIAN_POINT('Ctrl Pts',(33.7499998509884,-2.27660298347473,41.7));
#23552=CARTESIAN_POINT('',(34.6197132766247,-1.36766731739044,41.7));
#23553=CARTESIAN_POINT('',(34.6197132766247,-1.36766731739044,42.));
#23554=CARTESIAN_POINT('Ctrl Pts',(34.6197132766247,-1.36766731739044,41.7));
#23555=CARTESIAN_POINT('Ctrl Pts',(34.3127556145191,-1.96793973445892,41.7));
#23556=CARTESIAN_POINT('Ctrl Pts',(33.7499998509884,-2.27660298347473,41.7));
#23557=CARTESIAN_POINT('Ctrl Pts',(34.9266712367535,-0.00682175159454346,
42.));
#23558=CARTESIAN_POINT('Ctrl Pts',(34.9266712367535,-0.00682175159454346,
41.7));
#23559=CARTESIAN_POINT('Ctrl Pts',(34.9266712367535,-0.767394304275513,
42.));
#23560=CARTESIAN_POINT('Ctrl Pts',(34.9266712367535,-0.767394304275513,
41.7));
#23561=CARTESIAN_POINT('Ctrl Pts',(34.6197132766247,-1.36766731739044,42.));
#23562=CARTESIAN_POINT('Ctrl Pts',(34.6197132766247,-1.36766731739044,41.7));
#23563=CARTESIAN_POINT('',(34.9266712367535,-0.00682175159454346,41.7));
#23564=CARTESIAN_POINT('',(34.9266712367535,-0.00682175159454346,42.));
#23565=CARTESIAN_POINT('Ctrl Pts',(34.9266712367535,-0.00682175159454346,
41.7));
#23566=CARTESIAN_POINT('Ctrl Pts',(34.9266712367535,-0.767394304275513,
41.7));
#23567=CARTESIAN_POINT('Ctrl Pts',(34.6197132766247,-1.36766731739044,41.7));
#23568=CARTESIAN_POINT('Ctrl Pts',(34.6350611746311,1.33526593446732,42.));
#23569=CARTESIAN_POINT('Ctrl Pts',(34.6350611746311,1.33526593446732,41.7));
#23570=CARTESIAN_POINT('Ctrl Pts',(34.9266712367535,0.74351966381073,42.));
#23571=CARTESIAN_POINT('Ctrl Pts',(34.9266712367535,0.74351966381073,41.7));
#23572=CARTESIAN_POINT('Ctrl Pts',(34.9266712367535,-0.00682175159454346,
42.));
#23573=CARTESIAN_POINT('Ctrl Pts',(34.9266712367535,-0.00682175159454346,
41.7));
#23574=CARTESIAN_POINT('',(34.6350611746311,1.33526593446732,41.7));
#23575=CARTESIAN_POINT('',(34.6350611746311,1.33526593446732,42.));
#23576=CARTESIAN_POINT('Ctrl Pts',(34.6350611746311,1.33526593446732,41.7));
#23577=CARTESIAN_POINT('Ctrl Pts',(34.9266712367535,0.74351966381073,41.7));
#23578=CARTESIAN_POINT('Ctrl Pts',(34.9266712367535,-0.00682175159454346,
41.7));
#23579=CARTESIAN_POINT('Ctrl Pts',(33.7875168025494,2.25784420967102,42.));
#23580=CARTESIAN_POINT('Ctrl Pts',(33.7875168025494,2.25784420967102,41.7));
#23581=CARTESIAN_POINT('Ctrl Pts',(34.343451410532,1.92701190710068,42.));
#23582=CARTESIAN_POINT('Ctrl Pts',(34.343451410532,1.92701190710068,41.7));
#23583=CARTESIAN_POINT('Ctrl Pts',(34.6350611746311,1.33526593446732,42.));
#23584=CARTESIAN_POINT('Ctrl Pts',(34.6350611746311,1.33526593446732,41.7));
#23585=CARTESIAN_POINT('',(33.7875168025494,2.25784420967102,41.7));
#23586=CARTESIAN_POINT('',(33.7875168025494,2.25784420967102,42.));
#23587=CARTESIAN_POINT('Ctrl Pts',(33.7875168025494,2.25784420967102,41.7));
#23588=CARTESIAN_POINT('Ctrl Pts',(34.343451410532,1.92701190710068,41.7));
#23589=CARTESIAN_POINT('Ctrl Pts',(34.6350611746311,1.33526593446732,41.7));
#23590=CARTESIAN_POINT('Ctrl Pts',(32.5392223894596,2.58867621421814,42.));
#23591=CARTESIAN_POINT('Ctrl Pts',(32.5392223894596,2.58867621421814,41.7));
#23592=CARTESIAN_POINT('Ctrl Pts',(33.23158249259,2.58867621421814,42.));
#23593=CARTESIAN_POINT('Ctrl Pts',(33.23158249259,2.58867621421814,41.7));
#23594=CARTESIAN_POINT('Ctrl Pts',(33.7875168025494,2.25784420967102,42.));
#23595=CARTESIAN_POINT('Ctrl Pts',(33.7875168025494,2.25784420967102,41.7));
#23596=CARTESIAN_POINT('',(32.5392223894596,2.58867621421814,41.7));
#23597=CARTESIAN_POINT('',(32.5392223894596,2.58867621421814,42.));
#23598=CARTESIAN_POINT('Ctrl Pts',(32.5392223894596,2.58867621421814,41.7));
#23599=CARTESIAN_POINT('Ctrl Pts',(33.23158249259,2.58867621421814,41.7));
#23600=CARTESIAN_POINT('Ctrl Pts',(33.7875168025494,2.25784420967102,41.7));
#23601=CARTESIAN_POINT('Ctrl Pts',(30.8134378492832,1.88437908887863,42.));
#23602=CARTESIAN_POINT('Ctrl Pts',(30.8134378492832,1.88437908887863,41.7));
#23603=CARTESIAN_POINT('Ctrl Pts',(31.4819234609604,2.58867621421814,42.));
#23604=CARTESIAN_POINT('Ctrl Pts',(31.4819234609604,2.58867621421814,41.7));
#23605=CARTESIAN_POINT('Ctrl Pts',(32.5392223894596,2.58867621421814,42.));
#23606=CARTESIAN_POINT('Ctrl Pts',(32.5392223894596,2.58867621421814,41.7));
#23607=CARTESIAN_POINT('',(30.8134378492832,1.88437908887863,41.7));
#23608=CARTESIAN_POINT('',(30.8134378492832,1.88437908887863,42.));
#23609=CARTESIAN_POINT('Ctrl Pts',(30.8134378492832,1.88437908887863,41.7));
#23610=CARTESIAN_POINT('Ctrl Pts',(31.4819234609604,2.58867621421814,41.7));
#23611=CARTESIAN_POINT('Ctrl Pts',(32.5392223894596,2.58867621421814,41.7));
#23612=CARTESIAN_POINT('Ctrl Pts',(30.1449521258473,-0.0648021697998047,
42.));
#23613=CARTESIAN_POINT('Ctrl Pts',(30.1449521258473,-0.0648021697998047,
41.7));
#23614=CARTESIAN_POINT('Ctrl Pts',(30.1449521258473,1.1800816655159,42.));
#23615=CARTESIAN_POINT('Ctrl Pts',(30.1449521258473,1.1800816655159,41.7));
#23616=CARTESIAN_POINT('Ctrl Pts',(30.8134378492832,1.88437908887863,42.));
#23617=CARTESIAN_POINT('Ctrl Pts',(30.8134378492832,1.88437908887863,41.7));
#23618=CARTESIAN_POINT('',(30.1449521258473,-0.0648021697998047,41.7));
#23619=CARTESIAN_POINT('',(30.1449521258473,-0.0648021697998047,42.));
#23620=CARTESIAN_POINT('Ctrl Pts',(30.1449521258473,-0.0648021697998047,
41.7));
#23621=CARTESIAN_POINT('Ctrl Pts',(30.1449521258473,1.1800816655159,41.7));
#23622=CARTESIAN_POINT('Ctrl Pts',(30.8134378492832,1.88437908887863,41.7));
#23623=CARTESIAN_POINT('Ctrl Pts',(30.4314459860325,-1.31309688091278,42.));
#23624=CARTESIAN_POINT('Ctrl Pts',(30.4314459860325,-1.31309688091278,41.7));
#23625=CARTESIAN_POINT('Ctrl Pts',(30.1449521258473,-0.723056197166443,
42.));
#23626=CARTESIAN_POINT('Ctrl Pts',(30.1449521258473,-0.723056197166443,
41.7));
#23627=CARTESIAN_POINT('Ctrl Pts',(30.1449521258473,-0.0648021697998047,
42.));
#23628=CARTESIAN_POINT('Ctrl Pts',(30.1449521258473,-0.0648021697998047,
41.7));
#23629=CARTESIAN_POINT('',(30.4314459860325,-1.31309688091278,41.7));
#23630=CARTESIAN_POINT('',(30.4314459860325,-1.31309688091278,42.));
#23631=CARTESIAN_POINT('Ctrl Pts',(30.4314459860325,-1.31309688091278,41.7));
#23632=CARTESIAN_POINT('Ctrl Pts',(30.1449521258473,-0.723056197166443,
41.7));
#23633=CARTESIAN_POINT('Ctrl Pts',(30.1449521258473,-0.0648021697998047,
41.7));
#23634=CARTESIAN_POINT('Ctrl Pts',(31.2738743424416,-2.24420189857483,42.));
#23635=CARTESIAN_POINT('Ctrl Pts',(31.2738743424416,-2.24420189857483,41.7));
#23636=CARTESIAN_POINT('Ctrl Pts',(30.7179398834705,-1.90313756465912,42.));
#23637=CARTESIAN_POINT('Ctrl Pts',(30.7179398834705,-1.90313756465912,41.7));
#23638=CARTESIAN_POINT('Ctrl Pts',(30.4314459860325,-1.31309688091278,42.));
#23639=CARTESIAN_POINT('Ctrl Pts',(30.4314459860325,-1.31309688091278,41.7));
#23640=CARTESIAN_POINT('Ctrl Pts',(31.2738743424416,-2.24420189857483,41.7));
#23641=CARTESIAN_POINT('Ctrl Pts',(30.7179398834705,-1.90313756465912,41.7));
#23642=CARTESIAN_POINT('Ctrl Pts',(30.4314459860325,-1.31309688091278,41.7));
#23643=CARTESIAN_POINT('Origin',(32.5358116813004,0.00170499086380005,41.7));
#23644=CARTESIAN_POINT('Origin',(29.667462259531,1.90995901823044,42.));
#23645=CARTESIAN_POINT('',(29.667462259531,1.90995901823044,41.7));
#23646=CARTESIAN_POINT('',(29.667462259531,1.90995901823044,42.));
#23647=CARTESIAN_POINT('',(28.0133013427258,1.90995901823044,41.7));
#23648=CARTESIAN_POINT('',(29.667462259531,1.90995901823044,41.7));
#23649=CARTESIAN_POINT('',(28.0133013427258,1.90995901823044,42.));
#23650=CARTESIAN_POINT('Origin',(29.667462259531,2.5,42.));
#23651=CARTESIAN_POINT('',(29.667462259531,2.5,41.7));
#23652=CARTESIAN_POINT('',(29.667462259531,2.5,42.));
#23653=CARTESIAN_POINT('',(29.667462259531,2.5,41.7));
#23654=CARTESIAN_POINT('Origin',(25.7042973488569,2.5,42.));
#23655=CARTESIAN_POINT('',(25.7042973488569,2.5,41.7));
#23656=CARTESIAN_POINT('',(25.7042973488569,2.5,42.));
#23657=CARTESIAN_POINT('',(25.7042973488569,2.5,41.7));
#23658=CARTESIAN_POINT('Origin',(25.7042973488569,1.90995901823044,42.));
#23659=CARTESIAN_POINT('',(25.7042973488569,1.90995901823044,41.7));
#23660=CARTESIAN_POINT('',(25.7042973488569,1.90995901823044,42.));
#23661=CARTESIAN_POINT('',(25.7042973488569,1.90995901823044,41.7));
#23662=CARTESIAN_POINT('Origin',(27.3516370356083,1.90995901823044,42.));
#23663=CARTESIAN_POINT('',(27.3516370356083,1.90995901823044,41.7));
#23664=CARTESIAN_POINT('',(27.3516370356083,1.90995901823044,42.));
#23665=CARTESIAN_POINT('',(27.3516370356083,1.90995901823044,41.7));
#23666=CARTESIAN_POINT('Origin',(27.3516370356083,-2.5,42.));
#23667=CARTESIAN_POINT('',(27.3516370356083,-2.5,41.7));
#23668=CARTESIAN_POINT('',(27.3516370356083,-2.5,42.));
#23669=CARTESIAN_POINT('',(27.3516370356083,-2.5,41.7));
#23670=CARTESIAN_POINT('Origin',(28.0133013427258,-2.5,42.));
#23671=CARTESIAN_POINT('',(28.0133013427258,-2.5,41.7));
#23672=CARTESIAN_POINT('',(28.0133013427258,-2.5,42.));
#23673=CARTESIAN_POINT('',(28.0133013427258,-2.5,41.7));
#23674=CARTESIAN_POINT('Origin',(28.0133013427258,1.90995901823044,42.));
#23675=CARTESIAN_POINT('',(28.0133013427258,1.90995901823044,41.7));
#23676=CARTESIAN_POINT('Origin',(27.685879804194,0.,41.7));
#23677=CARTESIAN_POINT('Ctrl Pts',(20.4519100487232,-2.14699864387512,42.));
#23678=CARTESIAN_POINT('Ctrl Pts',(20.4519100487232,-2.14699864387512,41.7));
#23679=CARTESIAN_POINT('Ctrl Pts',(19.9982947669923,-1.7087310552597,42.));
#23680=CARTESIAN_POINT('Ctrl Pts',(19.9982947669923,-1.7087310552597,41.7));
#23681=CARTESIAN_POINT('Ctrl Pts',(19.9982947669923,-1.05388820171356,42.));
#23682=CARTESIAN_POINT('Ctrl Pts',(19.9982947669923,-1.05388820171356,41.7));
#23683=CARTESIAN_POINT('',(20.4519100487232,-2.14699864387512,41.7));
#23684=CARTESIAN_POINT('',(20.4519100487232,-2.14699864387512,42.));
#23685=CARTESIAN_POINT('',(19.9982947669923,-1.05388820171356,41.7));
#23686=CARTESIAN_POINT('Ctrl Pts',(20.4519100487232,-2.14699864387512,41.7));
#23687=CARTESIAN_POINT('Ctrl Pts',(19.9982947669923,-1.7087310552597,41.7));
#23688=CARTESIAN_POINT('Ctrl Pts',(19.9982947669923,-1.05388820171356,41.7));
#23689=CARTESIAN_POINT('',(19.9982947669923,-1.05388820171356,42.));
#23690=CARTESIAN_POINT('Ctrl Pts',(21.6456344723701,-2.58526623249054,42.));
#23691=CARTESIAN_POINT('Ctrl Pts',(21.6456344723701,-2.58526623249054,41.7));
#23692=CARTESIAN_POINT('Ctrl Pts',(20.9055253863335,-2.58526623249054,42.));
#23693=CARTESIAN_POINT('Ctrl Pts',(20.9055253863335,-2.58526623249054,41.7));
#23694=CARTESIAN_POINT('Ctrl Pts',(20.4519100487232,-2.14699864387512,42.));
#23695=CARTESIAN_POINT('Ctrl Pts',(20.4519100487232,-2.14699864387512,41.7));
#23696=CARTESIAN_POINT('',(21.6456344723701,-2.58526623249054,41.7));
#23697=CARTESIAN_POINT('',(21.6456344723701,-2.58526623249054,42.));
#23698=CARTESIAN_POINT('Ctrl Pts',(21.6456344723701,-2.58526623249054,41.7));
#23699=CARTESIAN_POINT('Ctrl Pts',(20.9055253863335,-2.58526623249054,41.7));
#23700=CARTESIAN_POINT('Ctrl Pts',(20.4519100487232,-2.14699864387512,41.7));
#23701=CARTESIAN_POINT('Ctrl Pts',(22.8393588960171,-2.14870393276215,42.));
#23702=CARTESIAN_POINT('Ctrl Pts',(22.8393588960171,-2.14870393276215,41.7));
#23703=CARTESIAN_POINT('Ctrl Pts',(22.3857437074184,-2.58526623249054,42.));
#23704=CARTESIAN_POINT('Ctrl Pts',(22.3857437074184,-2.58526623249054,41.7));
#23705=CARTESIAN_POINT('Ctrl Pts',(21.6456344723701,-2.58526623249054,42.));
#23706=CARTESIAN_POINT('Ctrl Pts',(21.6456344723701,-2.58526623249054,41.7));
#23707=CARTESIAN_POINT('',(22.8393588960171,-2.14870393276215,41.7));
#23708=CARTESIAN_POINT('',(22.8393588960171,-2.14870393276215,42.));
#23709=CARTESIAN_POINT('Ctrl Pts',(22.8393588960171,-2.14870393276215,41.7));
#23710=CARTESIAN_POINT('Ctrl Pts',(22.3857437074184,-2.58526623249054,41.7));
#23711=CARTESIAN_POINT('Ctrl Pts',(21.6456344723701,-2.58526623249054,41.7));
#23712=CARTESIAN_POINT('Ctrl Pts',(23.2929743826389,-1.07094138860703,42.));
#23713=CARTESIAN_POINT('Ctrl Pts',(23.2929743826389,-1.07094138860703,41.7));
#23714=CARTESIAN_POINT('Ctrl Pts',(23.2929743826389,-1.71214163303375,42.));
#23715=CARTESIAN_POINT('Ctrl Pts',(23.2929743826389,-1.71214163303375,41.7));
#23716=CARTESIAN_POINT('Ctrl Pts',(22.8393588960171,-2.14870393276215,42.));
#23717=CARTESIAN_POINT('Ctrl Pts',(22.8393588960171,-2.14870393276215,41.7));
#23718=CARTESIAN_POINT('',(23.2929743826389,-1.07094138860703,41.7));
#23719=CARTESIAN_POINT('',(23.2929743826389,-1.07094138860703,42.));
#23720=CARTESIAN_POINT('Ctrl Pts',(23.2929743826389,-1.07094138860703,41.7));
#23721=CARTESIAN_POINT('Ctrl Pts',(23.2929743826389,-1.71214163303375,41.7));
#23722=CARTESIAN_POINT('Ctrl Pts',(22.8393588960171,-2.14870393276215,41.7));
#23723=CARTESIAN_POINT('Ctrl Pts',(23.0525241792202,-0.272851288318634,
42.));
#23724=CARTESIAN_POINT('Ctrl Pts',(23.0525241792202,-0.272851288318634,
41.7));
#23725=CARTESIAN_POINT('Ctrl Pts',(23.2929743826389,-0.607094168663025,
42.));
#23726=CARTESIAN_POINT('Ctrl Pts',(23.2929743826389,-0.607094168663025,
41.7));
#23727=CARTESIAN_POINT('Ctrl Pts',(23.2929743826389,-1.07094138860703,42.));
#23728=CARTESIAN_POINT('Ctrl Pts',(23.2929743826389,-1.07094138860703,41.7));
#23729=CARTESIAN_POINT('',(23.0525241792202,-0.272851288318634,41.7));
#23730=CARTESIAN_POINT('',(23.0525241792202,-0.272851288318634,42.));
#23731=CARTESIAN_POINT('Ctrl Pts',(23.0525241792202,-0.272851288318634,
41.7));
#23732=CARTESIAN_POINT('Ctrl Pts',(23.2929743826389,-0.607094168663025,
41.7));
#23733=CARTESIAN_POINT('Ctrl Pts',(23.2929743826389,-1.07094138860703,41.7));
#23734=CARTESIAN_POINT('Ctrl Pts',(22.3516373336315,0.211459994316101,42.));
#23735=CARTESIAN_POINT('Ctrl Pts',(22.3516373336315,0.211459994316101,41.7));
#23736=CARTESIAN_POINT('Ctrl Pts',(22.8120739758015,0.0613915920257568,
42.));
#23737=CARTESIAN_POINT('Ctrl Pts',(22.8120739758015,0.0613915920257568,
41.7));
#23738=CARTESIAN_POINT('Ctrl Pts',(23.0525241792202,-0.272851288318634,
42.));
#23739=CARTESIAN_POINT('Ctrl Pts',(23.0525241792202,-0.272851288318634,
41.7));
#23740=CARTESIAN_POINT('',(22.3516373336315,0.211459994316101,41.7));
#23741=CARTESIAN_POINT('',(22.3516373336315,0.211459994316101,42.));
#23742=CARTESIAN_POINT('Ctrl Pts',(22.3516373336315,0.211459994316101,41.7));
#23743=CARTESIAN_POINT('Ctrl Pts',(22.8120739758015,0.0613915920257568,
41.7));
#23744=CARTESIAN_POINT('Ctrl Pts',(23.0525241792202,-0.272851288318634,
41.7));
#23745=CARTESIAN_POINT('Ctrl Pts',(22.9058663547039,0.608799457550049,42.));
#23746=CARTESIAN_POINT('Ctrl Pts',(22.9058663547039,0.608799457550049,41.7));
#23747=CARTESIAN_POINT('Ctrl Pts',(22.7233971655369,0.351296067237854,42.));
#23748=CARTESIAN_POINT('Ctrl Pts',(22.7233971655369,0.351296067237854,41.7));
#23749=CARTESIAN_POINT('Ctrl Pts',(22.3516373336315,0.211459994316101,42.));
#23750=CARTESIAN_POINT('Ctrl Pts',(22.3516373336315,0.211459994316101,41.7));
#23751=CARTESIAN_POINT('',(22.9058663547039,0.608799457550049,41.7));
#23752=CARTESIAN_POINT('',(22.9058663547039,0.608799457550049,42.));
#23753=CARTESIAN_POINT('Ctrl Pts',(22.9058663547039,0.608799457550049,41.7));
#23754=CARTESIAN_POINT('Ctrl Pts',(22.7233971655369,0.351296067237854,41.7));
#23755=CARTESIAN_POINT('Ctrl Pts',(22.3516373336315,0.211459994316101,41.7));
#23756=CARTESIAN_POINT('Ctrl Pts',(23.0883358418941,1.21418833732605,42.));
#23757=CARTESIAN_POINT('Ctrl Pts',(23.0883358418941,1.21418833732605,41.7));
#23758=CARTESIAN_POINT('Ctrl Pts',(23.0883358418941,0.866302847862244,42.));
#23759=CARTESIAN_POINT('Ctrl Pts',(23.0883358418941,0.866302847862244,41.7));
#23760=CARTESIAN_POINT('Ctrl Pts',(22.9058663547039,0.608799457550049,42.));
#23761=CARTESIAN_POINT('Ctrl Pts',(22.9058663547039,0.608799457550049,41.7));
#23762=CARTESIAN_POINT('',(23.0883358418941,1.21418833732605,41.7));
#23763=CARTESIAN_POINT('',(23.0883358418941,1.21418833732605,42.));
#23764=CARTESIAN_POINT('Ctrl Pts',(23.0883358418941,1.21418833732605,41.7));
#23765=CARTESIAN_POINT('Ctrl Pts',(23.0883358418941,0.866302847862244,41.7));
#23766=CARTESIAN_POINT('Ctrl Pts',(22.9058663547039,0.608799457550049,41.7));
#23767=CARTESIAN_POINT('Ctrl Pts',(22.68929079175,2.14017748832703,42.));
#23768=CARTESIAN_POINT('Ctrl Pts',(22.68929079175,2.14017748832703,41.7));
#23769=CARTESIAN_POINT('Ctrl Pts',(23.0883358418941,1.75989091396332,42.));
#23770=CARTESIAN_POINT('Ctrl Pts',(23.0883358418941,1.75989091396332,41.7));
#23771=CARTESIAN_POINT('Ctrl Pts',(23.0883358418941,1.21418833732605,42.));
#23772=CARTESIAN_POINT('Ctrl Pts',(23.0883358418941,1.21418833732605,41.7));
#23773=CARTESIAN_POINT('',(22.68929079175,2.14017748832703,41.7));
#23774=CARTESIAN_POINT('',(22.68929079175,2.14017748832703,42.));
#23775=CARTESIAN_POINT('Ctrl Pts',(22.68929079175,2.14017748832703,41.7));
#23776=CARTESIAN_POINT('Ctrl Pts',(23.0883358418941,1.75989091396332,41.7));
#23777=CARTESIAN_POINT('Ctrl Pts',(23.0883358418941,1.21418833732605,41.7));
#23778=CARTESIAN_POINT('Ctrl Pts',(21.6354024410248,2.52046346664429,42.));
#23779=CARTESIAN_POINT('Ctrl Pts',(21.6354024410248,2.52046346664429,41.7));
#23780=CARTESIAN_POINT('Ctrl Pts',(22.2902457416058,2.52046346664429,42.));
#23781=CARTESIAN_POINT('Ctrl Pts',(22.2902457416058,2.52046346664429,41.7));
#23782=CARTESIAN_POINT('Ctrl Pts',(22.68929079175,2.14017748832703,42.));
#23783=CARTESIAN_POINT('Ctrl Pts',(22.68929079175,2.14017748832703,41.7));
#23784=CARTESIAN_POINT('',(21.6354024410248,2.52046346664429,41.7));
#23785=CARTESIAN_POINT('',(21.6354024410248,2.52046346664429,42.));
#23786=CARTESIAN_POINT('Ctrl Pts',(21.6354024410248,2.52046346664429,41.7));
#23787=CARTESIAN_POINT('Ctrl Pts',(22.2902457416058,2.52046346664429,41.7));
#23788=CARTESIAN_POINT('Ctrl Pts',(22.68929079175,2.14017748832703,41.7));
#23789=CARTESIAN_POINT('Ctrl Pts',(20.5917463451624,2.14870393276215,42.));
#23790=CARTESIAN_POINT('Ctrl Pts',(20.5917463451624,2.14870393276215,41.7));
#23791=CARTESIAN_POINT('Ctrl Pts',(20.9839700162411,2.52046346664429,42.));
#23792=CARTESIAN_POINT('Ctrl Pts',(20.9839700162411,2.52046346664429,41.7));
#23793=CARTESIAN_POINT('Ctrl Pts',(21.6354024410248,2.52046346664429,42.));
#23794=CARTESIAN_POINT('Ctrl Pts',(21.6354024410248,2.52046346664429,41.7));
#23795=CARTESIAN_POINT('',(20.5917463451624,2.14870393276215,41.7));
#23796=CARTESIAN_POINT('',(20.5917463451624,2.14870393276215,42.));
#23797=CARTESIAN_POINT('Ctrl Pts',(20.5917463451624,2.14870393276215,41.7));
#23798=CARTESIAN_POINT('Ctrl Pts',(20.9839700162411,2.52046346664429,41.7));
#23799=CARTESIAN_POINT('Ctrl Pts',(21.6354024410248,2.52046346664429,41.7));
#23800=CARTESIAN_POINT('Ctrl Pts',(20.1995225995779,1.23124152421951,42.));
#23801=CARTESIAN_POINT('Ctrl Pts',(20.1995225995779,1.23124152421951,41.7));
#23802=CARTESIAN_POINT('Ctrl Pts',(20.1995225995779,1.77694410085678,42.));
#23803=CARTESIAN_POINT('Ctrl Pts',(20.1995225995779,1.77694410085678,41.7));
#23804=CARTESIAN_POINT('Ctrl Pts',(20.5917463451624,2.14870393276215,42.));
#23805=CARTESIAN_POINT('Ctrl Pts',(20.5917463451624,2.14870393276215,41.7));
#23806=CARTESIAN_POINT('',(20.1995225995779,1.23124152421951,41.7));
#23807=CARTESIAN_POINT('',(20.1995225995779,1.23124152421951,42.));
#23808=CARTESIAN_POINT('Ctrl Pts',(20.1995225995779,1.23124152421951,41.7));
#23809=CARTESIAN_POINT('Ctrl Pts',(20.1995225995779,1.77694410085678,41.7));
#23810=CARTESIAN_POINT('Ctrl Pts',(20.5917463451624,2.14870393276215,41.7));
#23811=CARTESIAN_POINT('Ctrl Pts',(20.3836972266436,0.610504746437073,42.));
#23812=CARTESIAN_POINT('Ctrl Pts',(20.3836972266436,0.610504746437073,41.7));
#23813=CARTESIAN_POINT('Ctrl Pts',(20.1995225995779,0.869713723659515,42.));
#23814=CARTESIAN_POINT('Ctrl Pts',(20.1995225995779,0.869713723659515,41.7));
#23815=CARTESIAN_POINT('Ctrl Pts',(20.1995225995779,1.23124152421951,42.));
#23816=CARTESIAN_POINT('Ctrl Pts',(20.1995225995779,1.23124152421951,41.7));
#23817=CARTESIAN_POINT('',(20.3836972266436,0.610504746437073,41.7));
#23818=CARTESIAN_POINT('',(20.3836972266436,0.610504746437073,42.));
#23819=CARTESIAN_POINT('Ctrl Pts',(20.3836972266436,0.610504746437073,41.7));
#23820=CARTESIAN_POINT('Ctrl Pts',(20.1995225995779,0.869713723659515,41.7));
#23821=CARTESIAN_POINT('Ctrl Pts',(20.1995225995779,1.23124152421951,41.7));
#23822=CARTESIAN_POINT('Ctrl Pts',(20.94986371696,0.211459994316101,42.));
#23823=CARTESIAN_POINT('Ctrl Pts',(20.94986371696,0.211459994316101,41.7));
#23824=CARTESIAN_POINT('Ctrl Pts',(20.5678718537092,0.351296067237854,42.));
#23825=CARTESIAN_POINT('Ctrl Pts',(20.5678718537092,0.351296067237854,41.7));
#23826=CARTESIAN_POINT('Ctrl Pts',(20.3836972266436,0.610504746437073,42.));
#23827=CARTESIAN_POINT('Ctrl Pts',(20.3836972266436,0.610504746437073,41.7));
#23828=CARTESIAN_POINT('',(20.94986371696,0.211459994316101,41.7));
#23829=CARTESIAN_POINT('',(20.94986371696,0.211459994316101,42.));
#23830=CARTESIAN_POINT('Ctrl Pts',(20.94986371696,0.211459994316101,41.7));
#23831=CARTESIAN_POINT('Ctrl Pts',(20.5678718537092,0.351296067237854,41.7));
#23832=CARTESIAN_POINT('Ctrl Pts',(20.3836972266436,0.610504746437073,41.7));
#23833=CARTESIAN_POINT('Ctrl Pts',(20.2455662563443,-0.237039625644684,
42.));
#23834=CARTESIAN_POINT('Ctrl Pts',(20.2455662563443,-0.237039625644684,
41.7));
#23835=CARTESIAN_POINT('Ctrl Pts',(20.4928377270699,0.0920873880386353,
42.));
#23836=CARTESIAN_POINT('Ctrl Pts',(20.4928377270699,0.0920873880386353,
41.7));
#23837=CARTESIAN_POINT('Ctrl Pts',(20.94986371696,0.211459994316101,42.));
#23838=CARTESIAN_POINT('Ctrl Pts',(20.94986371696,0.211459994316101,41.7));
#23839=CARTESIAN_POINT('',(20.2455662563443,-0.237039625644684,41.7));
#23840=CARTESIAN_POINT('',(20.2455662563443,-0.237039625644684,42.));
#23841=CARTESIAN_POINT('Ctrl Pts',(20.2455662563443,-0.237039625644684,
41.7));
#23842=CARTESIAN_POINT('Ctrl Pts',(20.4928377270699,0.0920873880386353,
41.7));
#23843=CARTESIAN_POINT('Ctrl Pts',(20.94986371696,0.211459994316101,41.7));
#23844=CARTESIAN_POINT('Ctrl Pts',(19.9982947669923,-1.05388820171356,42.));
#23845=CARTESIAN_POINT('Ctrl Pts',(19.9982947669923,-1.05388820171356,41.7));
#23846=CARTESIAN_POINT('Ctrl Pts',(19.9982947669923,-0.566166639328003,
42.));
#23847=CARTESIAN_POINT('Ctrl Pts',(19.9982947669923,-0.566166639328003,
41.7));
#23848=CARTESIAN_POINT('Ctrl Pts',(20.2455662563443,-0.237039625644684,
42.));
#23849=CARTESIAN_POINT('Ctrl Pts',(20.2455662563443,-0.237039625644684,
41.7));
#23850=CARTESIAN_POINT('Ctrl Pts',(19.9982947669923,-1.05388820171356,41.7));
#23851=CARTESIAN_POINT('Ctrl Pts',(19.9982947669923,-0.566166639328003,
41.7));
#23852=CARTESIAN_POINT('Ctrl Pts',(20.2455662563443,-0.237039625644684,
41.7));
#23853=CARTESIAN_POINT('Origin',(21.6456345748156,-0.0324013829231262,41.7));
#23854=CARTESIAN_POINT('Origin',(39.0330834686756,-2.5,42.));
#23855=CARTESIAN_POINT('',(39.0330834686756,-2.5,41.7));
#23856=CARTESIAN_POINT('',(39.0330834686756,-2.5,42.));
#23857=CARTESIAN_POINT('',(36.4068896323442,1.42905861139297,41.7));
#23858=CARTESIAN_POINT('',(39.0330834686756,-2.5,41.7));
#23859=CARTESIAN_POINT('',(36.4068896323442,1.42905861139297,42.));
#23860=CARTESIAN_POINT('Origin',(39.7118009626865,-2.5,42.));
#23861=CARTESIAN_POINT('',(39.7118009626865,-2.5,41.7));
#23862=CARTESIAN_POINT('',(39.7118009626865,-2.5,42.));
#23863=CARTESIAN_POINT('',(39.7118009626865,-2.5,41.7));
#23864=CARTESIAN_POINT('Origin',(39.7118009626865,2.5,42.));
#23865=CARTESIAN_POINT('',(39.7118009626865,2.5,41.7));
#23866=CARTESIAN_POINT('',(39.7118009626865,2.5,42.));
#23867=CARTESIAN_POINT('',(39.7118009626865,2.5,41.7));
#23868=CARTESIAN_POINT('Origin',(39.0774215757847,2.5,42.));
#23869=CARTESIAN_POINT('',(39.0774215757847,2.5,41.7));
#23870=CARTESIAN_POINT('',(39.0774215757847,2.5,42.));
#23871=CARTESIAN_POINT('',(39.0774215757847,2.5,41.7));
#23872=CARTESIAN_POINT('Origin',(39.0774215757847,-1.42564833164215,42.));
#23873=CARTESIAN_POINT('',(39.0774215757847,-1.42564833164215,41.7));
#23874=CARTESIAN_POINT('',(39.0774215757847,-1.42564833164215,42.));
#23875=CARTESIAN_POINT('',(39.0774215757847,-1.42564833164215,41.7));
#23876=CARTESIAN_POINT('Origin',(36.4512279629707,2.5,42.));
#23877=CARTESIAN_POINT('',(36.4512279629707,2.5,41.7));
#23878=CARTESIAN_POINT('',(36.4512279629707,2.5,42.));
#23879=CARTESIAN_POINT('',(36.4512279629707,2.5,41.7));
#23880=CARTESIAN_POINT('Origin',(35.772510394454,2.5,42.));
#23881=CARTESIAN_POINT('',(35.772510394454,2.5,41.7));
#23882=CARTESIAN_POINT('',(35.772510394454,2.5,42.));
#23883=CARTESIAN_POINT('',(35.772510394454,2.5,41.7));
#23884=CARTESIAN_POINT('Origin',(35.772510394454,-2.5,42.));
#23885=CARTESIAN_POINT('',(35.772510394454,-2.5,41.7));
#23886=CARTESIAN_POINT('',(35.772510394454,-2.5,42.));
#23887=CARTESIAN_POINT('',(35.772510394454,-2.5,41.7));
#23888=CARTESIAN_POINT('Origin',(36.4068896323442,-2.5,42.));
#23889=CARTESIAN_POINT('',(36.4068896323442,-2.5,41.7));
#23890=CARTESIAN_POINT('',(36.4068896323442,-2.5,42.));
#23891=CARTESIAN_POINT('',(36.4068896323442,-2.5,41.7));
#23892=CARTESIAN_POINT('Origin',(36.4068896323442,1.42905861139297,42.));
#23893=CARTESIAN_POINT('',(36.4068896323442,1.42905861139297,41.7));
#23894=CARTESIAN_POINT('Origin',(37.7421556785703,0.,41.7));
#23895=CARTESIAN_POINT('Origin',(15.,0.,0.));
#23896=CARTESIAN_POINT('',(9.9,-3.73517273739943E-16,3.05));
#23897=CARTESIAN_POINT('',(15.,3.73517273739943E-16,3.05));
#23898=CARTESIAN_POINT('Origin',(9.9,0.,0.));
#23899=CARTESIAN_POINT('Origin',(9.9,0.,0.));
#23900=CARTESIAN_POINT('Origin',(91.6,0.,0.));
#23901=CARTESIAN_POINT('',(91.1,-21.05,-2.57788151220518E-15));
#23902=CARTESIAN_POINT('Origin',(91.1,0.,0.));
#23903=CARTESIAN_POINT('',(91.6,-21.525,-2.63605223516468E-15));
#23904=CARTESIAN_POINT('Origin',(80.05,0.,0.));
#23905=CARTESIAN_POINT('',(80.05,-21.05,-2.57788151220518E-15));
#23906=CARTESIAN_POINT('Origin',(42.,22.,8.5));
#23907=CARTESIAN_POINT('Origin',(84.,-22.,22.));
#23908=CARTESIAN_POINT('Origin',(42.,22.,8.5));
#23909=CARTESIAN_POINT('',(0.,0.,0.));
#23910=CARTESIAN_POINT('Origin',(80.4,0.,0.));
#23911=CARTESIAN_POINT('',(69.2061568471518,-20.9251045326925,0.000537903476663659));
#23912=CARTESIAN_POINT('',(68.9938431528481,-20.9246928645182,0.000347110336330147));
#23913=CARTESIAN_POINT('',(80.4,-20.925,-2.56257342721584E-15));
#23914=CARTESIAN_POINT('',(68.725,9.00143038127672,18.8903144283542));
#23915=CARTESIAN_POINT('Ctrl Pts',(69.2061568471518,-20.9251045326925,0.000537903476663659));
#23916=CARTESIAN_POINT('Ctrl Pts',(69.1973932851687,-20.925892267353,0.768641798467955));
#23917=CARTESIAN_POINT('Ctrl Pts',(69.1886297231856,-20.8844127756245,1.53666082027718));
#23918=CARTESIAN_POINT('Ctrl Pts',(69.1798661612025,-20.8000149036333,2.29993382021793));
#23919=CARTESIAN_POINT('Ctrl Pts',(69.140247873288,-20.4184692263878,5.75053638654726));
#23920=CARTESIAN_POINT('Ctrl Pts',(69.1006295853734,-19.1597744826372,9.10414161453262));
#23921=CARTESIAN_POINT('Ctrl Pts',(69.0610112974588,-17.1767275083919,11.9536689002946));
#23922=CARTESIAN_POINT('Ctrl Pts',(69.0213930095442,-15.1936805341465,14.8031961860566));
#23923=CARTESIAN_POINT('Ctrl Pts',(68.9817747216296,-12.4862813294065,17.1486455295952));
#23924=CARTESIAN_POINT('Ctrl Pts',(68.9421564337151,-9.38318674595559,18.7052533021947));
#23925=CARTESIAN_POINT('Ctrl Pts',(68.9025381458005,-6.28009216250464,20.2618610747941));
#23926=CARTESIAN_POINT('Ctrl Pts',(68.8629198578859,-2.7813022003428,21.0296272764544));
#23927=CARTESIAN_POINT('Ctrl Pts',(68.8233015699713,0.688453527214973,20.9154363519887));
#23928=CARTESIAN_POINT('Ctrl Pts',(68.7905343799809,3.55819250711376,20.8209921971777));
#23929=CARTESIAN_POINT('Ctrl Pts',(68.7577671899904,6.40807065798892,20.1232464597002));
#23930=CARTESIAN_POINT('Ctrl Pts',(68.725,9.00178625489531,18.890518144815));
#23931=CARTESIAN_POINT('',(68.725,-9.00107450765889,18.890110711893));
#23932=CARTESIAN_POINT('Origin',(68.725,0.,0.));
#23933=CARTESIAN_POINT('Ctrl Pts',(68.725,-9.0010745076589,18.890110711893));
#23934=CARTESIAN_POINT('Ctrl Pts',(68.7646182879146,-12.1359393145908,17.3963581273268));
#23935=CARTESIAN_POINT('Ctrl Pts',(68.8042365758292,-14.8902410183971,15.1079808431403));
#23936=CARTESIAN_POINT('Ctrl Pts',(68.8438548637437,-16.9306635496692,12.2997765477629));
#23937=CARTESIAN_POINT('Ctrl Pts',(68.8834731516583,-18.9710860809414,9.49157225238549));
#23938=CARTESIAN_POINT('Ctrl Pts',(68.9230914395729,-20.2976294396793,6.16354094581719));
#23939=CARTESIAN_POINT('Ctrl Pts',(68.9627097274875,-20.7491077747907,2.72122018983935));
#23940=CARTESIAN_POINT('Ctrl Pts',(68.973087535941,-20.8673702219923,1.81952182472461));
#23941=CARTESIAN_POINT('Ctrl Pts',(68.9834653443946,-20.9255899684262,0.909981474127051));
#23942=CARTESIAN_POINT('Ctrl Pts',(68.9938431528481,-20.9246928645182,0.000347110336330147));
#23943=CARTESIAN_POINT('Origin',(80.4,0.,0.));
#23944=CARTESIAN_POINT('',(70.7061568471518,-20.9257818388602,-0.000467423370275055));
#23945=CARTESIAN_POINT('',(70.4938431528481,-20.9261779264193,-0.000381460781396608));
#23946=CARTESIAN_POINT('',(80.4,-20.925,-2.56257342721584E-15));
#23947=CARTESIAN_POINT('Ctrl Pts',(70.7061568471518,-20.9257818388602,-0.000467423370275055));
#23948=CARTESIAN_POINT('Ctrl Pts',(70.6728127401437,-20.9229483509825,2.92178557156433));
#23949=CARTESIAN_POINT('Ctrl Pts',(70.6394686331356,-20.3051998739425,5.84519881683506));
#23950=CARTESIAN_POINT('Ctrl Pts',(70.6061245261274,-19.1164161743571,8.51427815820994));
#23951=CARTESIAN_POINT('Ctrl Pts',(70.5665062382128,-17.7039454530144,11.6855837741494));
#23952=CARTESIAN_POINT('Ctrl Pts',(70.5268879502982,-15.4853242409376,14.4978372802698));
#23953=CARTESIAN_POINT('Ctrl Pts',(70.4872696623837,-12.7298766583704,16.6096520162404));
#23954=CARTESIAN_POINT('Ctrl Pts',(70.4476513744691,-9.97442907580324,18.7214667522109));
#23955=CARTESIAN_POINT('Ctrl Pts',(70.4080330865545,-6.68215512274561,20.1328427180316));
#23956=CARTESIAN_POINT('Ctrl Pts',(70.3684147986399,-3.25271237917639,20.6724493517347));
#23957=CARTESIAN_POINT('Ctrl Pts',(70.3287965107253,0.176730364392844,21.2120559854378));
#23958=CARTESIAN_POINT('Ctrl Pts',(70.2891782228108,3.74334189847368,20.8798932870233));
#23959=CARTESIAN_POINT('Ctrl Pts',(70.2495599348962,7.01416209926513,19.7162833642022));
#23960=CARTESIAN_POINT('Ctrl Pts',(70.2099416469816,10.2849823000566,18.5526734413812));
#23961=CARTESIAN_POINT('Ctrl Pts',(70.170323359067,13.2600111675587,16.5576162941535));
#23962=CARTESIAN_POINT('Ctrl Pts',(70.1307050711524,15.5781023176152,13.9732969767378));
#23963=CARTESIAN_POINT('Ctrl Pts',(70.0910867832378,17.8961934676717,11.3889776593222));
#23964=CARTESIAN_POINT('Ctrl Pts',(70.0514684953233,19.5573469002827,8.21539617171875));
#23965=CARTESIAN_POINT('Ctrl Pts',(70.0118502074087,20.3599109362165,4.83780181075189));
#23966=CARTESIAN_POINT('Ctrl Pts',(69.9722319194941,21.1624749721504,1.46020744978499));
#23967=CARTESIAN_POINT('Ctrl Pts',(69.9326136315796,21.1064496114072,-2.12139978454527));
#23968=CARTESIAN_POINT('Ctrl Pts',(69.892995343665,20.1986359219932,-5.47223959788331));
#23969=CARTESIAN_POINT('Ctrl Pts',(69.8533770557504,19.2908222325792,-8.82307941122133));
#23970=CARTESIAN_POINT('Ctrl Pts',(69.8137587678358,17.5312202144946,-11.9431518035671));
#23971=CARTESIAN_POINT('Ctrl Pts',(69.7741404799212,15.1334324590649,-14.4537028000153));
#23972=CARTESIAN_POINT('Ctrl Pts',(69.7345221920066,12.7356447036353,-16.9642537964634));
#23973=CARTESIAN_POINT('Ctrl Pts',(69.6949039040921,9.6996712108608,-18.8652833970139));
#23974=CARTESIAN_POINT('Ctrl Pts',(69.6552856161775,6.39405661300567,-19.926021496295));
#23975=CARTESIAN_POINT('Ctrl Pts',(69.6156673282629,3.08844201515051,-20.9867595955761));
#23976=CARTESIAN_POINT('Ctrl Pts',(69.5760490403483,-0.486813687785254,
-21.2072061935878));
#23977=CARTESIAN_POINT('Ctrl Pts',(69.5364307524337,-3.89770107861504,-20.5605992296267));
#23978=CARTESIAN_POINT('Ctrl Pts',(69.4968124645191,-7.3085884694448,-19.9139922656657));
#23979=CARTESIAN_POINT('Ctrl Pts',(69.4571941766046,-10.5551075481686,-18.400331739732));
#23980=CARTESIAN_POINT('Ctrl Pts',(69.41757588869,-13.2431549501084,-16.2033677003751));
#23981=CARTESIAN_POINT('Ctrl Pts',(69.3779576007755,-15.9312023520481,-14.0064036610182));
#23982=CARTESIAN_POINT('Ctrl Pts',(69.3383393128609,-18.0607780772039,-11.126136108238));
#23983=CARTESIAN_POINT('Ctrl Pts',(69.2987210249463,-19.3733676344116,-7.91220237951135));
#23984=CARTESIAN_POINT('Ctrl Pts',(69.2678662990148,-20.3956124910162,-5.40919052358253));
#23985=CARTESIAN_POINT('Ctrl Pts',(69.2370115730833,-20.922331078576,-2.70380026547276));
#23986=CARTESIAN_POINT('Ctrl Pts',(69.2061568471518,-20.9251045326925,0.000537903476663659));
#23987=CARTESIAN_POINT('Ctrl Pts',(68.9938431528481,-20.9246928645182,0.000347110336330147));
#23988=CARTESIAN_POINT('Ctrl Pts',(69.0230836323092,-20.9221651874547,-2.56263572467314));
#23989=CARTESIAN_POINT('Ctrl Pts',(69.0523241117702,-20.4503176146989,-5.1263649164617));
#23990=CARTESIAN_POINT('Ctrl Pts',(69.0815645912312,-19.5298600150513,-7.51753008448147));
#23991=CARTESIAN_POINT('Ctrl Pts',(69.1211828791458,-18.2827206087156,-10.7573493974371));
#23992=CARTESIAN_POINT('Ctrl Pts',(69.1608011670604,-16.2120284845591,-13.6803778179609));
#23993=CARTESIAN_POINT('Ctrl Pts',(69.2004194549749,-13.5691025042824,-15.9314525116625));
#23994=CARTESIAN_POINT('Ctrl Pts',(69.2400377428895,-10.9261765240057,-18.1825272053641));
#23995=CARTESIAN_POINT('Ctrl Pts',(69.2796560308041,-7.71101668760872,-19.7616481722434));
#23996=CARTESIAN_POINT('Ctrl Pts',(69.3192743187187,-4.31394387820961,-20.4772883046503));
#23997=CARTESIAN_POINT('Ctrl Pts',(69.3588926066333,-0.916871068810491,
-21.1929284370572));
#23998=CARTESIAN_POINT('Ctrl Pts',(69.3985108945478,2.66211471359076,-21.0450877349916));
#23999=CARTESIAN_POINT('Ctrl Pts',(69.4381291824624,5.98856361433238,-20.0516283795423));
#24000=CARTESIAN_POINT('Ctrl Pts',(69.477747470377,9.31501251507399,-19.0581690240929));
#24001=CARTESIAN_POINT('Ctrl Pts',(69.5173657582916,12.388924534156,-17.2190910152599));
#24002=CARTESIAN_POINT('Ctrl Pts',(69.5569840462062,14.8371432934536,-14.7576877650994));
#24003=CARTESIAN_POINT('Ctrl Pts',(69.5966023341207,17.2853620527513,-12.2962845149389));
#24004=CARTESIAN_POINT('Ctrl Pts',(69.6362206220353,19.1078875522646,-9.21255602345092));
#24005=CARTESIAN_POINT('Ctrl Pts',(69.6758389099499,20.0834819577218,-5.88082212359926));
#24006=CARTESIAN_POINT('Ctrl Pts',(69.7154571978645,21.059076363179,-2.54908822374764));
#24007=CARTESIAN_POINT('Ctrl Pts',(69.755075485779,21.1877396745801,1.03065108446768));
#24008=CARTESIAN_POINT('Ctrl Pts',(69.7946937736936,20.4538514891497,4.42383093525681));
#24009=CARTESIAN_POINT('Ctrl Pts',(69.8343120616082,19.7199633037193,7.81701078604597));
#24010=CARTESIAN_POINT('Ctrl Pts',(69.8739303495228,18.1235236214575,11.0236311794089));
#24011=CARTESIAN_POINT('Ctrl Pts',(69.9135486374374,15.8583291813194,13.6544379008176));
#24012=CARTESIAN_POINT('Ctrl Pts',(69.953166925352,13.5931347411813,16.2852446222263));
#24013=CARTESIAN_POINT('Ctrl Pts',(69.9927852132666,10.659185543167,18.3402376716807));
#24014=CARTESIAN_POINT('Ctrl Pts',(70.0324035011811,7.41264078387936,19.5699532923244));
#24015=CARTESIAN_POINT('Ctrl Pts',(70.0720217890957,4.1660960245917,20.7996689129682));
#24016=CARTESIAN_POINT('Ctrl Pts',(70.1116400770103,0.606955704030666,21.2041071048013));
#24017=CARTESIAN_POINT('Ctrl Pts',(70.1512583649248,-2.8327267895864,20.7341735427668));
#24018=CARTESIAN_POINT('Ctrl Pts',(70.1908766528394,-6.27240928320346,20.2642399807324));
#24019=CARTESIAN_POINT('Ctrl Pts',(70.230494940754,-9.59263394987655,18.9199346648303));
#24020=CARTESIAN_POINT('Ctrl Pts',(70.2701132286686,-12.3903503097503,16.864445520801));
#24021=CARTESIAN_POINT('Ctrl Pts',(70.3097315165832,-15.1880666696241,14.8089563767717));
#24022=CARTESIAN_POINT('Ctrl Pts',(70.3493498044977,-17.4632747226986,12.0422834046151));
#24023=CARTESIAN_POINT('Ctrl Pts',(70.3889680924123,-18.9397810715315,8.90028051227176));
#24024=CARTESIAN_POINT('Ctrl Pts',(70.4239264458909,-20.2426195729629,6.12784249127099));
#24025=CARTESIAN_POINT('Ctrl Pts',(70.4588847993695,-20.9235944663035,3.06317519724849));
#24026=CARTESIAN_POINT('Ctrl Pts',(70.4938431528481,-20.9261779264193,-0.000381460781396608));
#24027=CARTESIAN_POINT('Origin',(80.4,0.,0.));
#24028=CARTESIAN_POINT('',(72.2061568471519,-20.9232657042053,0.000120932580692235));
#24029=CARTESIAN_POINT('',(71.9938431528481,-20.923224691771,-9.04407733959185E-6));
#24030=CARTESIAN_POINT('',(80.4,-20.925,-2.56257342721584E-15));
#24031=CARTESIAN_POINT('Ctrl Pts',(72.2061568471519,-20.9232657042053,0.000120932580692235));
#24032=CARTESIAN_POINT('Ctrl Pts',(72.1878504830332,-20.9235905266545,1.6050316355066));
#24033=CARTESIAN_POINT('Ctrl Pts',(72.1695441189146,-20.7412699845247,3.20986972041554));
#24034=CARTESIAN_POINT('Ctrl Pts',(72.151237754796,-20.3754940092624,4.77174431109023));
#24035=CARTESIAN_POINT('Ctrl Pts',(72.1116194668814,-19.5838885431924,8.15192383875766));
#24036=CARTESIAN_POINT('Ctrl Pts',(72.0720011789668,-17.9330365351294,11.3308761079985));
#24037=CARTESIAN_POINT('Ctrl Pts',(72.0323828910522,-15.6233391450283,13.9226999483342));
#24038=CARTESIAN_POINT('Ctrl Pts',(71.9927646031376,-13.3136417549272,16.5145237886699));
#24039=CARTESIAN_POINT('Ctrl Pts',(71.9531463152231,-10.3450989827881,18.5192192001004));
#24040=CARTESIAN_POINT('Ctrl Pts',(71.9135280273085,-7.07806985050165,19.693431064274));
#24041=CARTESIAN_POINT('Ctrl Pts',(71.8739097393939,-3.81104071821527,20.8676429284476));
#24042=CARTESIAN_POINT('Ctrl Pts',(71.8342914514793,-0.245525225781651,
21.2113712453643));
#24043=CARTESIAN_POINT('Ctrl Pts',(71.7946731635647,3.1856495550627,20.6828899529123));
#24044=CARTESIAN_POINT('Ctrl Pts',(71.7550548756502,6.61682433590708,20.1544086604602));
#24045=CARTESIAN_POINT('Ctrl Pts',(71.7154365877356,9.91365840516219,18.7537177586395));
#24046=CARTESIAN_POINT('Ctrl Pts',(71.675818299821,12.6759406182611,16.650850709023));
#24047=CARTESIAN_POINT('Ctrl Pts',(71.6362000119064,15.43822283136,14.5479836594065));
#24048=CARTESIAN_POINT('Ctrl Pts',(71.5965817239918,17.6659531883027,11.7429404619943));
#24049=CARTESIAN_POINT('Ctrl Pts',(71.5569634360773,19.0887017865803,8.57623250588363));
#24050=CARTESIAN_POINT('Ctrl Pts',(71.5173451481627,20.511450384858,5.40952454977299));
#24051=CARTESIAN_POINT('Ctrl Pts',(71.4777268602481,21.1292172244705,1.88115183496394));
#24052=CARTESIAN_POINT('Ctrl Pts',(71.4381085723336,20.8670100040871,-1.58056742383));
#24053=CARTESIAN_POINT('Ctrl Pts',(71.398490284419,20.6048027837037,-5.04228668262394));
#24054=CARTESIAN_POINT('Ctrl Pts',(71.3588719965044,19.4626215033242,-8.43735248540277));
#24055=CARTESIAN_POINT('Ctrl Pts',(71.3192537085898,17.5791184784511,-11.3536290855461));
#24056=CARTESIAN_POINT('Ctrl Pts',(71.2796354206752,15.695615453578,-14.2699056856894));
#24057=CARTESIAN_POINT('Ctrl Pts',(71.2400171327607,13.0707906842112,-16.7073930831972));
#24058=CARTESIAN_POINT('Ctrl Pts',(71.2003988448461,10.0232783821906,-18.3701984302307));
#24059=CARTESIAN_POINT('Ctrl Pts',(71.1607805569315,6.97576608016998,-20.0330037772643));
#24060=CARTESIAN_POINT('Ctrl Pts',(71.1211622690169,3.50556624549558,-20.9211270738236));
#24061=CARTESIAN_POINT('Ctrl Pts',(71.0815439811023,0.0339353377155988,
-20.9267567549895));
#24062=CARTESIAN_POINT('Ctrl Pts',(71.0419256931877,-3.43769557006433,-20.9323864361554));
#24063=CARTESIAN_POINT('Ctrl Pts',(71.0023074052732,-6.91075755094984,-20.0555225019279));
#24064=CARTESIAN_POINT('Ctrl Pts',(70.9626891173586,-9.96364670214212,-18.4026097141319));
#24065=CARTESIAN_POINT('Ctrl Pts',(70.923070829444,-13.0165358533344,-16.7496969263358));
#24066=CARTESIAN_POINT('Ctrl Pts',(70.8834525415295,-15.6492521748335,-14.3207352849711));
#24067=CARTESIAN_POINT('Ctrl Pts',(70.8438342536149,-17.5422034790138,-11.4105826752288));
#24068=CARTESIAN_POINT('Ctrl Pts',(70.8042159657003,-19.435154783194,-8.5004300654865));
#24069=CARTESIAN_POINT('Ctrl Pts',(70.7645976777857,-20.5883410700555,-5.10908648736654));
#24070=CARTESIAN_POINT('Ctrl Pts',(70.7249793898711,-20.861774098182,-1.64823583542732));
#24071=CARTESIAN_POINT('Ctrl Pts',(70.7187052089647,-20.9050765318448,-1.10015553657129));
#24072=CARTESIAN_POINT('Ctrl Pts',(70.7124310280583,-20.926315001003,-0.550332019836438));
#24073=CARTESIAN_POINT('Ctrl Pts',(70.7061568471518,-20.9257818388602,-0.000467423370275055));
#24074=CARTESIAN_POINT('Ctrl Pts',(70.4938431528481,-20.9261779264193,-0.000381460781396608));
#24075=CARTESIAN_POINT('Ctrl Pts',(70.4985030872841,-20.926522300612,-0.408752329164892));
#24076=CARTESIAN_POINT('Ctrl Pts',(70.5031630217201,-20.9148124849085,-0.81710346289888));
#24077=CARTESIAN_POINT('Ctrl Pts',(70.507822956156,-20.8909145891097,-1.22474006541663));
#24078=CARTESIAN_POINT('Ctrl Pts',(70.5474412440706,-20.6877371132634,-4.69042493823162));
#24079=CARTESIAN_POINT('Ctrl Pts',(70.5870595319852,-19.6035775169795,-8.10446187133154));
#24080=CARTESIAN_POINT('Ctrl Pts',(70.6266778198998,-17.7700447003034,-11.0524120658346));
#24081=CARTESIAN_POINT('Ctrl Pts',(70.6662961078144,-15.9365118836273,-14.0003622603376));
#24082=CARTESIAN_POINT('Ctrl Pts',(70.7059143957289,-13.3536058465589,-16.4822257162438));
#24083=CARTESIAN_POINT('Ctrl Pts',(70.7455326836435,-10.3348721858182,-18.1967227121314));
#24084=CARTESIAN_POINT('Ctrl Pts',(70.7851509715581,-7.31613852507755,-19.911219708019));
#24085=CARTESIAN_POINT('Ctrl Pts',(70.8247692594727,-3.8615772406645,-20.8583502438879));
#24086=CARTESIAN_POINT('Ctrl Pts',(70.8643875473873,-0.390546384666549,
-20.9231396890874));
#24087=CARTESIAN_POINT('Ctrl Pts',(70.9040058353019,3.0804844713314,-20.9879291342869));
#24088=CARTESIAN_POINT('Ctrl Pts',(70.9436241232164,6.56798489891426,-20.170377488817));
#24089=CARTESIAN_POINT('Ctrl Pts',(70.983242411131,9.64859827329515,-18.5697294569708));
#24090=CARTESIAN_POINT('Ctrl Pts',(71.0228606990455,12.7292116476761,-16.9690814251246));
#24091=CARTESIAN_POINT('Ctrl Pts',(71.0624789869601,15.402937968855,-14.5853370069021));
#24092=CARTESIAN_POINT('Ctrl Pts',(71.1020972748747,17.3452067411371,-11.7078650453502));
#24093=CARTESIAN_POINT('Ctrl Pts',(71.1417155627893,19.2874755134191,-8.83039308379838));
#24094=CARTESIAN_POINT('Ctrl Pts',(71.1813338507039,20.4982867368043,-5.45919357891726));
#24095=CARTESIAN_POINT('Ctrl Pts',(71.2209521386185,20.8306569304741,-2.00350508960085));
#24096=CARTESIAN_POINT('Ctrl Pts',(71.2605704265331,21.1630271241438,1.45218339971558));
#24097=CARTESIAN_POINT('Ctrl Pts',(71.3001887144476,20.6169562880982,4.99236087346727));
#24098=CARTESIAN_POINT('Ctrl Pts',(71.3398070023622,19.2587333621318,8.18727610869908));
#24099=CARTESIAN_POINT('Ctrl Pts',(71.3794252902768,17.9005104361654,11.3821913439309));
#24100=CARTESIAN_POINT('Ctrl Pts',(71.4190435781914,15.7301354202783,14.2318443406428));
#24101=CARTESIAN_POINT('Ctrl Pts',(71.458661866106,13.0110757048767,16.3903084108907));
#24102=CARTESIAN_POINT('Ctrl Pts',(71.4982801540205,10.2920159894752,18.5487724811387));
#24103=CARTESIAN_POINT('Ctrl Pts',(71.5378984419351,7.02427157455919,20.0160476249225));
#24104=CARTESIAN_POINT('Ctrl Pts',(71.5775167298497,3.60452233700019,20.6140175491853));
#24105=CARTESIAN_POINT('Ctrl Pts',(71.6171350177642,0.184773099441191,21.211987473448));
#24106=CARTESIAN_POINT('Ctrl Pts',(71.6567533056788,-3.38698096076084,20.9406521781897));
#24107=CARTESIAN_POINT('Ctrl Pts',(71.6963715935934,-6.67715545615774,19.8329497506961));
#24108=CARTESIAN_POINT('Ctrl Pts',(71.735989881508,-9.96732995155464,18.7252473232025));
#24109=CARTESIAN_POINT('Ctrl Pts',(71.7756081694226,-12.9759248821464,16.7811777634736));
#24110=CARTESIAN_POINT('Ctrl Pts',(71.8152264573371,-15.3377191917709,14.236736662324));
#24111=CARTESIAN_POINT('Ctrl Pts',(71.8548447452517,-17.6995135013954,11.6922955611743));
#24112=CARTESIAN_POINT('Ctrl Pts',(71.8944630331663,-19.4145071900526,8.54748291860389));
#24113=CARTESIAN_POINT('Ctrl Pts',(71.9340813210809,-20.2745127746554,5.18405560817734));
#24114=CARTESIAN_POINT('Ctrl Pts',(71.95400193167,-20.706935205232,3.49287890109326));
#24115=CARTESIAN_POINT('Ctrl Pts',(71.9739225422591,-20.9231983203047,1.74643172095956));
#24116=CARTESIAN_POINT('Ctrl Pts',(71.9938431528481,-20.923224691771,-9.04407733959185E-6));
#24117=CARTESIAN_POINT('Origin',(80.4,0.,0.));
#24118=CARTESIAN_POINT('',(73.7061568471518,-20.9264624460885,0.000284169623841063));
#24119=CARTESIAN_POINT('',(73.4938431528481,-20.9261267613403,0.000395174936093916));
#24120=CARTESIAN_POINT('',(80.4,-20.925,-2.56257342721584E-15));
#24121=CARTESIAN_POINT('Ctrl Pts',(73.7061568471518,-20.9264624460885,0.000284169623841063));
#24122=CARTESIAN_POINT('Ctrl Pts',(73.7028882259227,-20.9266544080345,0.286716760992491));
#24123=CARTESIAN_POINT('Ctrl Pts',(73.6996196046936,-20.9208949345101,0.573141625488209));
#24124=CARTESIAN_POINT('Ctrl Pts',(73.6963509834645,-20.9091336340165,0.859319827974444));
#24125=CARTESIAN_POINT('Ctrl Pts',(73.6567326955499,-20.76657732157,4.32802715938114));
#24126=CARTESIAN_POINT('Ctrl Pts',(73.6171144076354,-19.742270570929,7.76049646925485));
#24127=CARTESIAN_POINT('Ctrl Pts',(73.5774961197208,-17.9605566060624,10.7400515032444));
#24128=CARTESIAN_POINT('Ctrl Pts',(73.5378778318062,-16.1788426411958,13.7196065372339));
#24129=CARTESIAN_POINT('Ctrl Pts',(73.4982595438916,-13.6397214621036,16.2462472953392));
#24130=CARTESIAN_POINT('Ctrl Pts',(73.458641255977,-10.6514235019624,18.0132583747015));
#24131=CARTESIAN_POINT('Ctrl Pts',(73.4190229680625,-7.66312554182124,19.7802694540639));
#24132=CARTESIAN_POINT('Ctrl Pts',(73.3794046801479,-4.22565080063109,20.7876508546832));
#24133=CARTESIAN_POINT('Ctrl Pts',(73.3397863922333,-0.756283154890432,
20.913113964246));
#24134=CARTESIAN_POINT('Ctrl Pts',(73.3001681043188,2.71308449085023,21.0385770738088));
#24135=CARTESIAN_POINT('Ctrl Pts',(73.2605498164042,6.21434504114142,20.2821218923151));
#24136=CARTESIAN_POINT('Ctrl Pts',(73.2209315284896,9.32247149649723,18.7355764546733));
#24137=CARTESIAN_POINT('Ctrl Pts',(73.181313240575,12.430597951853,17.1890310170316));
#24138=CARTESIAN_POINT('Ctrl Pts',(73.1416949526605,15.1455903122734,14.8523953232418));
#24139=CARTESIAN_POINT('Ctrl Pts',(73.1020766647459,17.1378686907431,12.0093195740126));
#24140=CARTESIAN_POINT('Ctrl Pts',(73.0624583768313,19.1301470692127,9.16624382478331));
#24141=CARTESIAN_POINT('Ctrl Pts',(73.0228400889167,20.3997114657316,5.81672802011455));
#24142=CARTESIAN_POINT('Ctrl Pts',(72.9832218010021,20.7924462015731,2.36737847557188));
#24143=CARTESIAN_POINT('Ctrl Pts',(72.9436035130875,21.1851809374146,-1.08197106897078));
#24144=CARTESIAN_POINT('Ctrl Pts',(72.9039852251729,20.7010860125789,-4.63115435338729));
#24145=CARTESIAN_POINT('Ctrl Pts',(72.8643669372584,19.3989269517715,-7.84932691456705));
#24146=CARTESIAN_POINT('Ctrl Pts',(72.8247486493438,18.0967678909641,-11.0674994757468));
#24147=CARTESIAN_POINT('Ctrl Pts',(72.7851303614292,15.9765446941852,-13.9546613136897));
#24148=CARTESIAN_POINT('Ctrl Pts',(72.7455120735146,13.2956366939988,-16.1603324468621));
#24149=CARTESIAN_POINT('Ctrl Pts',(72.7058937856001,10.6147286938125,-18.3660035800345));
#24150=CARTESIAN_POINT('Ctrl Pts',(72.6662754976855,7.37313589021869,-19.8901840084363));
#24151=CARTESIAN_POINT('Ctrl Pts',(72.6266572097709,3.96436354884304,-20.5478495601004));
#24152=CARTESIAN_POINT('Ctrl Pts',(72.5870389218563,0.555591207467407,-21.2055151117644));
#24153=CARTESIAN_POINT('Ctrl Pts',(72.5474206339417,-3.02036067169011,-20.9966657866908));
#24154=CARTESIAN_POINT('Ctrl Pts',(72.5078023460271,-6.32939811713748,-19.9466543401817));
#24155=CARTESIAN_POINT('Ctrl Pts',(72.4681840581126,-9.63843556258485,-18.8966428936726));
#24156=CARTESIAN_POINT('Ctrl Pts',(72.428565770198,-12.6805585743221,-17.0054693257279));
#24157=CARTESIAN_POINT('Ctrl Pts',(72.3889474822835,-15.0864760364287,-14.5027080469193));
#24158=CARTESIAN_POINT('Ctrl Pts',(72.3493291943689,-17.4923934985352,-11.9999467681106));
#24159=CARTESIAN_POINT('Ctrl Pts',(72.3097109064543,-19.2621054110111,-8.88559777843788));
#24160=CARTESIAN_POINT('Ctrl Pts',(72.2700926185397,-20.1807819052104,-5.53771989055453));
#24161=CARTESIAN_POINT('Ctrl Pts',(72.2487806947437,-20.6749669007791,-3.73679102208467));
#24162=CARTESIAN_POINT('Ctrl Pts',(72.2274687709478,-20.9228875520371,-1.86828583450939));
#24163=CARTESIAN_POINT('Ctrl Pts',(72.2061568471519,-20.9232657042053,0.000120932580692235));
#24164=CARTESIAN_POINT('Ctrl Pts',(71.9938431528481,-20.923224691771,-9.04407733959185E-6));
#24165=CARTESIAN_POINT('Ctrl Pts',(72.0135408301736,-20.923250768112,-1.72690524055486));
#24166=CARTESIAN_POINT('Ctrl Pts',(72.0332385074991,-20.7118528671994,-3.45379516471595));
#24167=CARTESIAN_POINT('Ctrl Pts',(72.0529361848246,-20.2889561314617,-5.12723706239442));
#24168=CARTESIAN_POINT('Ctrl Pts',(72.0925544727392,-19.4383764231168,-8.49306044425692));
#24169=CARTESIAN_POINT('Ctrl Pts',(72.1321727606538,-17.7321995258788,-11.6426652296992));
#24170=CARTESIAN_POINT('Ctrl Pts',(72.1717910485684,-15.3775426299187,-14.193712814598));
#24171=CARTESIAN_POINT('Ctrl Pts',(72.211409336483,-13.0228857339585,-16.7447603994967));
#24172=CARTESIAN_POINT('Ctrl Pts',(72.2510276243975,-10.0197488392763,-18.6972507838519));
#24173=CARTESIAN_POINT('Ctrl Pts',(72.2906459123121,-6.73269043703646,-19.814166151453));
#24174=CARTESIAN_POINT('Ctrl Pts',(72.3302642002267,-3.4456320347966,-20.9310815190541));
#24175=CARTESIAN_POINT('Ctrl Pts',(72.3698824881413,0.125347875000815,-21.2124218699011));
#24176=CARTESIAN_POINT('Ctrl Pts',(72.4095007760559,3.54675888097773,-20.6240345771262));
#24177=CARTESIAN_POINT('Ctrl Pts',(72.4491190639704,6.96816988695464,-20.0356472843512));
#24178=CARTESIAN_POINT('Ctrl Pts',(72.488737351885,10.240011989111,-18.5775323479543));
#24179=CARTESIAN_POINT('Ctrl Pts',(72.5283556397996,12.965107881875,-16.4266940803577));
#24180=CARTESIAN_POINT('Ctrl Pts',(72.5679739277141,15.6902037746389,-14.2758558127611));
#24181=CARTESIAN_POINT('Ctrl Pts',(72.6075922156288,17.8685534580103,-11.4322942139648));
#24182=CARTESIAN_POINT('Ctrl Pts',(72.6472105035433,19.2357214761139,-8.24119652063211));
#24183=CARTESIAN_POINT('Ctrl Pts',(72.6868287914579,20.6028894942175,-5.05009882729935));
#24184=CARTESIAN_POINT('Ctrl Pts',(72.7264470793725,21.1588758470531,-1.51146503943013));
#24185=CARTESIAN_POINT('Ctrl Pts',(72.766065367287,20.8361879250575,1.94514101031227));
#24186=CARTESIAN_POINT('Ctrl Pts',(72.8056836552016,20.5135000030618,5.40174706005465));
#24187=CARTESIAN_POINT('Ctrl Pts',(72.8453019431162,19.3121378062348,8.77632537167022));
#24188=CARTESIAN_POINT('Ctrl Pts',(72.8849202310308,17.377937773333,11.6592272275857));
#24189=CARTESIAN_POINT('Ctrl Pts',(72.9245385189454,15.4437377404312,14.5421290835011));
#24190=CARTESIAN_POINT('Ctrl Pts',(72.9641568068599,12.7766998714546,16.9333544837164));
#24191=CARTESIAN_POINT('Ctrl Pts',(73.0037750947745,9.70058273469135,18.542626443029));
#24192=CARTESIAN_POINT('Ctrl Pts',(73.0433933826891,6.62446559792813,20.1518984023415));
#24193=CARTESIAN_POINT('Ctrl Pts',(73.0830116706037,3.13926919337822,20.9792169207512));
#24194=CARTESIAN_POINT('Ctrl Pts',(73.1226299585183,-0.331929547330916,
20.9241516811057));
#24195=CARTESIAN_POINT('Ctrl Pts',(73.1622482464329,-3.80312828804008,20.8690864414602));
#24196=CARTESIAN_POINT('Ctrl Pts',(73.2018665343474,-7.26032936490853,19.9316374437595));
#24197=CARTESIAN_POINT('Ctrl Pts',(73.241484822262,-10.2838542709487,18.2256040265391));
#24198=CARTESIAN_POINT('Ctrl Pts',(73.2811031101765,-13.307379176989,16.5195706093187));
#24199=CARTESIAN_POINT('Ctrl Pts',(73.3207213980912,-15.8972279122009,14.0449527725788));
#24200=CARTESIAN_POINT('Ctrl Pts',(73.3603396860057,-17.7390120952464,11.1021507233064));
#24201=CARTESIAN_POINT('Ctrl Pts',(73.3999579739203,-19.5807962782918,8.15934867403405));
#24202=CARTESIAN_POINT('Ctrl Pts',(73.4395762618349,-20.6745159091708,4.7483624122293));
#24203=CARTESIAN_POINT('Ctrl Pts',(73.4791945497495,-20.8874015563273,1.28326030993092));
#24204=CARTESIAN_POINT('Ctrl Pts',(73.484077417449,-20.913639248689,0.856194022577959));
#24205=CARTESIAN_POINT('Ctrl Pts',(73.4889602851486,-20.9264970502493,0.428305714220112));
#24206=CARTESIAN_POINT('Ctrl Pts',(73.4938431528481,-20.9261267613403,0.000395174936093916));
#24207=CARTESIAN_POINT('Origin',(80.4,0.,0.));
#24208=CARTESIAN_POINT('',(75.2061568471518,-20.9243088587828,-0.000506040078050995));
#24209=CARTESIAN_POINT('',(74.9938431528481,-20.9247245309142,-0.000535895639339255));
#24210=CARTESIAN_POINT('',(80.4,-20.925,-2.56257342721584E-15));
#24211=CARTESIAN_POINT('Ctrl Pts',(75.2061568471518,-20.9243088587828,-0.000506040078050995));
#24212=CARTESIAN_POINT('Ctrl Pts',(75.1783076808977,-20.9220942780769,2.44066904141215));
#24213=CARTESIAN_POINT('Ctrl Pts',(75.1504585146435,-20.4950188134656,4.88259874686084));
#24214=CARTESIAN_POINT('Ctrl Pts',(75.1226093483894,-19.6583159988833,7.17501999857562));
#24215=CARTESIAN_POINT('Ctrl Pts',(75.0829910604748,-18.4680206519944,10.436223739581));
#24216=CARTESIAN_POINT('Ctrl Pts',(75.0433727725602,-16.4487225807659,13.3948526757888));
#24217=CARTESIAN_POINT('Ctrl Pts',(75.0037544846456,-13.8455495578827,15.6917512512826));
#24218=CARTESIAN_POINT('Ctrl Pts',(74.9641361967311,-11.2423765349993,17.9886498267764));
#24219=CARTESIAN_POINT('Ctrl Pts',(74.9245179088165,-8.05532856046113,19.6238180415562));
#24220=CARTESIAN_POINT('Ctrl Pts',(74.8848996209019,-4.67128956317847,20.3987586315651));
#24221=CARTESIAN_POINT('Ctrl Pts',(74.8452813329873,-1.2872505658958,21.1736992215741));
#24222=CARTESIAN_POINT('Ctrl Pts',(74.8056630450727,2.29377945413133,21.0884121868122));
#24223=CARTESIAN_POINT('Ctrl Pts',(74.7660447571582,5.63709007686453,20.153250739204));
#24224=CARTESIAN_POINT('Ctrl Pts',(74.7264264692436,8.98040069959767,19.2180892915959));
#24225=CARTESIAN_POINT('Ctrl Pts',(74.686808181329,12.0859919250369,17.4330534311413));
#24226=CARTESIAN_POINT('Ctrl Pts',(74.6471898934144,14.5768680679944,15.0148332398398));
#24227=CARTESIAN_POINT('Ctrl Pts',(74.6075716054999,17.0677442109518,12.5966130485383));
#24228=CARTESIAN_POINT('Ctrl Pts',(74.5679533175852,18.9439052714275,9.54520852638985));
#24229=CARTESIAN_POINT('Ctrl Pts',(74.5283350296707,19.9775992456411,6.23103749567228));
#24230=CARTESIAN_POINT('Ctrl Pts',(74.4887167417561,21.0112932198546,2.91686646495466));
#24231=CARTESIAN_POINT('Ctrl Pts',(74.4490984538415,21.2025201078059,-0.660071074332059));
#24232=CARTESIAN_POINT('Ctrl Pts',(74.409480165927,20.5280663870395,-4.06556149888438));
#24233=CARTESIAN_POINT('Ctrl Pts',(74.3698618780124,19.8536126662731,-7.47105192343671));
#24234=CARTESIAN_POINT('Ctrl Pts',(74.3302435900978,18.3134783367888,-10.7050952332546));
#24235=CARTESIAN_POINT('Ctrl Pts',(74.2906253021832,16.0946242555306,-13.3751026151278));
#24236=CARTESIAN_POINT('Ctrl Pts',(74.2510070142686,13.8757701742724,-16.0451099970009));
#24237=CARTESIAN_POINT('Ctrl Pts',(74.211388726354,10.9781963412402,-18.1510814509292));
#24238=CARTESIAN_POINT('Ctrl Pts',(74.1717704384395,7.75364667676002,-19.4373676999711));
#24239=CARTESIAN_POINT('Ctrl Pts',(74.1321521505249,4.52909701227992,-20.723653949013));
#24240=CARTESIAN_POINT('Ctrl Pts',(74.0925338626103,0.977571516351926,-21.1902549931685));
#24241=CARTESIAN_POINT('Ctrl Pts',(74.0529155746958,-2.46980102084973,-20.7805289347822));
#24242=CARTESIAN_POINT('Ctrl Pts',(74.0132972867812,-5.91717355805138,-20.370802876396));
#24243=CARTESIAN_POINT('Ctrl Pts',(73.9736789988666,-9.2603931365267,-19.084749715468));
#24244=CARTESIAN_POINT('Ctrl Pts',(73.934060710952,-12.0936177557586,-17.0784867441326));
#24245=CARTESIAN_POINT('Ctrl Pts',(73.8944424230374,-14.9268423749905,-15.0722237727972));
#24246=CARTESIAN_POINT('Ctrl Pts',(73.8548241351229,-17.2500720349789,-12.3457509910545));
#24247=CARTESIAN_POINT('Ctrl Pts',(73.8152058472083,-18.7812839278471,-9.23004192371327));
#24248=CARTESIAN_POINT('Ctrl Pts',(73.7788561805228,-20.1861664924497,-6.37138769991231));
#24249=CARTESIAN_POINT('Ctrl Pts',(73.7425065138373,-20.9243276766347,-3.18507396591327));
#24250=CARTESIAN_POINT('Ctrl Pts',(73.7061568471518,-20.9264624460885,0.000284169623841063));
#24251=CARTESIAN_POINT('Ctrl Pts',(73.4938431528481,-20.9261267613403,0.000395174936093916));
#24252=CARTESIAN_POINT('Ctrl Pts',(73.5285785730632,-20.9234926246723,-3.04364642337207));
#24253=CARTESIAN_POINT('Ctrl Pts',(73.5633139932782,-20.2514482408018,-6.08881302228566));
#24254=CARTESIAN_POINT('Ctrl Pts',(73.5980494134932,-18.9646405085985,-8.84718662502006));
#24255=CARTESIAN_POINT('Ctrl Pts',(73.6376677014078,-17.4969421502789,-11.9933135148807));
#24256=CARTESIAN_POINT('Ctrl Pts',(73.6772859893224,-15.2294937702056,-14.7663493518099));
#24257=CARTESIAN_POINT('Ctrl Pts',(73.7169042772369,-12.4375467435986,-16.8296682022881));
#24258=CARTESIAN_POINT('Ctrl Pts',(73.7565225651515,-9.64559971699171,-18.8929870527663));
#24259=CARTESIAN_POINT('Ctrl Pts',(73.7961408530661,-6.32915404385119,-20.2465889167936));
#24260=CARTESIAN_POINT('Ctrl Pts',(73.8357591409807,-2.89080157164628,-20.7261565918932));
#24261=CARTESIAN_POINT('Ctrl Pts',(73.8753774288953,0.547550900558613,-21.2057242669927));
#24262=CARTESIAN_POINT('Ctrl Pts',(73.9149957168098,4.10781017182792,-20.8112577531646));
#24263=CARTESIAN_POINT('Ctrl Pts',(73.9546140047244,7.35778723659513,-19.5906423523913));
#24264=CARTESIAN_POINT('Ctrl Pts',(73.994232292639,10.6077643013624,-18.3700269516179));
#24265=CARTESIAN_POINT('Ctrl Pts',(74.0338505805536,13.5474591596276,-16.3232626638993));
#24266=CARTESIAN_POINT('Ctrl Pts',(74.0734688684682,15.8200147117645,-13.6988114563952));
#24267=CARTESIAN_POINT('Ctrl Pts',(74.1130871563828,18.0925702639014,-11.0743602488911));
#24268=CARTESIAN_POINT('Ctrl Pts',(74.1527054442973,19.6979865099099,-7.87222212160154));
#24269=CARTESIAN_POINT('Ctrl Pts',(74.1923237322119,20.4413778535412,-4.48111283578782));
#24270=CARTESIAN_POINT('Ctrl Pts',(74.2319420201265,21.1847691971725,-1.09000354997409));
#24271=CARTESIAN_POINT('Ctrl Pts',(74.2715603080411,21.0661356384265,2.49007689436369));
#24272=CARTESIAN_POINT('Ctrl Pts',(74.3111785959557,20.0998784093131,5.82453334861588));
#24273=CARTESIAN_POINT('Ctrl Pts',(74.3507968838702,19.1336211801997,9.15898980286805));
#24274=CARTESIAN_POINT('Ctrl Pts',(74.3904151717848,17.3197402807189,12.2478222670347));
#24275=CARTESIAN_POINT('Ctrl Pts',(74.4300334596993,14.8784273661496,14.7160694449476));
#24276=CARTESIAN_POINT('Ctrl Pts',(74.4696517476139,12.4371144515803,17.1843166228605));
#24277=CARTESIAN_POINT('Ctrl Pts',(74.5092700355286,9.36836952192247,19.0319785145197));
#24278=CARTESIAN_POINT('Ctrl Pts',(74.5488883234432,6.04471539600249,20.0347627033524));
#24279=CARTESIAN_POINT('Ctrl Pts',(74.5885066113577,2.72106127008243,21.037546892185));
#24280=CARTESIAN_POINT('Ctrl Pts',(74.6281248992722,-0.857502052099787,
21.1954533781911));
#24281=CARTESIAN_POINT('Ctrl Pts',(74.6677431871868,-4.25656358928468,20.4893134879792));
#24282=CARTESIAN_POINT('Ctrl Pts',(74.7073614751014,-7.65562512646958,19.7831735977672));
#24283=CARTESIAN_POINT('Ctrl Pts',(74.746979763016,-10.8751848786571,18.2129873313374));
#24284=CARTESIAN_POINT('Ctrl Pts',(74.7865980509306,-13.5244122288502,15.9693636273471));
#24285=CARTESIAN_POINT('Ctrl Pts',(74.8262163388453,-16.1736395790433,13.7257399233568));
#24286=CARTESIAN_POINT('Ctrl Pts',(74.8658346267597,-18.252534527242,10.8086787818062));
#24287=CARTESIAN_POINT('Ctrl Pts',(74.9054529146743,-19.5087346829906,7.57228973739029));
#24288=CARTESIAN_POINT('Ctrl Pts',(74.9349163273989,-20.4429482899325,5.1654450408548));
#24289=CARTESIAN_POINT('Ctrl Pts',(74.9643797401235,-20.9221597565615,2.58199186132092));
#24290=CARTESIAN_POINT('Ctrl Pts',(74.9938431528481,-20.9247245309142,-0.000535895639339255));
#24291=CARTESIAN_POINT('Origin',(80.4,0.,0.));
#24292=CARTESIAN_POINT('',(76.7061568471518,-20.9240642695764,0.000470086318913876));
#24293=CARTESIAN_POINT('',(76.4938431528481,-20.9237353903355,0.000391611568432831));
#24294=CARTESIAN_POINT('',(80.4,-20.925,-2.56257342721584E-15));
#24295=CARTESIAN_POINT('Ctrl Pts',(76.7061568471518,-20.9240642695764,0.000470086318913876));
#24296=CARTESIAN_POINT('Ctrl Pts',(76.6933454237872,-20.9249940480266,1.1235190201765));
#24297=CARTESIAN_POINT('Ctrl Pts',(76.6805340004226,-20.8361268006114,2.24642227573881));
#24298=CARTESIAN_POINT('Ctrl Pts',(76.667722577058,-20.6561712045076,3.35453291263967));
#24299=CARTESIAN_POINT('Ctrl Pts',(76.6281042891434,-20.0996731156252,6.78127520383157));
#24300=CARTESIAN_POINT('Ctrl Pts',(76.5884860012288,-18.6720921626798,10.0665548731172));
#24301=CARTESIAN_POINT('Ctrl Pts',(76.5488677133143,-16.54672605952,12.8115633941809));
#24302=CARTESIAN_POINT('Ctrl Pts',(76.5092494253997,-14.4213599563602,15.5565719152446));
#24303=CARTESIAN_POINT('Ctrl Pts',(76.469631137485,-11.598208702986,17.7613092880865));
#24304=CARTESIAN_POINT('Ctrl Pts',(76.4300128495705,-8.41998187187309,19.1581367875178));
#24305=CARTESIAN_POINT('Ctrl Pts',(76.3903945616559,-5.24175504076021,20.554964286949));
#24306=CARTESIAN_POINT('Ctrl Pts',(76.3507762737414,-1.70845263190867,21.1438819129698));
#24307=CARTESIAN_POINT('Ctrl Pts',(76.3111579858268,1.7510087117926,20.8533994442906));
#24308=CARTESIAN_POINT('Ctrl Pts',(76.2715396979122,5.21047005549381,20.5629169756114));
#24309=CARTESIAN_POINT('Ctrl Pts',(76.2319214099976,8.59609033404474,19.3930344122323));
#24310=CARTESIAN_POINT('Ctrl Pts',(76.192303122083,11.4968804171816,17.4857667994554));
#24311=CARTESIAN_POINT('Ctrl Pts',(76.1526848341684,14.3976705003185,15.5784991866785));
#24312=CARTESIAN_POINT('Ctrl Pts',(76.1130665462539,16.8136303880413,12.9338465245038));
#24313=CARTESIAN_POINT('Ctrl Pts',(76.0734482583393,18.4514805122609,9.87284998354419));
#24314=CARTESIAN_POINT('Ctrl Pts',(76.0338299704247,20.0893306364805,6.81185344258452));
#24315=CARTESIAN_POINT('Ctrl Pts',(75.9942116825101,20.9490709971969,3.33451302283995));
#24316=CARTESIAN_POINT('Ctrl Pts',(75.9545933945955,20.9263355066529,-0.137048002209587));
#24317=CARTESIAN_POINT('Ctrl Pts',(75.9149751066809,20.9036000161089,-3.60860902725913));
#24318=CARTESIAN_POINT('Ctrl Pts',(75.8753568187664,19.9983886743046,-7.07439065761364));
#24319=CARTESIAN_POINT('Ctrl Pts',(75.8357385308518,18.3205874080315,-10.1136727708874));
#24320=CARTESIAN_POINT('Ctrl Pts',(75.7961202429372,16.6427861417585,-13.1529548841611));
#24321=CARTESIAN_POINT('Ctrl Pts',(75.7565019550227,14.1923949510166,-15.7657374803541));
#24322=CARTESIAN_POINT('Ctrl Pts',(75.7168836671081,11.2668731080905,-17.6348481779147));
#24323=CARTESIAN_POINT('Ctrl Pts',(75.6772653791935,8.34135126516437,-19.5039588754752));
#24324=CARTESIAN_POINT('Ctrl Pts',(75.6376470912789,4.94069877005392,-20.6293976744032));
#24325=CARTESIAN_POINT('Ctrl Pts',(75.5980288033643,1.47772955235106,-20.8745446719688));
#24326=CARTESIAN_POINT('Ctrl Pts',(75.5584105154498,-1.98523966535179,-21.1196916695344));
#24327=CARTESIAN_POINT('Ctrl Pts',(75.5187922275352,-5.51052560564705,-20.4845468657374));
#24328=CARTESIAN_POINT('Ctrl Pts',(75.4791739396206,-8.67018476532732,-19.0462121175576));
#24329=CARTESIAN_POINT('Ctrl Pts',(75.439555651706,-11.8298439250076,-17.6078773693778));
#24330=CARTESIAN_POINT('Ctrl Pts',(75.3999373637915,-14.6238763040729,-15.366352676815));
#24331=CARTESIAN_POINT('Ctrl Pts',(75.3603190758769,-16.7131071448944,-12.5937424721642));
#24332=CARTESIAN_POINT('Ctrl Pts',(75.3207007879623,-18.8023379857158,-9.82113226751339));
#24333=CARTESIAN_POINT('Ctrl Pts',(75.2810825000477,-20.1867672882934,-6.51743655077455));
#24334=CARTESIAN_POINT('Ctrl Pts',(75.2414642121331,-20.6983356283075,-3.08369941950365));
#24335=CARTESIAN_POINT('Ctrl Pts',(75.2296950904727,-20.8503035791748,-2.06366366896917));
#24336=CARTESIAN_POINT('Ctrl Pts',(75.2179259688123,-20.9252447456786,-1.03215223968963));
#24337=CARTESIAN_POINT('Ctrl Pts',(75.2061568471518,-20.9243088587828,-0.000506040078050995));
#24338=CARTESIAN_POINT('Ctrl Pts',(74.9938431528481,-20.9247245309142,-0.000535895639339255));
#24339=CARTESIAN_POINT('Ctrl Pts',(75.0039980280381,-20.9256085073797,-0.890631258715375));
#24340=CARTESIAN_POINT('Ctrl Pts',(75.0141529032281,-20.8698712062196,-1.78061669003418));
#24341=CARTESIAN_POINT('Ctrl Pts',(75.024307778418,-20.7566264448263,-2.66322350324698));
#24342=CARTESIAN_POINT('Ctrl Pts',(75.0639260663326,-20.3148126876145,-6.10663075218757));
#24343=CARTESIAN_POINT('Ctrl Pts',(75.1035443542472,-18.9976798098923,-9.43772830278766));
#24344=CARTESIAN_POINT('Ctrl Pts',(75.1431626421618,-16.9651179503399,-12.2521456785888));
#24345=CARTESIAN_POINT('Ctrl Pts',(75.1827809300764,-14.9325560907876,-15.0665630543899));
#24346=CARTESIAN_POINT('Ctrl Pts',(75.222399217991,-12.1845652494053,-17.3643002553922));
#24347=CARTESIAN_POINT('Ctrl Pts',(75.2620175059056,-9.05473108345861,-18.8664290687071));
#24348=CARTESIAN_POINT('Ctrl Pts',(75.3016357938201,-5.92489691751194,-20.3685578820221));
#24349=CARTESIAN_POINT('Ctrl Pts',(75.3412540817347,-2.41321942700093,-21.0750783076498));
#24350=CARTESIAN_POINT('Ctrl Pts',(75.3808723696492,1.05400984949412,-20.9002240187869));
#24351=CARTESIAN_POINT('Ctrl Pts',(75.4204906575638,4.52123912598912,-20.7253697299241));
#24352=CARTESIAN_POINT('Ctrl Pts',(75.4601089454784,7.94402018846819,-19.6691407265706));
#24353=CARTESIAN_POINT('Ctrl Pts',(75.499727233393,10.9068528637832,-17.8597553568377));
#24354=CARTESIAN_POINT('Ctrl Pts',(75.5393455213076,13.8696855390983,-16.0503699871048));
#24355=CARTESIAN_POINT('Ctrl Pts',(75.5789638092222,16.3725698272493,-13.4878282509926));
#24356=CARTESIAN_POINT('Ctrl Pts',(75.6185820971367,18.1116741842043,-10.4832036631717));
#24357=CARTESIAN_POINT('Ctrl Pts',(75.6582003850513,19.8507785411594,-7.47857907535073));
#24358=CARTESIAN_POINT('Ctrl Pts',(75.6978186729659,20.8261029669184,-4.03187163582119));
#24359=CARTESIAN_POINT('Ctrl Pts',(75.7374369608805,20.9192503275774,-0.561486002016126));
#24360=CARTESIAN_POINT('Ctrl Pts',(75.7770552487951,21.0123976882365,2.90889963178892));
#24361=CARTESIAN_POINT('Ctrl Pts',(75.8166735367096,20.2233679837955,6.40296345986942));
#24362=CARTESIAN_POINT('Ctrl Pts',(75.8562918246242,18.6479435540623,9.49655211130938));
#24363=CARTESIAN_POINT('Ctrl Pts',(75.8959101125388,17.0725191243292,12.5901407627493));
#24364=CARTESIAN_POINT('Ctrl Pts',(75.9355284004534,14.7106999693039,15.2832542375487));
#24365=CARTESIAN_POINT('Ctrl Pts',(75.9751466883679,11.8491933746539,17.2489685827404));
#24366=CARTESIAN_POINT('Ctrl Pts',(76.0147649762825,8.98768678000398,19.2146829279322));
#24367=CARTESIAN_POINT('Ctrl Pts',(76.0543832641971,5.62649274572937,20.4529981435163));
#24368=CARTESIAN_POINT('Ctrl Pts',(76.0940015521117,2.173635237644,20.8135919689991));
#24369=CARTESIAN_POINT('Ctrl Pts',(76.1336198400263,-1.27922227044142,21.1741857944818));
#24370=CARTESIAN_POINT('Ctrl Pts',(76.1732381279408,-4.82374325233762,20.6570582298631));
#24371=CARTESIAN_POINT('Ctrl Pts',(76.2128564158554,-8.02964921379633,19.3249847167259));
#24372=CARTESIAN_POINT('Ctrl Pts',(76.25247470377,-11.235555175255,17.9929112035887));
#24373=CARTESIAN_POINT('Ctrl Pts',(76.2920929916846,-14.1028461162763,15.845891741933));
#24374=CARTESIAN_POINT('Ctrl Pts',(76.3317112795992,-16.2834542344755,13.144558531653));
#24375=CARTESIAN_POINT('Ctrl Pts',(76.3713295675138,-18.4640623526748,10.443225321373));
#24376=CARTESIAN_POINT('Ctrl Pts',(76.4109478554283,-19.9579876480521,7.18757836246868));
#24377=CARTESIAN_POINT('Ctrl Pts',(76.4505661433429,-20.5838786968473,3.77282899052993));
#24378=CARTESIAN_POINT('Ctrl Pts',(76.464991813178,-20.8117759154783,2.52946261600763));
#24379=CARTESIAN_POINT('Ctrl Pts',(76.4794174830131,-20.9245884769033,1.2650023195153));
#24380=CARTESIAN_POINT('Ctrl Pts',(76.4938431528481,-20.9237353903355,0.000391611568432831));
#24381=CARTESIAN_POINT('Origin',(80.4,0.,0.));
#24382=CARTESIAN_POINT('',(78.2061568471519,-20.9266265721997,-0.000199885376053199));
#24383=CARTESIAN_POINT('',(77.9938431528481,-20.9267713605918,-5.6450652404226E-5));
#24384=CARTESIAN_POINT('',(80.4,-20.925,-2.56257342721584E-15));
#24385=CARTESIAN_POINT('Ctrl Pts',(78.2061568471519,-20.9266265721997,-0.000199885376053199));
#24386=CARTESIAN_POINT('Ctrl Pts',(78.1687648787622,-20.9249937207778,3.27642156312699));
#24387=CARTESIAN_POINT('Ctrl Pts',(78.1313729103724,-20.1423394509286,6.55379572127686));
#24388=CARTESIAN_POINT('Ctrl Pts',(78.0939809419828,-18.6587817608754,9.47523947412083));
#24389=CARTESIAN_POINT('Ctrl Pts',(78.0543626540682,-17.0868929774374,12.5706261229379));
#24390=CARTESIAN_POINT('Ctrl Pts',(78.0147443661537,-14.7281524151643,15.2664363615343));
#24391=CARTESIAN_POINT('Ctrl Pts',(77.9751260782391,-11.8688936414524,17.2354188698681));
#24392=CARTESIAN_POINT('Ctrl Pts',(77.9355077903245,-9.00963486774041,19.2044013782019));
#24393=CARTESIAN_POINT('Ctrl Pts',(77.8958895024099,-5.64985788258961,20.446556156273));
#24394=CARTESIAN_POINT('Ctrl Pts',(77.8562712144953,-2.19741463258577,20.8110948492483));
#24395=CARTESIAN_POINT('Ctrl Pts',(77.8166529265807,1.25502861741808,21.1756335422237));
#24396=CARTESIAN_POINT('Ctrl Pts',(77.7770346386661,4.80013813227497,20.6625561501032));
#24397=CARTESIAN_POINT('Ctrl Pts',(77.7374163507516,8.00756397421087,19.3341464536408));
#24398=CARTESIAN_POINT('Ctrl Pts',(77.697798062837,11.2149898161467,18.0057367571785));
#24399=CARTESIAN_POINT('Ctrl Pts',(77.6581797749224,14.0847319851616,15.8619947563745));
#24400=CARTESIAN_POINT('Ctrl Pts',(77.6185614870079,16.2684251180171,13.1631547917429));
#24401=CARTESIAN_POINT('Ctrl Pts',(77.5789431990933,18.4521182508726,10.4643148271113));
#24402=CARTESIAN_POINT('Ctrl Pts',(77.5393249111787,19.9497623475687,7.21037689865213));
#24403=CARTESIAN_POINT('Ctrl Pts',(77.4997066232641,20.5795545495139,3.79634487836558));
#24404=CARTESIAN_POINT('Ctrl Pts',(77.4600883353496,21.2093467514592,0.382312858078985));
#24405=CARTESIAN_POINT('Ctrl Pts',(77.420470047435,20.9712870586536,-3.19181325403503));
#24406=CARTESIAN_POINT('Ctrl Pts',(77.3808517595204,19.8942741478675,-6.49216112102925));
#24407=CARTESIAN_POINT('Ctrl Pts',(77.3412334716058,18.8172612370814,-9.79250898802348));
#24408=CARTESIAN_POINT('Ctrl Pts',(77.3016151836912,16.9012951083147,-12.8190786098979));
#24409=CARTESIAN_POINT('Ctrl Pts',(77.2619968957766,14.3789598046942,-15.2044669366243));
#24410=CARTESIAN_POINT('Ctrl Pts',(77.2223786078621,11.8566245010736,-17.5898552633507));
#24411=CARTESIAN_POINT('Ctrl Pts',(77.1827603199475,8.72792002259909,-19.3340622949291));
#24412=CARTESIAN_POINT('Ctrl Pts',(77.1431420320329,5.37264783153356,-20.2253542656298));
#24413=CARTESIAN_POINT('Ctrl Pts',(77.1035237441183,2.01737564046811,-21.1166462363305));
#24414=CARTESIAN_POINT('Ctrl Pts',(77.0639054562038,-1.56446426318834,-21.1550231461535));
#24415=CARTESIAN_POINT('Ctrl Pts',(77.0242871682892,-4.93806314554617,-20.3358263235727));
#24416=CARTESIAN_POINT('Ctrl Pts',(76.9846688803746,-8.31166202790415,-19.5166295009918));
#24417=CARTESIAN_POINT('Ctrl Pts',(76.94505059246,-11.4770198889634,-17.839858946007));
#24418=CARTESIAN_POINT('Ctrl Pts',(76.9054323045454,-14.0498858183275,-15.509062137469));
#24419=CARTESIAN_POINT('Ctrl Pts',(76.8658140166308,-16.6227517476915,-13.178265328931));
#24420=CARTESIAN_POINT('Ctrl Pts',(76.8261957287163,-18.6031257453604,-10.1934422668398));
#24421=CARTESIAN_POINT('Ctrl Pts',(76.7865774408017,-19.750605131785,-6.91692827924511));
#24422=CARTESIAN_POINT('Ctrl Pts',(76.7597705762517,-20.5270224406819,-4.69994538359761));
#24423=CARTESIAN_POINT('Ctrl Pts',(76.7329637117018,-20.9221187835623,-2.34941874305164));
#24424=CARTESIAN_POINT('Ctrl Pts',(76.7061568471518,-20.9240642695764,0.000470086318913876));
#24425=CARTESIAN_POINT('Ctrl Pts',(76.4938431528481,-20.9237353903355,0.000391611568432831));
#24426=CARTESIAN_POINT('Ctrl Pts',(76.5190357709276,-20.9222455819358,-2.20809194231692));
#24427=CARTESIAN_POINT('Ctrl Pts',(76.5442283890071,-20.5740956707248,-4.41703422450956));
#24428=CARTESIAN_POINT('Ctrl Pts',(76.5694210070866,-19.886843487402,-6.51488732871773));
#24429=CARTESIAN_POINT('Ctrl Pts',(76.6090392950012,-18.8060604269481,-9.81400249105353));
#24430=CARTESIAN_POINT('Ctrl Pts',(76.6486575829158,-16.886637503827,-12.8383810307519));
#24431=CARTESIAN_POINT('Ctrl Pts',(76.6882758708304,-14.3615783902992,-15.2208858788705));
#24432=CARTESIAN_POINT('Ctrl Pts',(76.7278941587449,-11.8365192767715,-17.603390726989));
#24433=CARTESIAN_POINT('Ctrl Pts',(76.7675124466595,-8.70582397283707,-19.3440218835278));
#24434=CARTESIAN_POINT('Ctrl Pts',(76.8071307345741,-5.34953561216826,-20.2314796674008));
#24435=CARTESIAN_POINT('Ctrl Pts',(76.8467490224887,-1.99324725149935,-21.1189374512739));
#24436=CARTESIAN_POINT('Ctrl Pts',(76.8863673104033,1.58863416590386,-21.1532218624812));
#24437=CARTESIAN_POINT('Ctrl Pts',(76.9259855983179,4.96129486669173,-20.3301710284013));
#24438=CARTESIAN_POINT('Ctrl Pts',(76.9656038862325,8.33395556747946,-19.5071201943215));
#24439=CARTESIAN_POINT('Ctrl Pts',(77.005222174147,11.4973955516517,-17.8267341149546));
#24440=CARTESIAN_POINT('Ctrl Pts',(77.0448404620616,14.067596724807,-15.4929991669305));
#24441=CARTESIAN_POINT('Ctrl Pts',(77.0844587499761,16.6377978979623,-13.1592642189064));
#24442=CARTESIAN_POINT('Ctrl Pts',(77.1240770378908,18.6147602601005,-10.172180402225));
#24443=CARTESIAN_POINT('Ctrl Pts',(77.1636953258054,19.7584952788611,-6.89435748373493));
#24444=CARTESIAN_POINT('Ctrl Pts',(77.2033136137199,20.9022302976217,-3.61653456524486));
#24445=CARTESIAN_POINT('Ctrl Pts',(77.2429319016344,21.2127379730048,-0.0479725449460383));
#24446=CARTESIAN_POINT('Ctrl Pts',(77.282550189549,20.6523249817942,3.37813167959247));
#24447=CARTESIAN_POINT('Ctrl Pts',(77.3221684774636,20.0919119905837,6.80423590413097));
#24448=CARTESIAN_POINT('Ctrl Pts',(77.3617867653783,18.6605783327797,10.0878823329092));
#24449=CARTESIAN_POINT('Ctrl Pts',(77.4014050532928,16.5320772726997,12.8304607028663));
#24450=CARTESIAN_POINT('Ctrl Pts',(77.4410233412074,14.4035762126197,15.5730390728233));
#24451=CARTESIAN_POINT('Ctrl Pts',(77.4806416291219,11.5779077502638,17.7745493839593));
#24452=CARTESIAN_POINT('Ctrl Pts',(77.5202599170365,8.39808702856311,19.1677446523838));
#24453=CARTESIAN_POINT('Ctrl Pts',(77.5598782049511,5.21826630686235,20.5609399208084));
#24454=CARTESIAN_POINT('Ctrl Pts',(77.5994964928657,1.68429332581686,21.1458201465215));
#24455=CARTESIAN_POINT('Ctrl Pts',(77.6391147807803,-1.77483386920591,20.8513852186139));
#24456=CARTESIAN_POINT('Ctrl Pts',(77.6787330686949,-5.23396106422867,20.5569502907062));
#24457=CARTESIAN_POINT('Ctrl Pts',(77.7183513566094,-8.61824247322863,19.3832002091777));
#24458=CARTESIAN_POINT('Ctrl Pts',(77.7579696445239,-11.5168514947511,17.4726195072793));
#24459=CARTESIAN_POINT('Ctrl Pts',(77.7975879324385,-14.4154605162737,15.5620388053809));
#24460=CARTESIAN_POINT('Ctrl Pts',(77.8372062203532,-16.8283971503188,12.9146274831127));
#24461=CARTESIAN_POINT('Ctrl Pts',(77.8768245082678,-18.4627488293163,9.85176159191279));
#24462=CARTESIAN_POINT('Ctrl Pts',(77.9158307231279,-20.0718509915664,6.83621469858147));
#24463=CARTESIAN_POINT('Ctrl Pts',(77.954836937988,-20.9262394823794,3.41795100344054));
#24464=CARTESIAN_POINT('Ctrl Pts',(77.9938431528481,-20.9267713605918,-5.6450652404226E-5));
#24465=CARTESIAN_POINT('Origin',(80.4,0.,0.));
#24466=CARTESIAN_POINT('',(79.7061568471518,-20.923342133494,-0.000201647965826224));
#24467=CARTESIAN_POINT('',(79.4938431528481,-20.9235342978811,-0.000316448518974899));
#24468=CARTESIAN_POINT('',(80.4,-20.925,-2.56257342721584E-15));
#24469=CARTESIAN_POINT('Ctrl Pts',(79.7061568471518,-20.923342133494,-0.000201647965826224));
#24470=CARTESIAN_POINT('Ctrl Pts',(79.6838026216517,-20.9226777745741,1.95956275646496));
#24471=CARTESIAN_POINT('Ctrl Pts',(79.6614483961515,-20.6495711928031,3.91950855148925));
#24472=CARTESIAN_POINT('Ctrl Pts',(79.6390941706513,-20.1065201583901,5.80156418667976));
#24473=CARTESIAN_POINT('Ctrl Pts',(79.5994758827368,-19.1440733836838,9.13712246964086));
#24474=CARTESIAN_POINT('Ctrl Pts',(79.5598575948222,-17.333722852153,12.2280253855573));
#24475=CARTESIAN_POINT('Ctrl Pts',(79.5202393069077,-14.8952316586553,14.6990603008119));
#24476=CARTESIAN_POINT('Ctrl Pts',(79.4806210189931,-12.4567404651576,17.1700952160665));
#24477=CARTESIAN_POINT('Ctrl Pts',(79.4410027310785,-9.39010860969301,19.0212621306593));
#24478=CARTESIAN_POINT('Ctrl Pts',(79.4013844431639,-6.06760239959109,20.0278431442926));
#24479=CARTESIAN_POINT('Ctrl Pts',(79.3617661552493,-2.74509618948911,21.0344241579259));
#24480=CARTESIAN_POINT('Ctrl Pts',(79.3221478673347,0.833284375250171,21.1964192705997));
#24481=CARTESIAN_POINT('Ctrl Pts',(79.2825295794201,4.23315049876201,20.4941634800434));
#24482=CARTESIAN_POINT('Ctrl Pts',(79.2429112915056,7.63301662227385,19.7919076894871));
#24483=CARTESIAN_POINT('Ctrl Pts',(79.203293003591,10.8543683045582,18.2254009957007));
#24484=CARTESIAN_POINT('Ctrl Pts',(79.1636747156764,13.5061574016271,15.9848056645799));
#24485=CARTESIAN_POINT('Ctrl Pts',(79.1240564277619,16.1579464986958,13.7442103334592));
#24486=CARTESIAN_POINT('Ctrl Pts',(79.0844381398473,18.2401730105491,10.8295263650042));
#24487=CARTESIAN_POINT('Ctrl Pts',(79.0448198519327,19.5000701196733,7.59457472277011));
#24488=CARTESIAN_POINT('Ctrl Pts',(79.0052015640181,20.7599672287975,4.35962308053591));
#24489=CARTESIAN_POINT('Ctrl Pts',(78.9655832761036,21.1975349351925,0.804403764522593));
#24490=CARTESIAN_POINT('Ctrl Pts',(78.925964988189,20.7596557725489,-2.63950603280019));
#24491=CARTESIAN_POINT('Ctrl Pts',(78.8863467002744,20.3217766099053,-6.08341583012296));
#24492=CARTESIAN_POINT('Ctrl Pts',(78.8467284123598,19.008450578223,-9.41601610875521));
#24493=CARTESIAN_POINT('Ctrl Pts',(78.8071101244452,16.9791056933766,-12.2327539722279));
#24494=CARTESIAN_POINT('Ctrl Pts',(78.7674918365306,14.9497608085302,-15.0494918357007));
#24495=CARTESIAN_POINT('Ctrl Pts',(78.727873548616,12.2043970705196,-17.3503672840139));
#24496=CARTESIAN_POINT('Ctrl Pts',(78.6882552607015,9.07628122579333,-18.8560711443881));
#24497=CARTESIAN_POINT('Ctrl Pts',(78.6486369727869,5.94816538106711,-20.3617750047622));
#24498=CARTESIAN_POINT('Ctrl Pts',(78.6090186848723,2.43729742962522,-21.0723072771974));
#24499=CARTESIAN_POINT('Ctrl Pts',(78.5694003969577,-1.03012936197627,-20.9014146265153));
#24500=CARTESIAN_POINT('Ctrl Pts',(78.5297821090432,-4.49755615357775,-20.7305219758331));
#24501=CARTESIAN_POINT('Ctrl Pts',(78.4901638211286,-7.92154178533884,-19.6782044020336));
#24502=CARTESIAN_POINT('Ctrl Pts',(78.450545533214,-10.8864398583564,-17.872205434761));
#24503=CARTESIAN_POINT('Ctrl Pts',(78.4109272452994,-13.851337931374,-16.0662064674884));
#24504=CARTESIAN_POINT('Ctrl Pts',(78.3713089573849,-16.357148445648,-13.5065261067426));
#24505=CARTESIAN_POINT('Ctrl Pts',(78.3316906694703,-18.0996846350513,-10.5038905174988));
#24506=CARTESIAN_POINT('Ctrl Pts',(78.2920723815557,-19.8422208244545,-7.50125492825505));
#24507=CARTESIAN_POINT('Ctrl Pts',(78.2524540936411,-20.8214826889869,-4.05566411051326));
#24508=CARTESIAN_POINT('Ctrl Pts',(78.2128358057265,-20.9185951189516,-0.585387172123522));
#24509=CARTESIAN_POINT('Ctrl Pts',(78.2106094862016,-20.9240522780143,-0.390377601760896));
#24510=CARTESIAN_POINT('Ctrl Pts',(78.2083831666768,-20.9267237922488,-0.195290077752758));
#24511=CARTESIAN_POINT('Ctrl Pts',(78.2061568471519,-20.9266265721997,-0.000199885376053199));
#24512=CARTESIAN_POINT('Ctrl Pts',(77.9938431528481,-20.9267713605918,-5.6450652404226E-5));
#24513=CARTESIAN_POINT('Ctrl Pts',(77.9944552259026,-20.9267797066547,-0.0536907309856513));
#24514=CARTESIAN_POINT('Ctrl Pts',(77.995067298957,-20.9265778086015,-0.107324948224965));
#24515=CARTESIAN_POINT('Ctrl Pts',(77.9956793720115,-20.9261652833693,-0.160957545385623));
#24516=CARTESIAN_POINT('Ctrl Pts',(78.035297659926,-20.8994633344748,-3.63249033135252));
#24517=CARTESIAN_POINT('Ctrl Pts',(78.0749159478406,-19.9902927127358,-7.09723544315468));
#24518=CARTESIAN_POINT('Ctrl Pts',(78.1145342357552,-18.3090199720912,-10.1345985840523));
#24519=CARTESIAN_POINT('Ctrl Pts',(78.1541525236698,-16.6277472314466,-13.1719617249499));
#24520=CARTESIAN_POINT('Ctrl Pts',(78.1937708115843,-14.1743723718966,-15.781942894943));
#24521=CARTESIAN_POINT('Ctrl Pts',(78.2333890994989,-11.2467168609356,-17.6477097847924));
#24522=CARTESIAN_POINT('Ctrl Pts',(78.2730073874135,-8.31906134997462,-19.5134766746417));
#24523=CARTESIAN_POINT('Ctrl Pts',(78.3126256753281,-4.91712518760277,-20.6350292843473));
#24524=CARTESIAN_POINT('Ctrl Pts',(78.3522439632427,-1.45387813107363,-20.8762194656575));
#24525=CARTESIAN_POINT('Ctrl Pts',(78.3918622511573,2.00936892545546,-21.1174096469676));
#24526=CARTESIAN_POINT('Ctrl Pts',(78.4314805390718,5.53392687614181,-20.4782373998824));
#24527=CARTESIAN_POINT('Ctrl Pts',(78.4710988269864,8.6919405903041,-19.0362934830532));
#24528=CARTESIAN_POINT('Ctrl Pts',(78.510717114901,11.8499543044664,-17.594349566224));
#24529=CARTESIAN_POINT('Ctrl Pts',(78.5503354028156,14.6414237821046,-15.3496339796508));
#24530=CARTESIAN_POINT('Ctrl Pts',(78.5899536907302,16.7274853827683,-12.5746385064375));
#24531=CARTESIAN_POINT('Ctrl Pts',(78.6295719786448,18.8135469834321,-9.79964303322422));
#24532=CARTESIAN_POINT('Ctrl Pts',(78.6691902665594,20.1942007071214,-6.49436767337088));
#24533=CARTESIAN_POINT('Ctrl Pts',(78.7088085544739,20.7018454567228,-3.06004828136315));
#24534=CARTESIAN_POINT('Ctrl Pts',(78.7484268423885,21.2094902063242,0.37427111064453));
#24535=CARTESIAN_POINT('Ctrl Pts',(78.788045130303,20.8441259818378,3.9376345348067));
#24536=CARTESIAN_POINT('Ctrl Pts',(78.8276634182176,19.6501052836908,7.19747616447438));
#24537=CARTESIAN_POINT('Ctrl Pts',(78.8672817061322,18.4560845855438,10.4573177941421));
#24538=CARTESIAN_POINT('Ctrl Pts',(78.9068999940468,16.4334074137363,13.4136376293154));
#24539=CARTESIAN_POINT('Ctrl Pts',(78.9465182819614,13.8276117386402,15.7075604217756));
#24540=CARTESIAN_POINT('Ctrl Pts',(78.986136569876,11.2218160635441,18.0014832142357));
#24541=CARTESIAN_POINT('Ctrl Pts',(79.0257548577905,8.03290188515943,19.6330089639828));
#24542=CARTESIAN_POINT('Ctrl Pts',(79.0653731457051,4.6479796756686,20.4040825751338));
#24543=CARTESIAN_POINT('Ctrl Pts',(79.1049914336197,1.26305746617771,21.1751561862849));
#24544=CARTESIAN_POINT('Ctrl Pts',(79.1446097215342,-2.31787277441935,21.0857776588399));
#24545=CARTESIAN_POINT('Ctrl Pts',(79.1842280094488,-5.66011273856516,20.1467968815155));
#24546=CARTESIAN_POINT('Ctrl Pts',(79.2238462973634,-9.00235270271097,19.207816104191));
#24547=CARTESIAN_POINT('Ctrl Pts',(79.263464585278,-12.1059023904055,17.4192330769871));
#24548=CARTESIAN_POINT('Ctrl Pts',(79.3030828731926,-14.5940139439646,14.9981684815738));
#24549=CARTESIAN_POINT('Ctrl Pts',(79.3427011611072,-17.0821254975237,12.5771038861606));
#24550=CARTESIAN_POINT('Ctrl Pts',(79.3823194490217,-18.9547989169474,9.52355772253809));
#24551=CARTESIAN_POINT('Ctrl Pts',(79.4219377369363,-19.984705572149,6.2082077923363));
#24552=CARTESIAN_POINT('Ctrl Pts',(79.4459062089069,-20.6077837034092,4.20247064271143));
#24553=CARTESIAN_POINT('Ctrl Pts',(79.4698746808775,-20.9224033728877,2.1009115046599));
#24554=CARTESIAN_POINT('Ctrl Pts',(79.4938431528481,-20.9235342978811,-0.000316448518974899));
#24555=CARTESIAN_POINT('Origin',(80.4,0.,0.));
#24556=CARTESIAN_POINT('',(81.2061568471518,-20.9255032265546,0.000505554818943099));
#24557=CARTESIAN_POINT('',(80.9938431528482,-20.9250582860856,0.000536067210225428));
#24558=CARTESIAN_POINT('',(80.4,-20.925,-2.56257342721584E-15));
#24559=CARTESIAN_POINT('Ctrl Pts',(81.2061568471518,-20.9255032265546,0.000505554818943099));
#24560=CARTESIAN_POINT('Ctrl Pts',(81.1988403645412,-20.9261523161782,0.641741347385084));
#24561=CARTESIAN_POINT('Ctrl Pts',(81.1915238819306,-20.8972595484565,1.28291886862289));
#24562=CARTESIAN_POINT('Ctrl Pts',(81.1842073993199,-20.8383967471104,1.92133310540693));
#24563=CARTESIAN_POINT('Ctrl Pts',(81.1445891114053,-20.5196584222495,5.37830558626897));
#24564=CARTESIAN_POINT('Ctrl Pts',(81.1049708234908,-19.3221526752348,8.75425432232823));
#24565=CARTESIAN_POINT('Ctrl Pts',(81.0653525355762,-17.3912478004877,11.639364236673));
#24566=CARTESIAN_POINT('Ctrl Pts',(81.0257342476617,-15.4603429257406,14.5244741510179));
#24567=CARTESIAN_POINT('Ctrl Pts',(80.9861159597471,-12.7960389232611,16.9187452436483));
#24568=CARTESIAN_POINT('Ctrl Pts',(80.9464976718325,-9.72176249027052,18.5315308049465));
#24569=CARTESIAN_POINT('Ctrl Pts',(80.9068793839179,-6.64748605727993,20.1443163662447));
#24570=CARTESIAN_POINT('Ctrl Pts',(80.8672610960033,-3.16323719377827,20.9756163962107));
#24571=CARTESIAN_POINT('Ctrl Pts',(80.8276428080887,0.308022193045609,20.9245172517911));
#24572=CARTESIAN_POINT('Ctrl Pts',(80.7880245201741,3.77928157986949,20.8734181073715));
#24573=CARTESIAN_POINT('Ctrl Pts',(80.7484062322596,7.23755149001558,19.9399197885663));
#24574=CARTESIAN_POINT('Ctrl Pts',(80.708787944345,10.263023668083,18.2373420508659));
#24575=CARTESIAN_POINT('Ctrl Pts',(80.6691696564305,13.2884958461504,16.5347643131654));
#24576=CARTESIAN_POINT('Ctrl Pts',(80.6295513685158,15.8811702921392,14.0631071565697));
#24577=CARTESIAN_POINT('Ctrl Pts',(80.5899330806012,17.7263156044315,11.1224113835086));
#24578=CARTESIAN_POINT('Ctrl Pts',(80.5503147926867,19.5714609167237,8.18171561044757));
#24579=CARTESIAN_POINT('Ctrl Pts',(80.5106965047721,20.6690770953195,4.77198122092119));
#24580=CARTESIAN_POINT('Ctrl Pts',(80.4710782168576,20.8859216967403,1.30712461898108));
#24581=CARTESIAN_POINT('Ctrl Pts',(80.431459928943,21.102766298161,-2.15773198295897));
#24582=CARTESIAN_POINT('Ctrl Pts',(80.3918416410284,20.4388393224069,-5.67771079731262));
#24583=CARTESIAN_POINT('Ctrl Pts',(80.3522233531138,18.974736568142,-8.82551256650441));
#24584=CARTESIAN_POINT('Ctrl Pts',(80.3126050651992,17.5106338138771,-11.9733143356962));
#24585=CARTESIAN_POINT('Ctrl Pts',(80.2729867772846,15.2463552811015,-14.7489390597261));
#24586=CARTESIAN_POINT('Ctrl Pts',(80.2333684893701,12.4567675491407,-16.8154465334283));
#24587=CARTESIAN_POINT('Ctrl Pts',(80.1937502014555,9.66717981717998,-18.8819540071306));
#24588=CARTESIAN_POINT('Ctrl Pts',(80.1541319135409,6.35228288603402,-20.2393442305052));
#24589=CARTESIAN_POINT('Ctrl Pts',(80.1145136256263,2.91448059740862,-20.7228401224167));
#24590=CARTESIAN_POINT('Ctrl Pts',(80.0748953377118,-0.523321691216679,
-21.2063360143281));
#24591=CARTESIAN_POINT('Ctrl Pts',(80.0352770497972,-4.08402933732142,-20.8159375747763));
#24592=CARTESIAN_POINT('Ctrl Pts',(79.9956587618826,-7.33539890596775,-19.5990362717721));
#24593=CARTESIAN_POINT('Ctrl Pts',(79.956040473968,-10.5867684746141,-18.382134968768));
#24594=CARTESIAN_POINT('Ctrl Pts',(79.9164221860534,-13.5287999658021,-16.3387308023114));
#24595=CARTESIAN_POINT('Ctrl Pts',(79.8768038981389,-15.8043526300411,-13.7168778458229));
#24596=CARTESIAN_POINT('Ctrl Pts',(79.8371856102243,-18.0799052942802,-11.0950248893343));
#24597=CARTESIAN_POINT('Ctrl Pts',(79.7975673223097,-19.6889791315702,-7.89472314281364));
#24598=CARTESIAN_POINT('Ctrl Pts',(79.7579490343951,-20.4362445412743,-4.50446544455035));
#24599=CARTESIAN_POINT('Ctrl Pts',(79.7406849719807,-20.7618728647668,-3.02712698333307));
#24600=CARTESIAN_POINT('Ctrl Pts',(79.7234209095663,-20.9238552147395,-1.51371840994956));
#24601=CARTESIAN_POINT('Ctrl Pts',(79.7061568471518,-20.923342133494,-0.000201647965826224));
#24602=CARTESIAN_POINT('Ctrl Pts',(79.4938431528481,-20.9235342978811,-0.000316448518974899));
#24603=CARTESIAN_POINT('Ctrl Pts',(79.5094929687921,-20.9242727165845,-1.37227836431806));
#24604=CARTESIAN_POINT('Ctrl Pts',(79.5251427847361,-20.7913639781663,-2.74409908871077));
#24605=CARTESIAN_POINT('Ctrl Pts',(79.54079260068,-20.5234078536779,-4.08901343479093));
#24606=CARTESIAN_POINT('Ctrl Pts',(79.5804108885946,-19.8450635890258,-7.49373103493513));
#24607=CARTESIAN_POINT('Ctrl Pts',(79.6200291765092,-18.3012351687421,-10.7260125384424));
#24608=CARTESIAN_POINT('Ctrl Pts',(79.6596474644238,-16.0793318849288,-13.3934830022897));
#24609=CARTESIAN_POINT('Ctrl Pts',(79.6992657523384,-13.8574286011154,-16.0609534661369));
#24610=CARTESIAN_POINT('Ctrl Pts',(79.738884040253,-10.9574504537723,-18.1636128903242));
#24611=CARTESIAN_POINT('Ctrl Pts',(79.7785023281675,-7.73143322910731,-19.446214053696));
#24612=CARTESIAN_POINT('Ctrl Pts',(79.8181206160821,-4.50541600444238,-20.7288152170678));
#24613=CARTESIAN_POINT('Ctrl Pts',(79.8577389039966,-0.953359702455491,
-21.1913581196242));
#24614=CARTESIAN_POINT('Ctrl Pts',(79.8973571919113,2.49354245077003,-20.7776934919282));
#24615=CARTESIAN_POINT('Ctrl Pts',(79.9369754798258,5.94044460399564,-20.3640288642323));
#24616=CARTESIAN_POINT('Ctrl Pts',(79.9765937677405,9.28219260845988,-19.074156706284));
#24617=CARTESIAN_POINT('Ctrl Pts',(80.0162120556551,12.1131231017896,-17.0646579080625));
#24618=CARTESIAN_POINT('Ctrl Pts',(80.0558303435696,14.9440535951194,-15.0551591098409));
#24619=CARTESIAN_POINT('Ctrl Pts',(80.0954486314841,17.2641665773147,-12.3260336713461));
#24620=CARTESIAN_POINT('Ctrl Pts',(80.1350669193987,18.7918175820108,-9.20857713019443));
#24621=CARTESIAN_POINT('Ctrl Pts',(80.1746852073133,20.3194685867068,-6.09112058904278));
#24622=CARTESIAN_POINT('Ctrl Pts',(80.2143034952279,21.0546576139037,-2.58533294523431));
#24623=CARTESIAN_POINT('Ctrl Pts',(80.2539217831425,20.908138181714,0.883209246250315));
#24624=CARTESIAN_POINT('Ctrl Pts',(80.2935400710571,20.7616187495243,4.35175143773489));
#24625=CARTESIAN_POINT('Ctrl Pts',(80.3331583589716,19.7333908579481,7.78304817689562));
#24626=CARTESIAN_POINT('Ctrl Pts',(80.3727766468862,17.9482737283106,10.760565550748));
#24627=CARTESIAN_POINT('Ctrl Pts',(80.4123949348008,16.1631565986731,13.7380829246004));
#24628=CARTESIAN_POINT('Ctrl Pts',(80.4520132227154,13.6211502309744,16.2618209331444));
#24629=CARTESIAN_POINT('Ctrl Pts',(80.49163151063,10.6308352988371,18.0254165457365));
#24630=CARTESIAN_POINT('Ctrl Pts',(80.5312497985445,7.64052036669963,19.7890121583286));
#24631=CARTESIAN_POINT('Ctrl Pts',(80.5708680864591,4.20189687012352,20.7924653749687));
#24632=CARTESIAN_POINT('Ctrl Pts',(80.6104863743737,0.732388135970209,20.9139644356731));
#24633=CARTESIAN_POINT('Ctrl Pts',(80.6501046622882,-2.7371205981831,21.0354634963775));
#24634=CARTESIAN_POINT('Ctrl Pts',(80.6897229502028,-6.23751456991377,20.275008401146));
#24635=CARTESIAN_POINT('Ctrl Pts',(80.7293412381174,-9.34387197592999,18.7249127446763));
#24636=CARTESIAN_POINT('Ctrl Pts',(80.768959526032,-12.4502293819462,17.1748170882065));
#24637=CARTESIAN_POINT('Ctrl Pts',(80.8085778139465,-15.1625502222479,14.8350808704987));
#24638=CARTESIAN_POINT('Ctrl Pts',(80.8481961018611,-17.1515789125002,11.9897306728128));
#24639=CARTESIAN_POINT('Ctrl Pts',(80.8878143897757,-19.1406076027525,9.14438047512686));
#24640=CARTESIAN_POINT('Ctrl Pts',(80.9274326776903,-20.4063441429551,5.79341629746302));
#24641=CARTESIAN_POINT('Ctrl Pts',(80.9670509656049,-20.7951375276788,2.34362027709995));
#24642=CARTESIAN_POINT('Ctrl Pts',(80.975981694686,-20.8827790833909,1.56596946822868));
#24643=CARTESIAN_POINT('Ctrl Pts',(80.9849124237671,-20.9258597481872,0.783296629213236));
#24644=CARTESIAN_POINT('Ctrl Pts',(80.9938431528482,-20.9250582860856,0.000536067210225428));
#24645=CARTESIAN_POINT('Origin',(80.4,0.,0.));
#24646=CARTESIAN_POINT('',(82.7061568471518,-20.9253923844606,-0.000516496948829159));
#24647=CARTESIAN_POINT('',(82.4938431528481,-20.925825242932,-0.000460001030962829));
#24648=CARTESIAN_POINT('',(80.4,-20.925,-2.56257342721584E-15));
#24649=CARTESIAN_POINT('Ctrl Pts',(82.7061568471518,-20.9253923844606,-0.000516496948829159));
#24650=CARTESIAN_POINT('Ctrl Pts',(82.6742598195161,-20.9225376980426,2.7950656564594));
#24651=CARTESIAN_POINT('Ctrl Pts',(82.6423627918805,-20.3586526388534,5.59176473337593));
#24652=CARTESIAN_POINT('Ctrl Pts',(82.6104657642448,-19.2680752408653,8.16526646253917));
#24653=CARTESIAN_POINT('Ctrl Pts',(82.5708474763302,-17.913503591114,11.361731462952));
#24654=CARTESIAN_POINT('Ctrl Pts',(82.5312291884156,-15.7463858988448,14.2138623839457));
#24655=CARTESIAN_POINT('Ctrl Pts',(82.491610900501,-13.0297941397213,16.3754317368549));
#24656=CARTESIAN_POINT('Ctrl Pts',(82.4519926125865,-10.3132023805979,18.5370010897641));
#24657=CARTESIAN_POINT('Ctrl Pts',(82.4123743246719,-7.04713655462023,20.0080088745887));
#24658=CARTESIAN_POINT('Ctrl Pts',(82.3727560367573,-3.62807277037813,20.6098856829618));
#24659=CARTESIAN_POINT('Ctrl Pts',(82.3331377488427,-0.209008986136022,
21.2117624913349));
#24660=CARTESIAN_POINT('Ctrl Pts',(82.2935194609282,3.36305275637049,20.9445083232563));
#24661=CARTESIAN_POINT('Ctrl Pts',(82.2539011730136,6.65449071931628,19.8405658477385));
#24662=CARTESIAN_POINT('Ctrl Pts',(82.214282885099,9.94592868226207,18.7366233722206));
#24663=CARTESIAN_POINT('Ctrl Pts',(82.1746645971844,12.9567428656471,16.7959925892633));
#24664=CARTESIAN_POINT('Ctrl Pts',(82.1350463092699,15.3214428125367,14.2542516476342));
#24665=CARTESIAN_POINT('Ctrl Pts',(82.0954280213553,17.6861427594262,11.712510706005));
#24666=CARTESIAN_POINT('Ctrl Pts',(82.0558097334407,19.4047284698202,8.56965960570394));
#24667=CARTESIAN_POINT('Ctrl Pts',(82.0161914455261,20.2685764158903,5.20721710370577));
#24668=CARTESIAN_POINT('Ctrl Pts',(81.9765731576115,21.1324243619604,1.84477460170779));
#24669=CARTESIAN_POINT('Ctrl Pts',(81.9369548696969,21.1415345437067,-1.73725930198728));
#24670=CARTESIAN_POINT('Ctrl Pts',(81.8973365817824,20.2948010527979,-5.10405232332752));
#24671=CARTESIAN_POINT('Ctrl Pts',(81.8577182938678,19.4480675618891,-8.47084534466805));
#24672=CARTESIAN_POINT('Ctrl Pts',(81.8181000059532,17.745490398325,-11.6223974836537));
#24673=CARTESIAN_POINT('Ctrl Pts',(81.7784817180386,15.3937497713701,-14.1761337419043));
#24674=CARTESIAN_POINT('Ctrl Pts',(81.7388634301241,13.0420091444152,-16.7298700001546));
#24675=CARTESIAN_POINT('Ctrl Pts',(81.6992451422095,10.0411050540696,-18.68579037767));
#24676=CARTESIAN_POINT('Ctrl Pts',(81.6596268542949,6.75532494565278,-19.8064606825791));
#24677=CARTESIAN_POINT('Ctrl Pts',(81.6200085663803,3.46954483723591,-20.9271309874884));
#24678=CARTESIAN_POINT('Ctrl Pts',(81.5803902784657,-0.101111289252063,
-21.2125512197913));
#24679=CARTESIAN_POINT('Ctrl Pts',(81.5407719905512,-3.52319232732012,-20.6280734853409));
#24680=CARTESIAN_POINT('Ctrl Pts',(81.5011537026366,-6.94527336538818,-20.0435957508905));
#24681=CARTESIAN_POINT('Ctrl Pts',(81.461535414722,-10.2187793150363,-18.5892200496866));
#24682=CARTESIAN_POINT('Ctrl Pts',(81.4219171268074,-12.9463308919772,-16.4414967788018));
#24683=CARTESIAN_POINT('Ctrl Pts',(81.3822988388929,-15.6738824689181,-14.2937735079169));
#24684=CARTESIAN_POINT('Ctrl Pts',(81.3426805509783,-17.8554796731518,-11.452702667351));
#24685=CARTESIAN_POINT('Ctrl Pts',(81.3030622630637,-19.2262928239151,-8.26316913423555));
#24686=CARTESIAN_POINT('Ctrl Pts',(81.2707604577598,-20.3439519110395,-5.66266071703114));
#24687=CARTESIAN_POINT('Ctrl Pts',(81.2384586524558,-20.9226375371568,-2.83050967855002));
#24688=CARTESIAN_POINT('Ctrl Pts',(81.2061568471518,-20.9255032265546,0.000505554818943099));
#24689=CARTESIAN_POINT('Ctrl Pts',(80.9938431528482,-20.9250582860856,0.000536067210225428));
#24690=CARTESIAN_POINT('Ctrl Pts',(81.0245307116816,-20.9223043210767,-2.68916715644739));
#24691=CARTESIAN_POINT('Ctrl Pts',(81.0552182705152,-20.4014206134196,-5.37990615234729));
#24692=CARTESIAN_POINT('Ctrl Pts',(81.0859058293486,-19.3899459682665,-7.8714862729993));
#24693=CARTESIAN_POINT('Ctrl Pts',(81.1255241172632,-18.0841107948856,-11.0881689396731));
#24694=CARTESIAN_POINT('Ctrl Pts',(81.1651424051778,-15.960590218879,-13.9729064099583));
#24695=CARTESIAN_POINT('Ctrl Pts',(81.2047606930923,-13.2771638501336,-16.1755130025299));
#24696=CARTESIAN_POINT('Ctrl Pts',(81.2443789810069,-10.5937374813882,-18.3781195951016));
#24697=CARTESIAN_POINT('Ctrl Pts',(81.2839972689215,-7.35040531990409,-19.8985953099598));
#24698=CARTESIAN_POINT('Ctrl Pts',(81.3236155568361,-3.94088377642275,-20.5523656998175));
#24699=CARTESIAN_POINT('Ctrl Pts',(81.3632338447507,-0.531362232941471,
-21.2061360896753));
#24700=CARTESIAN_POINT('Ctrl Pts',(81.4028521326652,3.04434869253702,-20.9932011545327));
#24701=CARTESIAN_POINT('Ctrl Pts',(81.4424704205798,6.35218427850588,-19.9394096123785));
#24702=CARTESIAN_POINT('Ctrl Pts',(81.4820887084944,9.66001986447484,-18.8856180702242));
#24703=CARTESIAN_POINT('Ctrl Pts',(81.521706996409,12.6999801109342,-16.9909699210582));
#24704=CARTESIAN_POINT('Ctrl Pts',(81.5613252843236,15.1030364455882,-14.4854613637793));
#24705=CARTESIAN_POINT('Ctrl Pts',(81.6009435722382,17.5060927802421,-11.9799528065006));
#24706=CARTESIAN_POINT('Ctrl Pts',(81.6405618601527,19.2722452030907,-8.86358384110923));
#24707=CARTESIAN_POINT('Ctrl Pts',(81.6801801480673,20.1870959410649,-5.51465849029216));
#24708=CARTESIAN_POINT('Ctrl Pts',(81.7197984359819,21.1019466790391,-2.16573313947484));
#24709=CARTESIAN_POINT('Ctrl Pts',(81.7594167238965,21.1654957321386,1.4157485967681));
#24710=CARTESIAN_POINT('Ctrl Pts',(81.799035011811,20.3700287177943,4.79502146340806));
#24711=CARTESIAN_POINT('Ctrl Pts',(81.8386532997256,19.5745617034501,8.17429433004782));
#24712=CARTESIAN_POINT('Ctrl Pts',(81.8782715876402,17.9200786216621,11.3513583270846));
#24713=CARTESIAN_POINT('Ctrl Pts',(81.9178898755548,15.607421417739,13.9405415062475));
#24714=CARTESIAN_POINT('Ctrl Pts',(81.9575081634694,13.2947642138159,16.5297246854105));
#24715=CARTESIAN_POINT('Ctrl Pts',(81.9971264513839,10.3239328877575,18.5310270466995));
#24716=CARTESIAN_POINT('Ctrl Pts',(82.0367447392985,7.05556427488541,19.7015053628211));
#24717=CARTESIAN_POINT('Ctrl Pts',(82.0763630272131,3.78719566201337,20.8719836789428));
#24718=CARTESIAN_POINT('Ctrl Pts',(82.1159813151277,0.221289762327655,21.2116379498971));
#24719=CARTESIAN_POINT('Ctrl Pts',(82.1555996030423,-3.20927895989728,20.6792366724662));
#24720=CARTESIAN_POINT('Ctrl Pts',(82.1952178909568,-6.63984768212221,20.1468353950352));
#24721=CARTESIAN_POINT('Ctrl Pts',(82.2348361788714,-9.93507922688639,18.7423785692189));
#24722=CARTESIAN_POINT('Ctrl Pts',(82.274454466786,-12.6949569841818,16.6363568117567));
#24723=CARTESIAN_POINT('Ctrl Pts',(82.3140727547005,-15.4548347414771,14.5303350542944));
#24724=CARTESIAN_POINT('Ctrl Pts',(82.3536910426151,-17.6793587113037,11.7227483651862));
#24725=CARTESIAN_POINT('Ctrl Pts',(82.3933093305297,-19.0984882227091,8.5544168945259));
#24726=CARTESIAN_POINT('Ctrl Pts',(82.4268206046358,-20.2988641236403,5.87447210232992));
#24727=CARTESIAN_POINT('Ctrl Pts',(82.460331878742,-20.9230057193434,2.93642580920009));
#24728=CARTESIAN_POINT('Ctrl Pts',(82.4938431528481,-20.925825242932,-0.000460001030962829));
#24729=CARTESIAN_POINT('Origin',(80.4,0.,0.));
#24730=CARTESIAN_POINT('',(84.2061568471519,-20.9233820813322,0.00023179675235574));
#24731=CARTESIAN_POINT('',(83.9938431528481,-20.9232570769787,0.000107667472307858));
#24732=CARTESIAN_POINT('',(80.4,-20.925,-2.56257342721584E-15));
#24733=CARTESIAN_POINT('Ctrl Pts',(84.2061568471519,-20.9233820813322,0.00023179675235574));
#24734=CARTESIAN_POINT('Ctrl Pts',(84.1892975624057,-20.923959414903,1.4782541776566));
#24735=CARTESIAN_POINT('Ctrl Pts',(84.1724382776596,-20.7695434732479,2.95615766785475));
#24736=CARTESIAN_POINT('Ctrl Pts',(84.1555789929134,-20.4588924176437,4.40045690073148));
#24737=CARTESIAN_POINT('Ctrl Pts',(84.1159607049988,-19.7288814386964,7.79447175393849));
#24738=CARTESIAN_POINT('Ctrl Pts',(84.0763424170842,-18.1361069579233,11.0029167567447));
#24739=CARTESIAN_POINT('Ctrl Pts',(84.0367241291696,-15.8739199552632,13.6363105400914));
#24740=CARTESIAN_POINT('Ctrl Pts',(83.997105841255,-13.6117329526033,16.2697043234381));
#24741=CARTESIAN_POINT('Ctrl Pts',(83.9574875533405,-10.6801334280564,18.3280468873253));
#24742=CARTESIAN_POINT('Ctrl Pts',(83.9178692654259,-7.43499576792306,19.5614707479493));
#24743=CARTESIAN_POINT('Ctrl Pts',(83.8782509775113,-4.18985810778959,20.7948946085734));
#24744=CARTESIAN_POINT('Ctrl Pts',(83.8386326895967,-0.631182312069551,
21.2033997659342));
#24745=CARTESIAN_POINT('Ctrl Pts',(83.7990144016822,2.8090348358294,20.7373967310993));
#24746=CARTESIAN_POINT('Ctrl Pts',(83.7593961137676,6.24925198372836,20.2713936962645));
#24747=CARTESIAN_POINT('Ctrl Pts',(83.719777825853,9.57101048380623,18.9308824692342));
#24748=CARTESIAN_POINT('Ctrl Pts',(83.6801595379384,12.3710735509036,16.8785911464804));
#24749=CARTESIAN_POINT('Ctrl Pts',(83.6405412500238,15.1711366180009,14.8262998237266));
#24750=CARTESIAN_POINT('Ctrl Pts',(83.6009229621092,17.4495042521178,12.0622284052495));
#24751=CARTESIAN_POINT('Ctrl Pts',(83.5613046741946,18.9295995617761,8.92191461081752));
#24752=CARTESIAN_POINT('Ctrl Pts',(83.5216863862801,20.4096948714344,5.78160081638541));
#24753=CARTESIAN_POINT('Ctrl Pts',(83.4820680983655,21.0915178566342,2.26504464599836));
#24754=CARTESIAN_POINT('Ctrl Pts',(83.442449810451,20.8923002762184,-1.20087012629864));
#24755=CARTESIAN_POINT('Ctrl Pts',(83.4028315225364,20.6930826958026,-4.66678489859564));
#24756=CARTESIAN_POINT('Ctrl Pts',(83.3632132346218,19.6128245497712,-8.08205827280259));
#24757=CARTESIAN_POINT('Ctrl Pts',(83.3235949467072,17.7826611455037,-11.0321014533091));
#24758=CARTESIAN_POINT('Ctrl Pts',(83.2839766587926,15.9524977412362,-13.9821446338157));
#24759=CARTESIAN_POINT('Ctrl Pts',(83.244358370878,13.3724290787325,-16.4669576206218));
#24760=CARTESIAN_POINT('Ctrl Pts',(83.2047400829634,10.3556563112174,-18.1849025913216));
#24761=CARTESIAN_POINT('Ctrl Pts',(83.1651217950489,7.33888354370234,-19.9028475620214));
#24762=CARTESIAN_POINT('Ctrl Pts',(83.1255035071344,3.88540667117585,-20.8539245166148));
#24763=CARTESIAN_POINT('Ctrl Pts',(83.0858852192198,0.414452109907308,-20.9226797839212));
#24764=CARTESIAN_POINT('Ctrl Pts',(83.0462669313052,-3.05650245136114,-20.9914350512277));
#24765=CARTESIAN_POINT('Ctrl Pts',(83.0066486433905,-6.54493470137163,-20.1778686312471));
#24766=CARTESIAN_POINT('Ctrl Pts',(82.967030355476,-9.62737490091601,-18.5807414386274));
#24767=CARTESIAN_POINT('Ctrl Pts',(82.9274120675614,-12.7098151004605,-16.9836142460076));
#24768=CARTESIAN_POINT('Ctrl Pts',(82.8877937796469,-15.3862632495388,-14.6029262807486));
#24769=CARTESIAN_POINT('Ctrl Pts',(82.8481754917323,-17.3318184418224,-11.7276753617935));
#24770=CARTESIAN_POINT('Ctrl Pts',(82.8085572038177,-19.2773736341059,-8.85242444283849));
#24771=CARTESIAN_POINT('Ctrl Pts',(82.7689389159031,-20.4920358695947,-5.48261057018744));
#24772=CARTESIAN_POINT('Ctrl Pts',(82.7293206279885,-20.8283541837223,-2.02730409394606));
#24773=CARTESIAN_POINT('Ctrl Pts',(82.7215993677096,-20.8938997026386,-1.3538948667747));
#24774=CARTESIAN_POINT('Ctrl Pts',(82.7138781074307,-20.9260834136405,-0.677238406088404));
#24775=CARTESIAN_POINT('Ctrl Pts',(82.7061568471518,-20.9253923844606,-0.000516496948829159));
#24776=CARTESIAN_POINT('Ctrl Pts',(82.4938431528481,-20.925825242932,-0.000460001030962829));
#24777=CARTESIAN_POINT('Ctrl Pts',(82.4999501666566,-20.9263390661139,-0.535670991221695));
#24778=CARTESIAN_POINT('Ctrl Pts',(82.506057180465,-20.9062184484103,-1.0708434411499));
#24779=CARTESIAN_POINT('Ctrl Pts',(82.5121641942734,-20.8651905092526,-1.60440824321744));
#24780=CARTESIAN_POINT('Ctrl Pts',(82.551782482188,-20.5990282314065,-5.06582565808811));
#24781=CARTESIAN_POINT('Ctrl Pts',(82.5914007701026,-19.4529686227302,-8.45958423561709));
#24782=CARTESIAN_POINT('Ctrl Pts',(82.6310190580172,-17.5661347989447,-11.3737069165516));
#24783=CARTESIAN_POINT('Ctrl Pts',(82.6706373459318,-15.6793009751592,-14.2878295974861));
#24784=CARTESIAN_POINT('Ctrl Pts',(82.7102556338464,-13.0516929362646,-16.7223163818261));
#24785=CARTESIAN_POINT('Ctrl Pts',(82.749873921761,-10.0022827623316,-18.3816386739777));
#24786=CARTESIAN_POINT('Ctrl Pts',(82.7894922096756,-6.95287258839857,-20.0409609661294));
#24787=CARTESIAN_POINT('Ctrl Pts',(82.8291104975901,-3.48166027942724,-20.9251187660927));
#24788=CARTESIAN_POINT('Ctrl Pts',(82.8687287855047,-0.0100252018111283,
-20.9267818905258));
#24789=CARTESIAN_POINT('Ctrl Pts',(82.9083470734192,3.46160987580508,-20.9284450149589));
#24790=CARTESIAN_POINT('Ctrl Pts',(82.9479653613338,6.93366772206606,-20.0476134638616));
#24791=CARTESIAN_POINT('Ctrl Pts',(82.9875836492484,9.98466632863772,-18.3912136386938));
#24792=CARTESIAN_POINT('Ctrl Pts',(83.027201937163,13.0356649352094,-16.734813813526));
#24793=CARTESIAN_POINT('Ctrl Pts',(83.0668202250775,15.6656043020917,-14.3028457142875));
#24794=CARTESIAN_POINT('Ctrl Pts',(83.1064385129921,17.5552293433292,-11.3905321869272));
#24795=CARTESIAN_POINT('Ctrl Pts',(83.1460568009067,19.4448543845667,-8.47821865956675));
#24796=CARTESIAN_POINT('Ctrl Pts',(83.1856750888213,20.5941651001593,-5.08555970408439));
#24797=CARTESIAN_POINT('Ctrl Pts',(83.2252933767359,20.8636437141779,-1.62439889379187));
#24798=CARTESIAN_POINT('Ctrl Pts',(83.2649116646505,21.1331223281966,1.83676191650065));
#24799=CARTESIAN_POINT('Ctrl Pts',(83.304529952565,20.5227688406411,5.36642458160333));
#24800=CARTESIAN_POINT('Ctrl Pts',(83.3441482404796,19.1066756270191,8.5361142964574));
#24801=CARTESIAN_POINT('Ctrl Pts',(83.3837665283941,17.690582413397,11.7058040113115));
#24802=CARTESIAN_POINT('Ctrl Pts',(83.4233848163088,15.4687494737083,14.5155207759169));
#24803=CARTESIAN_POINT('Ctrl Pts',(83.4630031042234,12.710890807854,16.6241858648513));
#24804=CARTESIAN_POINT('Ctrl Pts',(83.502621392138,9.9530321419997,18.7328509537856));
#24805=CARTESIAN_POINT('Ctrl Pts',(83.5422396800525,6.65914774997982,20.1404643670489));
#24806=CARTESIAN_POINT('Ctrl Pts',(83.5818579679671,3.22909070747509,20.6761523016544));
#24807=CARTESIAN_POINT('Ctrl Pts',(83.6214762558816,-0.200966335029539,
21.2118402362598));
#24808=CARTESIAN_POINT('Ctrl Pts',(83.6610945437962,-3.76719602801901,20.8756026922076));
#24809=CARTESIAN_POINT('Ctrl Pts',(83.7007128317108,-7.0366846011192,19.7082564074725));
#24810=CARTESIAN_POINT('Ctrl Pts',(83.7403311196254,-10.3061731742194,18.5409101227374));
#24811=CARTESIAN_POINT('Ctrl Pts',(83.77994940754,-13.2789206274303,16.5424550973195));
#24812=CARTESIAN_POINT('Ctrl Pts',(83.8195676954546,-15.5940575218402,13.9554889131069));
#24813=CARTESIAN_POINT('Ctrl Pts',(83.8591859833692,-17.90919441625,11.3685227288943));
#24814=CARTESIAN_POINT('Ctrl Pts',(83.8988042712837,-19.5667207518589,8.19304538588687));
#24815=CARTESIAN_POINT('Ctrl Pts',(83.9384225591983,-20.3654251549704,4.81453622435309));
#24816=CARTESIAN_POINT('Ctrl Pts',(83.9568960904149,-20.7378514131556,3.23917803129373));
#24817=CARTESIAN_POINT('Ctrl Pts',(83.9753696216315,-20.9235487635752,1.61967575168914));
#24818=CARTESIAN_POINT('Ctrl Pts',(83.9938431528481,-20.9232570769787,0.000107667472307858));
#24819=CARTESIAN_POINT('Origin',(80.4,0.,0.));
#24820=CARTESIAN_POINT('',(85.7061568471519,-20.9266764847855,0.000165093697623506));
#24821=CARTESIAN_POINT('',(85.4938431528481,-20.9264318713289,0.000296857018782903));
#24822=CARTESIAN_POINT('',(80.4,-20.925,-2.56257342721584E-15));
#24823=CARTESIAN_POINT('Ctrl Pts',(85.7061568471519,-20.9266764847855,0.000165093697623506));
#24824=CARTESIAN_POINT('Ctrl Pts',(85.7043353052952,-20.9267437401954,0.159783909494946));
#24825=CARTESIAN_POINT('Ctrl Pts',(85.7025137634386,-20.924955439811,0.319401214298244));
#24826=CARTESIAN_POINT('Ctrl Pts',(85.700692221582,-20.9213021118419,0.478975820845309));
#24827=CARTESIAN_POINT('Ctrl Pts',(85.6610739336674,-20.8418427248384,3.94970183408668));
#24828=CARTESIAN_POINT('Ctrl Pts',(85.6214556457528,-19.8801197477881,7.40022915582282));
#24829=CARTESIAN_POINT('Ctrl Pts',(85.5818373578382,-18.1528791998465,10.4116894233209));
#24830=CARTESIAN_POINT('Ctrl Pts',(85.5422190699236,-16.4256386519049,13.4231496908189));
#24831=CARTESIAN_POINT('Ctrl Pts',(85.502600782009,-13.932880533072,15.9955429040789));
#24832=CARTESIAN_POINT('Ctrl Pts',(85.4629824940945,-10.977207145711,17.8165996523485));
#24833=CARTESIAN_POINT('Ctrl Pts',(85.4233642061799,-8.02153375834987,19.6376564006182));
#24834=CARTESIAN_POINT('Ctrl Pts',(85.3837459182653,-4.60294510246061,20.7073766838974));
#24835=CARTESIAN_POINT('Ctrl Pts',(85.3441276303508,-1.13643242420114,20.8959044129977));
#24836=CARTESIAN_POINT('Ctrl Pts',(85.3045093424362,2.33008025405834,21.0844321420979));
#24837=CARTESIAN_POINT('Ctrl Pts',(85.2648910545216,5.84451695468797,20.3917673170192));
#24838=CARTESIAN_POINT('Ctrl Pts',(85.225272766607,8.98025119151343,18.9019942976723));
#24839=CARTESIAN_POINT('Ctrl Pts',(85.1856544786924,12.1159854283389,17.4122212783253));
#24840=CARTESIAN_POINT('Ctrl Pts',(85.1460361907778,14.8730172013601,15.1253400647103));
#24841=CARTESIAN_POINT('Ctrl Pts',(85.1064179028633,16.9166633514284,12.3189610335593));
#24842=CARTESIAN_POINT('Ctrl Pts',(85.0667996149487,18.9603095014967,9.51258200240819));
#24843=CARTESIAN_POINT('Ctrl Pts',(85.0271813270341,20.290570028612,6.1867051537211));
#24844=CARTESIAN_POINT('Ctrl Pts',(84.9875630391195,20.7459611950595,2.74506720955921));
#24845=CARTESIAN_POINT('Ctrl Pts',(84.9479447512049,21.2013523615071,-0.696570734602592));
#24846=CARTESIAN_POINT('Ctrl Pts',(84.9083264632903,20.7818741672868,-4.2539697742394));
#24847=CARTESIAN_POINT('Ctrl Pts',(84.8687081753757,19.538448146423,-7.49528811463913));
#24848=CARTESIAN_POINT('Ctrl Pts',(84.8290898874612,18.2950221255592,-10.7366064550388));
#24849=CARTESIAN_POINT('Ctrl Pts',(84.7894715995466,16.227648278052,-13.6618440962017));
#24850=CARTESIAN_POINT('Ctrl Pts',(84.7498533116321,13.5872904183904,-15.9158989371707));
#24851=CARTESIAN_POINT('Ctrl Pts',(84.7102350237175,10.9469325587286,-18.1699537781397));
#24852=CARTESIAN_POINT('Ctrl Pts',(84.6706167358029,7.73359068691255,-19.7528258189148));
#24853=CARTESIAN_POINT('Ctrl Pts',(84.6309984478883,4.33734061549098,-20.4723661621495));
#24854=CARTESIAN_POINT('Ctrl Pts',(84.5913801599737,0.941090544069511,-21.1919065053843));
#24855=CARTESIAN_POINT('Ctrl Pts',(84.5517618720591,-2.63806772695736,-21.0481151510788));
#24856=CARTESIAN_POINT('Ctrl Pts',(84.5121435841446,-5.96565099396377,-20.0584473005797));
#24857=CARTESIAN_POINT('Ctrl Pts',(84.47252529623,-9.29323426097029,-19.0687794500805));
#24858=CARTESIAN_POINT('Ctrl Pts',(84.4329070083154,-12.3692425239563,-17.2332351033878));
#24859=CARTESIAN_POINT('Ctrl Pts',(84.3932887204009,-14.8202712494312,-14.7746356972074));
#24860=CARTESIAN_POINT('Ctrl Pts',(84.3536704324863,-17.271299974906,-12.3160362910271));
#24861=CARTESIAN_POINT('Ctrl Pts',(84.3140521445717,-19.0973491628698,-9.23438182535918));
#24862=CARTESIAN_POINT('Ctrl Pts',(84.2744338566571,-20.076750018291,-5.90376224072128));
#24863=CARTESIAN_POINT('Ctrl Pts',(84.2516748534887,-20.6393737040934,-3.99046447674405));
#24864=CARTESIAN_POINT('Ctrl Pts',(84.2289158503203,-20.9226027163257,-1.99500801065722));
#24865=CARTESIAN_POINT('Ctrl Pts',(84.2061568471519,-20.9233820813322,0.00023179675235574));
#24866=CARTESIAN_POINT('Ctrl Pts',(83.9938431528481,-20.9232570769787,0.000107667472307858));
#24867=CARTESIAN_POINT('Ctrl Pts',(84.0149879095461,-20.9229232132446,-1.85364582962594));
#24868=CARTESIAN_POINT('Ctrl Pts',(84.0361326662441,-20.6789244947364,-3.70748553756512));
#24869=CARTESIAN_POINT('Ctrl Pts',(84.0572774229421,-20.192370387916,-5.49531426904058));
#24870=CARTESIAN_POINT('Ctrl Pts',(84.0968957108566,-19.2807287471359,-8.84511462083977));
#24871=CARTESIAN_POINT('Ctrl Pts',(84.1365139987711,-17.5175629949616,-11.9631743443778));
#24872=CARTESIAN_POINT('Ctrl Pts',(84.1761322866857,-15.1169083448479,-14.4709841714991));
#24873=CARTESIAN_POINT('Ctrl Pts',(84.2157505746003,-12.7162536947343,-16.9787939986203));
#24874=CARTESIAN_POINT('Ctrl Pts',(84.255368862515,-9.6781101466813,-18.8763539293247));
#24875=CARTESIAN_POINT('Ctrl Pts',(84.2949871504296,-6.37128573930498,-19.9333142960833));
#24876=CARTESIAN_POINT('Ctrl Pts',(84.3346054383442,-3.06446133192865,-20.9902746628419));
#24877=CARTESIAN_POINT('Ctrl Pts',(84.3742237262587,0.511043934770997,-21.2066354656546));
#24878=CARTESIAN_POINT('Ctrl Pts',(84.4138420141732,3.92119030473388,-20.5561321116685));
#24879=CARTESIAN_POINT('Ctrl Pts',(84.4534603020878,7.33133667469677,-19.9056287576824));
#24880=CARTESIAN_POINT('Ctrl Pts',(84.4930785900024,10.5761241479228,-18.3882612468975));
#24881=CARTESIAN_POINT('Ctrl Pts',(84.532696877917,13.2616596496451,-16.188226713735));
#24882=CARTESIAN_POINT('Ctrl Pts',(84.5723151658316,15.9471951513673,-13.9881921805726));
#24883=CARTESIAN_POINT('Ctrl Pts',(84.6119334537461,18.0734786815857,-11.1054906250329));
#24884=CARTESIAN_POINT('Ctrl Pts',(84.6515517416607,19.3823952283142,-7.89006058352727));
#24885=CARTESIAN_POINT('Ctrl Pts',(84.6911700295753,20.6913117750429,-4.67463054202134));
#24886=CARTESIAN_POINT('Ctrl Pts',(84.7307883174899,21.1828613382816,-1.12647201454918));
#24887=CARTESIAN_POINT('Ctrl Pts',(84.7704066054045,20.7973734556465,2.32369493365209));
#24888=CARTESIAN_POINT('Ctrl Pts',(84.8100248933191,20.4118855730113,5.77386188185326));
#24889=CARTESIAN_POINT('Ctrl Pts',(84.8496431812336,19.1493602445025,9.12603725078375));
#24890=CARTESIAN_POINT('Ctrl Pts',(84.8892614691482,17.1630586583245,11.9732918735502));
#24891=CARTESIAN_POINT('Ctrl Pts',(84.9288797570627,15.1767570721465,14.8205464963164));
#24892=CARTESIAN_POINT('Ctrl Pts',(84.9684980449774,12.4666792282994,17.1628803729186));
#24893=CARTESIAN_POINT('Ctrl Pts',(85.0081163328919,9.36180842802518,18.7159515856198));
#24894=CARTESIAN_POINT('Ctrl Pts',(85.0477346208065,6.25693762775077,20.2690227983212));
#24895=CARTESIAN_POINT('Ctrl Pts',(85.0873529087211,2.75727387104925,21.0328313471215));
#24896=CARTESIAN_POINT('Ctrl Pts',(85.1269711966357,-0.712349681463435,
20.9146565529924));
#24897=CARTESIAN_POINT('Ctrl Pts',(85.1665894845502,-4.18197323397612,20.7964817588633));
#24898=CARTESIAN_POINT('Ctrl Pts',(85.2062077724648,-7.62155658229993,19.7963236218048));
#24899=CARTESIAN_POINT('Ctrl Pts',(85.2458260603794,-10.6135598807076,18.035593903638));
#24900=CARTESIAN_POINT('Ctrl Pts',(85.285444348294,-13.6055631791152,16.2748641854711));
#24901=CARTESIAN_POINT('Ctrl Pts',(85.3250626362085,-16.1499864276067,13.7535628861959));
#24902=CARTESIAN_POINT('Ctrl Pts',(85.3646809241231,-17.9379555612003,10.7777572380672));
#24903=CARTESIAN_POINT('Ctrl Pts',(85.4042992120377,-19.725924694794,7.80195158993853));
#24904=CARTESIAN_POINT('Ctrl Pts',(85.4439174999523,-20.7574397134897,4.37164159295638));
#24905=CARTESIAN_POINT('Ctrl Pts',(85.4835357878669,-20.9072823631693,0.903241376941042));
#24906=CARTESIAN_POINT('Ctrl Pts',(85.4869715761939,-20.9202770596534,0.602453796176518));
#24907=CARTESIAN_POINT('Ctrl Pts',(85.490407364521,-20.9266409150071,0.301379748239037));
#24908=CARTESIAN_POINT('Ctrl Pts',(85.4938431528481,-20.9264318713289,0.000296857018782903));
#24909=CARTESIAN_POINT('Origin',(80.4,0.,0.));
#24910=CARTESIAN_POINT('',(87.2061568471519,-20.9239756446721,-0.00045287493121049));
#24911=CARTESIAN_POINT('',(86.9938431528481,-20.9243500731069,-0.000510630017847893));
#24912=CARTESIAN_POINT('',(80.4,-20.925,-2.56257342721584E-15));
#24913=CARTESIAN_POINT('Ctrl Pts',(87.2061568471519,-20.9239756446721,-0.00045287493121049));
#24914=CARTESIAN_POINT('Ctrl Pts',(87.1797547602702,-20.9221409849285,2.3139812699255));
#24915=CARTESIAN_POINT('Ctrl Pts',(87.1533526733885,-20.5391101652039,4.62900771036594));
#24916=CARTESIAN_POINT('Ctrl Pts',(87.1269505865068,-19.7855330252692,6.81637607515132));
#24917=CARTESIAN_POINT('Ctrl Pts',(87.0873322985922,-18.6547346823365,10.0986844032635));
#24918=CARTESIAN_POINT('Ctrl Pts',(87.0477140106776,-16.6895687983901,13.093542151339));
#24919=CARTESIAN_POINT('Ctrl Pts',(87.008095722763,-14.1285919010428,15.437395855056));
#24920=CARTESIAN_POINT('Ctrl Pts',(86.9684774348485,-11.5676150036958,17.7812495587728));
#24921=CARTESIAN_POINT('Ctrl Pts',(86.9288591469339,-8.41082709294795,19.4740992181312));
#24922=CARTESIAN_POINT('Ctrl Pts',(86.8892408590193,-5.04143875094444,20.310445470555));
#24923=CARTESIAN_POINT('Ctrl Pts',(86.8496225711047,-1.67205040894083,21.1467917229788));
#24924=CARTESIAN_POINT('Ctrl Pts',(86.8100042831901,1.90993836431854,21.1266345684681));
#24925=CARTESIAN_POINT('Ctrl Pts',(86.7703859952755,5.26970076328099,20.252420935715));
#24926=CARTESIAN_POINT('Ctrl Pts',(86.730767707361,8.62946316224335,19.378207302962));
#24927=CARTESIAN_POINT('Ctrl Pts',(86.6911494194465,11.7669991869089,17.6499371919668));
#24928=CARTESIAN_POINT('Ctrl Pts',(86.6515311315319,14.3014352909681,15.2774097447887));
#24929=CARTESIAN_POINT('Ctrl Pts',(86.6119128436173,16.8358713950276,12.9048822976105));
#24930=CARTESIAN_POINT('Ctrl Pts',(86.5722945557027,18.7672075784806,9.88809751424954));
#24931=CARTESIAN_POINT('Ctrl Pts',(86.5326762677881,19.8609939878359,6.59327063808692));
#24932=CARTESIAN_POINT('Ctrl Pts',(86.4930579798735,20.9547803971911,3.29844376192457));
#24933=CARTESIAN_POINT('Ctrl Pts',(86.453439691959,21.2110170324486,-0.274425207039511));
#24934=CARTESIAN_POINT('Ctrl Pts',(86.4138214040444,20.598598671167,-3.69161653968933));
#24935=CARTESIAN_POINT('Ctrl Pts',(86.3742031161298,19.9861803098854,-7.10880787233935));
#24936=CARTESIAN_POINT('Ctrl Pts',(86.3345848282152,18.5051069520648,-10.3703215686751));
#24937=CARTESIAN_POINT('Ctrl Pts',(86.2949665403006,16.3351698917978,-13.0802341148015));
#24938=CARTESIAN_POINT('Ctrl Pts',(86.255348252386,14.1652328315308,-15.7901466609278));
#24939=CARTESIAN_POINT('Ctrl Pts',(86.2157299644714,11.3064320688171,-17.9484580568446));
#24940=CARTESIAN_POINT('Ctrl Pts',(86.1761116765569,8.10580476151847,-19.2931653457917));
#24941=CARTESIAN_POINT('Ctrl Pts',(86.1364933886423,4.90517745421972,-20.6378726347388));
#24942=CARTESIAN_POINT('Ctrl Pts',(86.0968751007277,1.36272360233598,-21.1689758167164));
#24943=CARTESIAN_POINT('Ctrl Pts',(86.0572568128131,-2.09152923409976,-20.8220029141007));
#24944=CARTESIAN_POINT('Ctrl Pts',(86.0176385248986,-5.5457820705354,-20.475030011485));
#24945=CARTESIAN_POINT('Ctrl Pts',(85.978020236984,-8.9118338915228,-19.2499810242761));
#24946=CARTESIAN_POINT('Ctrl Pts',(85.9384019490694,-11.7810710320579,-17.2955677914753));
#24947=CARTESIAN_POINT('Ctrl Pts',(85.8987836611549,-14.650308172593,-15.3411545586745));
#24948=CARTESIAN_POINT('Ctrl Pts',(85.8591653732403,-17.0227306326758,-12.6573770802819));
#24949=CARTESIAN_POINT('Ctrl Pts',(85.8195470853257,-18.6103439642389,-9.57002598871229));
#24950=CARTESIAN_POINT('Ctrl Pts',(85.7817503392677,-20.1249631234685,-6.62462296040961));
#24951=CARTESIAN_POINT('Ctrl Pts',(85.7439535932098,-20.9252809441659,-3.31190364893342));
#24952=CARTESIAN_POINT('Ctrl Pts',(85.7061568471519,-20.9266764847855,0.000165093697623506));
#24953=CARTESIAN_POINT('Ctrl Pts',(85.4938431528481,-20.9264318713289,0.000296857018782903));
#24954=CARTESIAN_POINT('Ctrl Pts',(85.5300256524356,-20.9242304194112,-3.17042571092434));
#24955=CARTESIAN_POINT('Ctrl Pts',(85.5662081520231,-20.1930730044325,-6.34212902779996));
#24956=CARTESIAN_POINT('Ctrl Pts',(85.6023906516106,-18.8006318920486,-9.19056805959208));
#24957=CARTESIAN_POINT('Ctrl Pts',(85.6420089395252,-17.2759684905849,-12.3094868450616));
#24958=CARTESIAN_POINT('Ctrl Pts',(85.6816272274398,-14.9584714069941,-15.0408339809522));
#24959=CARTESIAN_POINT('Ctrl Pts',(85.7212455153544,-12.1294675569991,-17.0530442321017));
#24960=CARTESIAN_POINT('Ctrl Pts',(85.7608638032689,-9.30046370700389,-19.0652544832512));
#24961=CARTESIAN_POINT('Ctrl Pts',(85.8004820911835,-5.95995309060449,-20.3583278496595));
#24962=CARTESIAN_POINT('Ctrl Pts',(85.8401003790981,-2.51344886046267,-20.7752948384409));
#24963=CARTESIAN_POINT('Ctrl Pts',(85.8797186670126,0.93305536967895,-21.1922618272222));
#24964=CARTESIAN_POINT('Ctrl Pts',(85.9193369549272,4.48555321356299,-20.7331224383767));
#24965=CARTESIAN_POINT('Ctrl Pts',(85.9589552428418,7.71279784520256,-19.4536127800814));
#24966=CARTESIAN_POINT('Ctrl Pts',(85.9985735307564,10.9400424768422,-18.1741031217861));
#24967=CARTESIAN_POINT('Ctrl Pts',(86.038191818671,13.8420338962374,-16.0742231940409));
#24968=CARTESIAN_POINT('Ctrl Pts',(86.0778101065855,16.0664919209217,-13.4088828077982));
#24969=CARTESIAN_POINT('Ctrl Pts',(86.1174283945001,18.2909499456059,-10.7435424215556));
#24970=CARTESIAN_POINT('Ctrl Pts',(86.1570466824147,19.8378745755793,-7.5127415768156));
#24971=CARTESIAN_POINT('Ctrl Pts',(86.1966649703293,20.5194806619033,-4.10867547563538));
#24972=CARTESIAN_POINT('Ctrl Pts',(86.2362832582439,21.2010867482273,-0.704609374455165));
#24973=CARTESIAN_POINT('Ctrl Pts',(86.2759015461584,21.0173742909019,2.87272198316526));
#24974=CARTESIAN_POINT('Ctrl Pts',(86.315519834073,19.9906446163735,6.18905716730465));
#24975=CARTESIAN_POINT('Ctrl Pts',(86.3551381219876,18.9639149418451,9.50539235144405));
#24976=CARTESIAN_POINT('Ctrl Pts',(86.3947564099022,17.0941680501136,12.5607313621024));
#24977=CARTESIAN_POINT('Ctrl Pts',(86.4343746978168,14.6083773125621,14.9841787593491));
#24978=CARTESIAN_POINT('Ctrl Pts',(86.4739929857313,12.1225865750108,17.4076261565957));
#24979=CARTESIAN_POINT('Ctrl Pts',(86.5136112736459,9.02075199163955,19.1991819404306));
#24980=CARTESIAN_POINT('Ctrl Pts',(86.5532295615605,5.67941321921927,20.1413645586307));
#24981=CARTESIAN_POINT('Ctrl Pts',(86.5928478494751,2.33807444679899,21.0835471768309));
#24982=CARTESIAN_POINT('Ctrl Pts',(86.6324661373897,-1.24276851467036,21.1763566293961));
#24983=CARTESIAN_POINT('Ctrl Pts',(86.6720844253043,-4.62842795266854,20.4085265388089));
#24984=CARTESIAN_POINT('Ctrl Pts',(86.7117027132188,-8.01408739066692,19.6406964482215));
#24985=CARTESIAN_POINT('Ctrl Pts',(86.7513210011334,-11.2045633051941,18.0122268144815));
#24986=CARTESIAN_POINT('Ctrl Pts',(86.7909392890479,-13.8125556409113,15.7208017437101));
#24987=CARTESIAN_POINT('Ctrl Pts',(86.8305575769625,-16.4205479766283,13.4293766729389));
#24988=CARTESIAN_POINT('Ctrl Pts',(86.8701758648772,-18.4460567335353,10.4749961651365));
#24989=CARTESIAN_POINT('Ctrl Pts',(86.9097941527917,-19.6432002078817,7.21630004859733));
#24990=CARTESIAN_POINT('Ctrl Pts',(86.9378104861439,-20.4897681039995,4.91189161754273));
#24991=CARTESIAN_POINT('Ctrl Pts',(86.965826819496,-20.9220950074049,2.45530394562074));
#24992=CARTESIAN_POINT('Ctrl Pts',(86.9938431528481,-20.9243500731069,-0.000510630017847893));
#24993=CARTESIAN_POINT('Origin',(80.4,0.,0.));
#24994=CARTESIAN_POINT('',(88.7061568471518,-20.924409432792,0.000516573290169631));
#24995=CARTESIAN_POINT('',(88.4938431528482,-20.9240272266393,0.000463189924240194));
#24996=CARTESIAN_POINT('',(80.4,-20.925,-2.56257342721584E-15));
#24997=CARTESIAN_POINT('Ctrl Pts',(88.7061568471518,-20.924409432792,0.000516573290169631));
#24998=CARTESIAN_POINT('Ctrl Pts',(88.6947925031596,-20.9253390160846,0.996667419708051));
#24999=CARTESIAN_POINT('Ctrl Pts',(88.6834281591675,-20.8554826568381,1.99268898101036));
#25000=CARTESIAN_POINT('Ctrl Pts',(88.6720638151753,-20.71375329641,2.97837611248698));
#25001=CARTESIAN_POINT('Ctrl Pts',(88.6324455272608,-20.2196574989527,6.41467094793555));
#25002=CARTESIAN_POINT('Ctrl Pts',(88.5928272393462,-18.852050566816,9.72536591451949));
#25003=CARTESIAN_POINT('Ctrl Pts',(88.5532089514317,-16.7769498136232,12.5085672578046));
#25004=CARTESIAN_POINT('Ctrl Pts',(88.5135906635171,-14.7018490604304,15.2917686010898));
#25005=CARTESIAN_POINT('Ctrl Pts',(88.4739723756024,-11.9192544861816,17.5474763210762));
#25006=CARTESIAN_POINT('Ctrl Pts',(88.4343540876879,-8.76695238403727,19.0018642713807));
#25007=CARTESIAN_POINT('Ctrl Pts',(88.3947357997733,-5.61465028189307,20.4562522216852));
#25008=CARTESIAN_POINT('Ctrl Pts',(88.3551175118588,-2.09264065185337,21.1093204023079));
#25009=CARTESIAN_POINT('Ctrl Pts',(88.3154992239442,1.3715307225796,20.881791191584));
#25010=CARTESIAN_POINT('Ctrl Pts',(88.2758809360296,4.83570209701267,20.65426198086));
#25011=CARTESIAN_POINT('Ctrl Pts',(88.2362626481149,8.24203521583906,19.5461353787892));
#25012=CARTESIAN_POINT('Ctrl Pts',(88.1966443602004,11.1770265639827,17.6919297161148));
#25013=CARTESIAN_POINT('Ctrl Pts',(88.1570260722858,14.1120179121264,15.8377240534403));
#25014=CARTESIAN_POINT('Ctrl Pts',(88.1174077843713,16.5756674895873,13.2374393301622));
#25015=CARTESIAN_POINT('Ctrl Pts',(88.0777894964567,18.2689065545072,10.2067307789809));
#25016=CARTESIAN_POINT('Ctrl Pts',(88.0381712085422,19.962145619427,7.17602222779963));
#25017=CARTESIAN_POINT('Ctrl Pts',(87.9985529206275,20.8849741718059,3.71488984871517));
#25018=CARTESIAN_POINT('Ctrl Pts',(87.9589346327129,20.9253676864696,0.243489379575099));
#25019=CARTESIAN_POINT('Ctrl Pts',(87.9193163447983,20.9657612011333,-3.22791108956507));
#25020=CARTESIAN_POINT('Ctrl Pts',(87.8796980568838,20.123719678082,-6.70957964876064));
#25021=CARTESIAN_POINT('Ctrl Pts',(87.8400797689692,18.501460697768,-9.77886762058159));
#25022=CARTESIAN_POINT('Ctrl Pts',(87.8004614810546,16.8792017174542,-12.8481555924023));
#25023=CARTESIAN_POINT('Ctrl Pts',(87.76084319314,14.4767252798779,-15.5050629768482));
#25024=CARTESIAN_POINT('Ctrl Pts',(87.7212249052254,11.5856741625279,-17.4270609711346));
#25025=CARTESIAN_POINT('Ctrl Pts',(87.6816066173109,8.69462304517777,-19.3490589654212));
#25026=CARTESIAN_POINT('Ctrl Pts',(87.6419883293963,5.31499724805383,-20.5361475695483));
#25027=CARTESIAN_POINT('Ctrl Pts',(87.6023700414818,1.85705821594267,-20.8442230527912));
#25028=CARTESIAN_POINT('Ctrl Pts',(87.5627517535672,-1.60088081616848,-21.1522985360341));
#25029=CARTESIAN_POINT('Ctrl Pts',(87.5231334656526,-5.13713308326719,-20.5813608983927));
#25030=CARTESIAN_POINT('Ctrl Pts',(87.483515177738,-8.32242385160441,-19.2007177242456));
#25031=CARTESIAN_POINT('Ctrl Pts',(87.4438968898234,-11.5077146199416,-17.8200745500985));
#25032=CARTESIAN_POINT('Ctrl Pts',(87.4042786019088,-14.3420438895175,-15.6297258394458));
#25033=CARTESIAN_POINT('Ctrl Pts',(87.3646603139942,-16.4813451597965,-12.8955636408637));
#25034=CARTESIAN_POINT('Ctrl Pts',(87.3250420260797,-18.6206464300755,-10.1614014422816));
#25035=CARTESIAN_POINT('Ctrl Pts',(87.2854237381651,-20.0649197010575,-6.88342575577012));
#25036=CARTESIAN_POINT('Ctrl Pts',(87.2458054502505,-20.6388409355891,-3.45955845844006));
#25037=CARTESIAN_POINT('Ctrl Pts',(87.2325892492176,-20.8302943984184,-2.31739606593537));
#25038=CARTESIAN_POINT('Ctrl Pts',(87.2193730481847,-20.9248940278327,-1.15899867749903));
#25039=CARTESIAN_POINT('Ctrl Pts',(87.2061568471519,-20.9239756446721,-0.00045287493121049));
#25040=CARTESIAN_POINT('Ctrl Pts',(86.9938431528481,-20.9243500731069,-0.000510630017847893));
#25041=CARTESIAN_POINT('Ctrl Pts',(87.0054451074106,-20.9252839272798,-1.01749771259551));
#25042=CARTESIAN_POINT('Ctrl Pts',(87.017047061973,-20.8524646044492,-2.03435221660832));
#25043=CARTESIAN_POINT('Ctrl Pts',(87.0286490165354,-20.7047678525638,-3.04021199421177));
#25044=CARTESIAN_POINT('Ctrl Pts',(87.06826730445,-20.2004138311137,-6.47501619520576));
#25045=CARTESIAN_POINT('Ctrl Pts',(87.1078855923646,-18.8229275964278,-9.78161287191766));
#25046=CARTESIAN_POINT('Ctrl Pts',(87.1475038802792,-16.7395257360041,-12.5586057718189));
#25047=CARTESIAN_POINT('Ctrl Pts',(87.1871221681938,-14.6561238755806,-15.3355986717201));
#25048=CARTESIAN_POINT('Ctrl Pts',(87.2267404561083,-11.8668063894195,-17.5829877948106));
#25049=CARTESIAN_POINT('Ctrl Pts',(87.2663587440229,-8.71017568220549,-19.0279568105308));
#25050=CARTESIAN_POINT('Ctrl Pts',(87.3059770319375,-5.55354497499143,-20.472925826251));
#25051=CARTESIAN_POINT('Ctrl Pts',(87.3455953198521,-2.0296010467245,-21.1154747346007));
#25052=CARTESIAN_POINT('Ctrl Pts',(87.3852136077667,1.43387550967048,-20.8776028753561));
#25053=CARTESIAN_POINT('Ctrl Pts',(87.4248318956813,4.89735206606537,-20.6397310161114));
#25054=CARTESIAN_POINT('Ctrl Pts',(87.4644501835958,8.30036125058831,-19.5214383892724));
#25055=CARTESIAN_POINT('Ctrl Pts',(87.5040684715104,11.2298030490743,-17.6584774054081));
#25056=CARTESIAN_POINT('Ctrl Pts',(87.5436867594249,14.1592448475604,-15.7955164215438));
#25057=CARTESIAN_POINT('Ctrl Pts',(87.5833050473396,16.6151192600096,-13.1878870806542));
#25058=CARTESIAN_POINT('Ctrl Pts',(87.6229233352542,18.299301391789,-10.1521361974108));
#25059=CARTESIAN_POINT('Ctrl Pts',(87.6625416231687,19.9834835235684,-7.11638531416741));
#25060=CARTESIAN_POINT('Ctrl Pts',(87.7021599110832,20.8959733746781,-3.65251288857022));
#25061=CARTESIAN_POINT('Ctrl Pts',(87.7417781989978,20.9260014614113,-0.181007279742066));
#25062=CARTESIAN_POINT('Ctrl Pts',(87.7813964869124,20.9560295481446,3.29049832908599));
#25063=CARTESIAN_POINT('Ctrl Pts',(87.8210147748271,20.1035958705014,6.769637121145));
#25064=CARTESIAN_POINT('Ctrl Pts',(87.8606330627417,18.4721795392379,9.8340675139267));
#25065=CARTESIAN_POINT('Ctrl Pts',(87.9002513506563,16.8407632079744,12.8984979067085));
#25066=CARTESIAN_POINT('Ctrl Pts',(87.9398696385707,14.4303642230905,15.5482199002129));
#25067=CARTESIAN_POINT('Ctrl Pts',(87.9794879264853,11.5335871004151,17.4615769446934));
#25068=CARTESIAN_POINT('Ctrl Pts',(88.0191062143999,8.63680997773975,19.3749339891738));
#25069=CARTESIAN_POINT('Ctrl Pts',(88.0587245023145,5.25365471727298,20.5519260846302));
#25070=CARTESIAN_POINT('Ctrl Pts',(88.0983427902291,1.79481121441017,20.8496751414245));
#25071=CARTESIAN_POINT('Ctrl Pts',(88.1379610781437,-1.66403228845263,21.1474241982189));
#25072=CARTESIAN_POINT('Ctrl Pts',(88.1775793660582,-5.19856403371147,20.5659302163512));
#25073=CARTESIAN_POINT('Ctrl Pts',(88.2171976539728,-8.37971814617746,19.1757822419043));
#25074=CARTESIAN_POINT('Ctrl Pts',(88.2568159418873,-11.5608722586435,17.7856342674574));
#25075=CARTESIAN_POINT('Ctrl Pts',(88.296434229802,-14.3886487383166,15.5868323004313));
#25076=CARTESIAN_POINT('Ctrl Pts',(88.3360525177166,-16.5197765446363,12.8462945518773));
#25077=CARTESIAN_POINT('Ctrl Pts',(88.3756708056312,-18.650904350956,10.1057568033234));
#25078=CARTESIAN_POINT('Ctrl Pts',(88.4152890935457,-20.0853834839222,6.82348327324171));
#25079=CARTESIAN_POINT('Ctrl Pts',(88.4549073814603,-20.6490788419189,3.39791756499875));
#25080=CARTESIAN_POINT('Ctrl Pts',(88.4678859719229,-20.8337403096959,2.27573342302018));
#25081=CARTESIAN_POINT('Ctrl Pts',(88.4808645623856,-20.9249529238808,1.13817176694133));
#25082=CARTESIAN_POINT('Ctrl Pts',(88.4938431528482,-20.9240272266393,0.000463189924240194));
#25083=CARTESIAN_POINT('Origin',(80.4,0.,0.));
#25084=CARTESIAN_POINT('',(90.2061568471519,-20.9263865279884,-0.000314477239331534));
#25085=CARTESIAN_POINT('',(89.9938431528482,-20.9266482192657,-0.000185637335865005));
#25086=CARTESIAN_POINT('',(80.4,-20.925,-2.56257342721584E-15));
#25087=CARTESIAN_POINT('Ctrl Pts',(90.2061568471519,-20.9263865279884,-0.000314477239331534));
#25088=CARTESIAN_POINT('Ctrl Pts',(90.1702119581346,-20.9240965220108,3.14960571920385));
#25089=CARTESIAN_POINT('Ctrl Pts',(90.1342670691174,-20.2028316475124,6.30053922034308));
#25090=CARTESIAN_POINT('Ctrl Pts',(90.0983221801002,-18.8279901652861,9.13439032196935));
#25091=CARTESIAN_POINT('Ctrl Pts',(90.0587038921856,-17.3126463384168,12.257847701334));
#25092=CARTESIAN_POINT('Ctrl Pts',(90.019085604271,-15.0033151063425,14.9961024454623));
#25093=CARTESIAN_POINT('Ctrl Pts',(89.9794673163564,-12.1803321236277,17.0167508358796));
#25094=CARTESIAN_POINT('Ctrl Pts',(89.9398490284419,-9.35734914091304,19.0373992262967));
#25095=CARTESIAN_POINT('Ctrl Pts',(89.9002307405273,-6.02071440755794,20.3404412630028));
#25096=CARTESIAN_POINT('Ctrl Pts',(89.8606124526128,-2.57547056647811,20.7676973057411));
#25097=CARTESIAN_POINT('Ctrl Pts',(89.8209941646982,0.86977327460192,21.1949533484794));
#25098=CARTESIAN_POINT('Ctrl Pts',(89.7813758767836,4.42362622340663,20.7464233972499));
#25099=CARTESIAN_POINT('Ctrl Pts',(89.741757588869,7.65467695105084,19.4765556660559));
#25100=CARTESIAN_POINT('Ctrl Pts',(89.7021393009544,10.885727678695,18.2066879348619));
#25101=CARTESIAN_POINT('Ctrl Pts',(89.6625210130398,13.7939761851787,16.1154824237035));
#25102=CARTESIAN_POINT('Ctrl Pts',(89.6229027251253,16.0263827258295,13.4567959274051));
#25103=CARTESIAN_POINT('Ctrl Pts',(89.5832844372107,18.2587892664803,10.7981094311067));
#25104=CARTESIAN_POINT('Ctrl Pts',(89.5436661492961,19.8153538412981,7.57194194966831));
#25105=CARTESIAN_POINT('Ctrl Pts',(89.5040478613815,20.5071210828747,4.16992623257053));
#25106=CARTESIAN_POINT('Ctrl Pts',(89.464429573467,21.1988883244512,0.767910515472837));
#25107=CARTESIAN_POINT('Ctrl Pts',(89.4248112855524,21.0258582327863,-2.80995343728448));
#25108=CARTESIAN_POINT('Ctrl Pts',(89.3851929976378,20.0090353749829,-6.12933954435845));
#25109=CARTESIAN_POINT('Ctrl Pts',(89.3455747097232,18.9922125171794,-9.44872565143252));
#25110=CARTESIAN_POINT('Ctrl Pts',(89.3059564218086,17.1315968932374,-12.5096339128235));
#25111=CARTESIAN_POINT('Ctrl Pts',(89.266338133894,14.653053406303,-14.9404928221193));
#25112=CARTESIAN_POINT('Ctrl Pts',(89.2267198459794,12.1745099193687,-17.3713517314152));
#25113=CARTESIAN_POINT('Ctrl Pts',(89.1871015580649,9.07803856944216,-19.172161288616));
#25114=CARTESIAN_POINT('Ctrl Pts',(89.1474832701503,5.73952795673904,-20.1243166026441));
#25115=CARTESIAN_POINT('Ctrl Pts',(89.1078649822357,2.40101734403591,-21.0764719166722));
#25116=CARTESIAN_POINT('Ctrl Pts',(89.0682466943211,-1.17953253144373,-21.1799729875277));
#25117=CARTESIAN_POINT('Ctrl Pts',(89.0286284064066,-4.5674695356959,-20.4222555545031));
#25118=CARTESIAN_POINT('Ctrl Pts',(88.989010118492,-7.95540653994797,-19.6645381214785));
#25119=CARTESIAN_POINT('Ctrl Pts',(88.9493918305774,-11.1507306729725,-18.0456021845738));
#25120=CARTESIAN_POINT('Ctrl Pts',(88.9097735426628,-13.7655533417224,-15.761974530108));
#25121=CARTESIAN_POINT('Ctrl Pts',(88.8701552547482,-16.3803760104724,-13.4783468756422));
#25122=CARTESIAN_POINT('Ctrl Pts',(88.8305369668336,-18.4146972149476,-10.5300275036151));
#25123=CARTESIAN_POINT('Ctrl Pts',(88.7909186789191,-19.6215654857963,-7.27492046544498));
#25124=CARTESIAN_POINT('Ctrl Pts',(88.7626647349967,-20.4822485248974,-4.95352757950775));
#25125=CARTESIAN_POINT('Ctrl Pts',(88.7344107910742,-20.9220983100175,-2.47610593764071));
#25126=CARTESIAN_POINT('Ctrl Pts',(88.7061568471518,-20.924409432792,0.000516573290169631));
#25127=CARTESIAN_POINT('Ctrl Pts',(88.4938431528482,-20.9240272266393,0.000463189924240194));
#25128=CARTESIAN_POINT('Ctrl Pts',(88.5204828503002,-20.922127151703,-2.33478364350704));
#25129=CARTESIAN_POINT('Ctrl Pts',(88.5471225477521,-20.5320375909792,-4.67064947204017));
#25130=CARTESIAN_POINT('Ctrl Pts',(88.5737622452041,-19.7650918416665,-6.87542328070042));
#25131=CARTESIAN_POINT('Ctrl Pts',(88.6133805331186,-18.6244979003904,-10.1543405317518));
#25132=CARTESIAN_POINT('Ctrl Pts',(88.6529988210332,-16.6503984348114,-13.1433171474505));
#25133=CARTESIAN_POINT('Ctrl Pts',(88.6926171089477,-14.0824344429329,-15.479513589219));
#25134=CARTESIAN_POINT('Ctrl Pts',(88.7322353968623,-11.5144704510542,-17.8157100309874));
#25135=CARTESIAN_POINT('Ctrl Pts',(88.771853684777,-8.35264193287629,-19.4991262988255));
#25136=CARTESIAN_POINT('Ctrl Pts',(88.8114719726915,-4.98077136280933,-20.3254081737541));
#25137=CARTESIAN_POINT('Ctrl Pts',(88.8510902606061,-1.60890079274246,-21.1516900486826));
#25138=CARTESIAN_POINT('Ctrl Pts',(88.8907085485206,1.97301182921349,-21.1208375307015));
#25139=CARTESIAN_POINT('Ctrl Pts',(88.9303268364352,5.33014894170708,-20.2365958861061));
#25140=CARTESIAN_POINT('Ctrl Pts',(88.9699451243498,8.68728605420077,-19.3523542415107));
#25141=CARTESIAN_POINT('Ctrl Pts',(89.0095634122645,11.8196476572324,-17.614723470301));
#25142=CARTESIAN_POINT('Ctrl Pts',(89.049181700179,14.3469883408086,-15.2346390290992));
#25143=CARTESIAN_POINT('Ctrl Pts',(89.0887999880936,16.8743290243847,-12.8545545878973));
#25144=CARTESIAN_POINT('Ctrl Pts',(89.1284182760081,18.7966487885054,-9.83201647670317));
#25145=CARTESIAN_POINT('Ctrl Pts',(89.1680365639226,19.8805923059492,-6.53393835010704));
#25146=CARTESIAN_POINT('Ctrl Pts',(89.2076548518372,20.964535823393,-3.23586022351083));
#25147=CARTESIAN_POINT('Ctrl Pts',(89.2472731397519,21.2101030941599,0.337757918487176));
#25148=CARTESIAN_POINT('Ctrl Pts',(89.2868914276665,20.5874840773349,3.75310540270599));
#25149=CARTESIAN_POINT('Ctrl Pts',(89.3265097155811,19.96486506051,7.16845288692471));
#25150=CARTESIAN_POINT('Ctrl Pts',(89.3661280034956,18.4740597560931,10.425529713364));
#25151=CARTESIAN_POINT('Ctrl Pts',(89.4057462914102,16.2960408441341,13.1289509712044));
#25152=CARTESIAN_POINT('Ctrl Pts',(89.4453645793247,14.1180219321752,15.8323722290448));
#25153=CARTESIAN_POINT('Ctrl Pts',(89.4849828672394,11.252789412674,17.9821379182864));
#25154=CARTESIAN_POINT('Ctrl Pts',(89.5246011551539,8.04816121095532,19.3172824673091));
#25155=CARTESIAN_POINT('Ctrl Pts',(89.5642194430685,4.84353300923676,20.6524270163317));
#25156=CARTESIAN_POINT('Ctrl Pts',(89.6038377309831,1.29950912530069,21.1729504251357));
#25157=CARTESIAN_POINT('Ctrl Pts',(89.6434560188976,-2.15369229061819,20.8156650221266));
#25158=CARTESIAN_POINT('Ctrl Pts',(89.6830743068122,-5.60689370653718,20.4583796191175));
#25159=CARTESIAN_POINT('Ctrl Pts',(89.7226925947269,-8.96927265443904,19.2232854042953));
#25160=CARTESIAN_POINT('Ctrl Pts',(89.7623108826414,-11.8326613287715,17.2603136321663));
#25161=CARTESIAN_POINT('Ctrl Pts',(89.801929170556,-14.6960500031039,15.2973418600373));
#25162=CARTESIAN_POINT('Ctrl Pts',(89.8415474584705,-17.0604484038671,12.6064925306015));
#25163=CARTESIAN_POINT('Ctrl Pts',(89.8811657463851,-18.6388361442031,9.5144147472828));
#25164=CARTESIAN_POINT('Ctrl Pts',(89.9187248818728,-20.1351875039382,6.58304707555306));
#25165=CARTESIAN_POINT('Ctrl Pts',(89.9562840173605,-20.9251103774838,3.29107461363035));
#25166=CARTESIAN_POINT('Ctrl Pts',(89.9938431528482,-20.9266482192657,-0.000185637335865005));
#25167=CARTESIAN_POINT('Origin',(80.4,0.,0.));
#25168=CARTESIAN_POINT('',(91.7061568471519,-20.9232794228044,4.20060754047213E-5));
#25169=CARTESIAN_POINT('',(91.4938431528482,-20.9233577741311,-0.000216749186123405));
#25170=CARTESIAN_POINT('',(80.4,-20.925,-2.56257342721584E-15));
#25171=CARTESIAN_POINT('Ctrl Pts',(91.7061568471519,-20.9232794228044,4.20060754047213E-5));
#25172=CARTESIAN_POINT('Ctrl Pts',(91.6852497010242,-20.9229908458237,1.83290267080309));
#25173=CARTESIAN_POINT('Ctrl Pts',(91.6643425548965,-20.6844852225557,3.66579445525847));
#25174=CARTESIAN_POINT('Ctrl Pts',(91.6434354087688,-20.2086692594407,5.43492192001744));
#25175=CARTESIAN_POINT('Ctrl Pts',(91.6038171208542,-19.307015169212,8.78735466374625));
#25176=CARTESIAN_POINT('Ctrl Pts',(91.5641988329397,-17.5532061518,11.9108168567498));
#25177=CARTESIAN_POINT('Ctrl Pts',(91.5245805450251,-15.1600597681339,14.4258209515636));
#25178=CARTESIAN_POINT('Ctrl Pts',(91.4849622571105,-12.7669133844678,16.9408250463774));
#25179=CARTESIAN_POINT('Ctrl Pts',(91.4453439691959,-9.73442963454778,18.8473710430013));
#25180=CARTESIAN_POINT('Ctrl Pts',(91.4057256812813,-6.43077111619045,19.9141816026769));
#25181=CARTESIAN_POINT('Ctrl Pts',(91.3661073933667,-3.12711259783322,20.9809921623526));
#25182=CARTESIAN_POINT('Ctrl Pts',(91.3264891054521,0.447720688961312,21.2080672850801));
#25183=CARTESIAN_POINT('Ctrl Pts',(91.2868708175375,3.85979173246923,20.5677588081614));
#25184=CARTESIAN_POINT('Ctrl Pts',(91.247252529623,7.27186277597725,19.9274503312428));
#25185=CARTESIAN_POINT('Ctrl Pts',(91.2076342417084,10.5211715761986,18.4197582546779));
#25186=CARTESIAN_POINT('Ctrl Pts',(91.1680159537938,13.2132654327391,16.2277473692253));
#25187=CARTESIAN_POINT('Ctrl Pts',(91.1283976658792,15.9053592892796,14.0357364837727));
#25188=CARTESIAN_POINT('Ctrl Pts',(91.0887793779647,18.0402382021391,11.1594067894323));
#25189=CARTESIAN_POINT('Ctrl Pts',(91.0491610900501,19.3587492228123,7.94790186760101));
#25190=CARTESIAN_POINT('Ctrl Pts',(91.0095428021355,20.6772602434854,4.73639694576969));
#25191=CARTESIAN_POINT('Ctrl Pts',(90.969924514221,21.179403371972,1.18971679644736));
#25192=CARTESIAN_POINT('Ctrl Pts',(90.9303062263064,20.8042193785163,-2.26158706287777));
#25193=CARTESIAN_POINT('Ctrl Pts',(90.8906879383918,20.4290353850607,-5.71289092220279));
#25194=CARTESIAN_POINT('Ctrl Pts',(90.8510696504772,19.1765242696626,-9.06881849153062));
#25195=CARTESIAN_POINT('Ctrl Pts',(90.8114513625626,17.1987329874818,-11.9219906681495));
#25196=CARTESIAN_POINT('Ctrl Pts',(90.7718330746481,15.220941705301,-14.7751628447684));
#25197=CARTESIAN_POINT('Ctrl Pts',(90.7322147867335,12.5178702563374,-17.1255796286783));
#25198=CARTESIAN_POINT('Ctrl Pts',(90.692596498819,9.41765069622895,-18.6879150721364));
#25199=CARTESIAN_POINT('Ctrl Pts',(90.6529782109044,6.31743113612043,-20.2502505155946));
#25200=CARTESIAN_POINT('Ctrl Pts',(90.6133599229898,2.82006346486707,-21.024504618601));
#25201=CARTESIAN_POINT('Ctrl Pts',(90.5737416350752,-0.649897517646015,
-20.9166901267311));
#25202=CARTESIAN_POINT('Ctrl Pts',(90.5341233471605,-4.11985850015881,-20.8088756348612));
#25203=CARTESIAN_POINT('Ctrl Pts',(90.494505059246,-7.56241279393134,-19.8189925481151));
#25204=CARTESIAN_POINT('Ctrl Pts',(90.4548867713314,-10.5596600892345,-18.0672045824493));
#25205=CARTESIAN_POINT('Ctrl Pts',(90.4152684834168,-13.5569073845378,-16.3154166167835));
#25206=CARTESIAN_POINT('Ctrl Pts',(90.3756501955023,-16.1088476813718,-13.8017237721979));
#25207=CARTESIAN_POINT('Ctrl Pts',(90.3360319075877,-17.9056943060018,-10.8312700430694));
#25208=CARTESIAN_POINT('Ctrl Pts',(90.2964136196731,-19.7025409306319,-7.86081631394061));
#25209=CARTESIAN_POINT('Ctrl Pts',(90.2567953317585,-20.7442938830579,-4.43360170026879));
#25210=CARTESIAN_POINT('Ctrl Pts',(90.217177043844,-20.9044921484388,-0.965664386132399));
#25211=CARTESIAN_POINT('Ctrl Pts',(90.2135036449466,-20.9193456961912,-0.644118004993295));
#25212=CARTESIAN_POINT('Ctrl Pts',(90.2098302460492,-20.9266205558477,-0.322221532532826));
#25213=CARTESIAN_POINT('Ctrl Pts',(90.2061568471519,-20.9263865279884,-0.000314477239331534));
#25214=CARTESIAN_POINT('Ctrl Pts',(89.9938431528482,-20.9266482192657,-0.000185637335865005));
#25215=CARTESIAN_POINT('Ctrl Pts',(89.9959023052751,-20.9267325303287,-0.180626599178571));
#25216=CARTESIAN_POINT('Ctrl Pts',(89.997961457702,-20.9244471914867,-0.361065420327887));
#25217=CARTESIAN_POINT('Ctrl Pts',(90.0000206101289,-20.9197786974978,-0.541442561017874));
#25218=CARTESIAN_POINT('Ctrl Pts',(90.0396388980435,-20.8299564305474,-4.01191584879784));
#25219=CARTESIAN_POINT('Ctrl Pts',(90.079257185958,-19.8579348167377,-7.45955618715585));
#25220=CARTESIAN_POINT('Ctrl Pts',(90.1188754738726,-18.121710053413,-10.4658456683132));
#25221=CARTESIAN_POINT('Ctrl Pts',(90.1584937617872,-16.3854852900884,-13.4721351494706));
#25222=CARTESIAN_POINT('Ctrl Pts',(90.1981120497018,-13.8850573772488,-16.0370737734273));
#25223=CARTESIAN_POINT('Ctrl Pts',(90.2377303376164,-10.9239596727245,-17.8492970677619));
#25224=CARTESIAN_POINT('Ctrl Pts',(90.2773486255309,-7.96286196820022,-19.6615203620964));
#25225=CARTESIAN_POINT('Ctrl Pts',(90.3169669134455,-4.54109447199126,-20.7210283268088));
#25226=CARTESIAN_POINT('Ctrl Pts',(90.3565852013601,-1.07403431882255,-20.8992045592561));
#25227=CARTESIAN_POINT('Ctrl Pts',(90.3962034892746,2.39302583434616,-21.0773807917034));
#25228=CARTESIAN_POINT('Ctrl Pts',(90.4358217771892,5.90537864447457,-20.3742252918856));
#25229=CARTESIAN_POINT('Ctrl Pts',(90.4754400651038,9.03665059614102,-18.875095935191));
#25230=CARTESIAN_POINT('Ctrl Pts',(90.5150583530184,12.1679225478073,-17.3759665784964));
#25231=CARTESIAN_POINT('Ctrl Pts',(90.554676640933,14.9181136410116,-15.0808633649252));
#25232=CARTESIAN_POINT('Ctrl Pts',(90.5942949288476,16.9533711204631,-12.2683947106227));
#25233=CARTESIAN_POINT('Ctrl Pts',(90.6339132167621,18.9886285999148,-9.45592605631999));
#25234=CARTESIAN_POINT('Ctrl Pts',(90.6735315046767,20.3089524656136,-6.12609196128567));
#25235=CARTESIAN_POINT('Ctrl Pts',(90.7131497925913,20.7540652241585,-2.68310962666201));
#25236=CARTESIAN_POINT('Ctrl Pts',(90.7527680805059,21.1991779827034,0.75987270796175));
#25237=CARTESIAN_POINT('Ctrl Pts',(90.7923863684204,20.7690796340944,4.31600328217511));
#25238=CARTESIAN_POINT('Ctrl Pts',(90.832004656335,19.5159809054035,7.55359447776977));
#25239=CARTESIAN_POINT('Ctrl Pts',(90.8716229442496,18.2628821767127,10.7911856733641));
#25240=CARTESIAN_POINT('Ctrl Pts',(90.9112412321641,16.1867830679401,13.7102374903398));
#25241=CARTESIAN_POINT('Ctrl Pts',(90.9508595200787,13.5397066043922,15.956398358946));
#25242=CARTESIAN_POINT('Ctrl Pts',(90.9904778079933,10.8926301408442,18.2025592275522));
#25243=CARTESIAN_POINT('Ctrl Pts',(91.0300960959079,7.67457632252076,19.7758291477888));
#25244=CARTESIAN_POINT('Ctrl Pts',(91.0697143838225,4.27619290028805,20.4852255990882));
#25245=CARTESIAN_POINT('Ctrl Pts',(91.1093326717371,0.877809478055243,21.1946220503876));
#25246=CARTESIAN_POINT('Ctrl Pts',(91.1489509596516,-2.70090354808683,21.0401450327498));
#25247=CARTESIAN_POINT('Ctrl Pts',(91.1885692475662,-6.02551691195499,20.0405454316577));
#25248=CARTESIAN_POINT('Ctrl Pts',(91.2281875354808,-9.35013027582305,19.0409458305656));
#25249=CARTESIAN_POINT('Ctrl Pts',(91.2678058233954,-12.4206439774172,17.1962236460193));
#25250=CARTESIAN_POINT('Ctrl Pts',(91.30742411131,-14.8643207022932,14.7303173377137));
#25251=CARTESIAN_POINT('Ctrl Pts',(91.3470423992245,-17.3079974271691,12.2644110294083));
#25252=CARTESIAN_POINT('Ctrl Pts',(91.3866606871391,-19.1248371753269,9.17732059734364));
#25253=CARTESIAN_POINT('Ctrl Pts',(91.4262789750536,-20.0942886764528,5.84379016318228));
#25254=CARTESIAN_POINT('Ctrl Pts',(91.4488003676518,-20.6453826032978,3.94881308069201));
#25255=CARTESIAN_POINT('Ctrl Pts',(91.47132176025,-20.9226462243581,1.97419984397363));
#25256=CARTESIAN_POINT('Ctrl Pts',(91.4938431528482,-20.9233577741311,-0.000216749186123405));
#25257=CARTESIAN_POINT('Origin',(65.9521295958992,0.,0.));
#25258=CARTESIAN_POINT('',(90.7021295958993,-20.0672796057963,-0.000301566765486798));
#25259=CARTESIAN_POINT('',(90.9978704041008,-20.0643751936834,-0.000207850816367205));
#25260=CARTESIAN_POINT('',(65.9521295958992,-20.06595,-1.45722292471193E-12));
#25261=CARTESIAN_POINT('',(92.,-13.2931882197129,15.0310843373919));
#25262=CARTESIAN_POINT('Ctrl Pts',(90.7021295958993,-20.0672796057963,-0.000301566765486157));
#25263=CARTESIAN_POINT('Ctrl Pts',(90.7058029947966,-20.0675040259313,-0.308993125960923));
#25264=CARTESIAN_POINT('Ctrl Pts',(90.7490946816086,-19.9852882243807,-3.94686076179615));
#25265=CARTESIAN_POINT('Ctrl Pts',(90.8320046563349,-17.8946924029286,-10.8246147761969));
#25266=CARTESIAN_POINT('Ctrl Pts',(90.9508595200788,-10.5531717722109,-18.05610365574));
#25267=CARTESIAN_POINT('Ctrl Pts',(91.0697143838226,-0.649498319719339,
-20.9038376377461));
#25268=CARTESIAN_POINT('Ctrl Pts',(91.1885692475662,9.41186437891623,-18.6764334630907));
#25269=CARTESIAN_POINT('Ctrl Pts',(91.30742411131,17.1881649583186,-11.9146634752632));
#25270=CARTESIAN_POINT('Ctrl Pts',(91.4262789750537,20.7914374193968,-2.26020113694711));
#25271=CARTESIAN_POINT('Ctrl Pts',(91.5451338387974,19.3468526295679,7.94302560746775));
#25272=CARTESIAN_POINT('Ctrl Pts',(91.6639887025412,13.2051503325794,16.2177622139406));
#25273=CARTESIAN_POINT('Ctrl Pts',(91.7828435662849,3.85741299640702,20.5551491420764));
#25274=CARTESIAN_POINT('Ctrl Pts',(91.8948473321045,-5.83399714535016,19.9395461276724));
#25275=CARTESIAN_POINT('Ctrl Pts',(91.9672328100095,-11.2292638125539,16.8535785943549));
#25276=CARTESIAN_POINT('Ctrl Pts',(92.,-13.2939520371393,15.0312716283105));
#25277=CARTESIAN_POINT('',(92.,9.87756200380559,17.4664283201654));
#25278=CARTESIAN_POINT('Origin',(92.,0.,0.));
#25279=CARTESIAN_POINT('Ctrl Pts',(90.9978704041008,-20.0643751936834,-0.000207850816367205));
#25280=CARTESIAN_POINT('Ctrl Pts',(91.0149672994172,-20.064893183897,-1.4375331253234));
#25281=CARTESIAN_POINT('Ctrl Pts',(91.0716824826482,-19.5596239647444,-6.20518254004424));
#25282=CARTESIAN_POINT('Ctrl Pts',(91.1680159537938,-15.8234056085072,-13.6752200512566));
#25283=CARTESIAN_POINT('Ctrl Pts',(91.2868708175377,-7.37201867707368,-19.5715898806077));
#25284=CARTESIAN_POINT('Ctrl Pts',(91.4057256812812,2.86917222790772,-20.7161033751214));
#25285=CARTESIAN_POINT('Ctrl Pts',(91.5245805450251,12.4137954244847,-16.8313801312361));
#25286=CARTESIAN_POINT('Ctrl Pts',(91.6434354087687,18.9444853649975,-8.85960809395612));
#25287=CARTESIAN_POINT('Ctrl Pts',(91.7622902725126,20.8758294198323,1.26187795552705));
#25288=CARTESIAN_POINT('Ctrl Pts',(91.8811451362562,17.7386656817295,11.0795895560304));
#25289=CARTESIAN_POINT('Ctrl Pts',(91.9603817120854,12.7761628790883,15.8272202722995));
#25290=CARTESIAN_POINT('Ctrl Pts',(92.,9.87756200380534,17.4664283201656));
#25291=CARTESIAN_POINT('Origin',(65.9521295958992,0.,0.));
#25292=CARTESIAN_POINT('',(89.2021295958992,-20.0653836777985,0.000495366012167058));
#25293=CARTESIAN_POINT('',(89.4978704041008,-20.0675305536619,-0.00017801622778868));
#25294=CARTESIAN_POINT('',(65.9521295958992,-20.06595,-1.45722292471193E-12));
#25295=CARTESIAN_POINT('Ctrl Pts',(89.2021295958992,-20.0653836777985,0.000495366012166348));
#25296=CARTESIAN_POINT('Ctrl Pts',(89.2303835398216,-20.0631674353115,-2.37445247022255));
#25297=CARTESIAN_POINT('Ctrl Pts',(89.2982557716587,-19.0499289088233,-8.08144412695439));
#25298=CARTESIAN_POINT('Ctrl Pts',(89.4057462914101,-13.7570952656821,-15.7522897774154));
#25299=CARTESIAN_POINT('Ctrl Pts',(89.524601155154,-4.56466310983042,-20.4097073491906));
#25300=CARTESIAN_POINT('Ctrl Pts',(89.6434560188976,5.73600137388006,-20.1119514620605));
#25301=CARTESIAN_POINT('Ctrl Pts',(89.7623108826413,14.6440500167558,-14.9313128191482));
#25302=CARTESIAN_POINT('Ctrl Pts',(89.8811657463853,19.996741067543,-6.12557344600731));
#25303=CARTESIAN_POINT('Ctrl Pts',(90.0000206101288,20.4945207331834,4.16736407124383));
#25304=CARTESIAN_POINT('Ctrl Pts',(90.1188754738726,16.0165355102348,13.4485275657482));
#25305=CARTESIAN_POINT('Ctrl Pts',(90.2377303376165,7.64997362942123,19.4645885301395));
#25306=CARTESIAN_POINT('Ctrl Pts',(90.3565852013599,-2.57388810220134,20.7549368562865));
#25307=CARTESIAN_POINT('Ctrl Pts',(90.475440065104,-12.172848063172,17.0062950847534));
#25308=CARTESIAN_POINT('Ctrl Pts',(90.59062152995,-18.6110913235361,9.37224505906302));
#25309=CARTESIAN_POINT('Ctrl Pts',(90.666184706882,-20.0650836131825,3.02030255107542));
#25310=CARTESIAN_POINT('Ctrl Pts',(90.7021295958993,-20.0672796057963,-0.000301566765486157));
#25311=CARTESIAN_POINT('Ctrl Pts',(89.4978704041008,-20.0675305536619,-0.000178016227787951));
#25312=CARTESIAN_POINT('Ctrl Pts',(89.4999295565277,-20.0676114034384,-0.173211197506917));
#25313=CARTESIAN_POINT('Ctrl Pts',(89.5416069968692,-20.0232548899331,-3.67537764220059));
#25314=CARTESIAN_POINT('Ctrl Pts',(89.6229027251253,-18.1105753899303,-10.4594150595525));
#25315=CARTESIAN_POINT('Ctrl Pts',(89.7417575888689,-10.9172475795155,-17.8383297808979));
#25316=CARTESIAN_POINT('Ctrl Pts',(89.8606124526128,-1.07337439090547,-20.886363306994));
#25317=CARTESIAN_POINT('Ctrl Pts',(89.9794673163564,9.03109813531615,-18.8634983461956));
#25318=CARTESIAN_POINT('Ctrl Pts',(90.0983221801003,16.9429543312567,-12.2608565786884));
#25319=CARTESIAN_POINT('Ctrl Pts',(90.2171770438438,20.7413131374097,-2.68146095729082));
#25320=CARTESIAN_POINT('Ctrl Pts',(90.3360319075878,19.5039895591631,7.5489531352732));
#25321=CARTESIAN_POINT('Ctrl Pts',(90.4548867713314,13.531387277919,15.9465943979035));
#25322=CARTESIAN_POINT('Ctrl Pts',(90.5737416350752,4.2735654835411,20.4726382052112));
#25323=CARTESIAN_POINT('Ctrl Pts',(90.6925964988188,-6.021814680891,20.0282327411152));
#25324=CARTESIAN_POINT('Ctrl Pts',(90.8114513625627,-14.8551873562319,14.7212645520118));
#25325=CARTESIAN_POINT('Ctrl Pts',(90.9132093309899,-19.330090149826,7.11771580065352));
#25326=CARTESIAN_POINT('Ctrl Pts',(90.9753490115026,-20.0636928557065,1.89315151059409));
#25327=CARTESIAN_POINT('Ctrl Pts',(90.9978704041008,-20.0643751936834,-0.000207850816367205));
#25328=CARTESIAN_POINT('Origin',(65.9521295958992,0.,0.));
#25329=CARTESIAN_POINT('',(87.7021295958992,-20.0649676983134,-0.000434282711544843));
#25330=CARTESIAN_POINT('',(87.9978704041009,-20.0650171626467,0.000444174233464878));
#25331=CARTESIAN_POINT('',(65.9521295958992,-20.06595,-1.45722292471193E-12));
#25332=CARTESIAN_POINT('Ctrl Pts',(87.7021295958992,-20.0649676983134,-0.000434282711544581));
#25333=CARTESIAN_POINT('Ctrl Pts',(87.7153457969321,-20.065848378389,-1.11141741996506));
#25334=CARTESIAN_POINT('Ctrl Pts',(87.7681802858796,-19.7031926272816,-5.55223264921002));
#25335=CARTESIAN_POINT('Ctrl Pts',(87.8606330627416,-16.4712183986482,-12.887640119355));
#25336=CARTESIAN_POINT('Ctrl Pts',(87.9794879264853,-8.3173102399601,-19.1889200778529));
#25337=CARTESIAN_POINT('Ctrl Pts',(88.0983427902292,1.85591716921299,-20.8314155746315));
#25338=CARTESIAN_POINT('Ctrl Pts',(88.2171976539728,11.5785554866035,-17.4163531264618));
#25339=CARTESIAN_POINT('Ctrl Pts',(88.3360525177166,18.4900927013111,-9.77285911485978));
#25340=CARTESIAN_POINT('Ctrl Pts',(88.4549073814602,20.9125103499811,0.243339770501251));
#25341=CARTESIAN_POINT('Ctrl Pts',(88.5737622452041,18.2576814481021,10.2004593779692));
#25342=CARTESIAN_POINT('Ctrl Pts',(88.6926171089477,11.170158976582,17.6810591260786));
#25343=CARTESIAN_POINT('Ctrl Pts',(88.8114719726915,1.37068800228615,20.868960630139));
#25344=CARTESIAN_POINT('Ctrl Pts',(88.9303268364353,-8.76156563726881,18.9901888080648));
#25345=CARTESIAN_POINT('Ctrl Pts',(89.049181700179,-16.766641421806,12.5008815214899));
#25346=CARTESIAN_POINT('Ctrl Pts',(89.1397826200003,-19.7657518411832,5.24065233111284));
#25347=CARTESIAN_POINT('Ctrl Pts',(89.190765251907,-20.0662750981985,0.955750471229892));
#25348=CARTESIAN_POINT('Ctrl Pts',(89.2021295958992,-20.0653836777985,0.000495366012166348));
#25349=CARTESIAN_POINT('Ctrl Pts',(87.9978704041009,-20.0650171626467,0.000444174233465294));
#25350=CARTESIAN_POINT('Ctrl Pts',(88.0245101015528,-20.0631950929372,-2.23893198812163));
#25351=CARTESIAN_POINT('Ctrl Pts',(88.0907680869193,-19.1327997546737,-7.8101620247403));
#25352=CARTESIAN_POINT('Ctrl Pts',(88.1966443602004,-14.0737816631622,-15.4700023912384));
#25353=CARTESIAN_POINT('Ctrl Pts',(88.3154992239441,-4.97771098870528,-20.312919475056));
#25354=CARTESIAN_POINT('Ctrl Pts',(88.4343540876879,5.32687389681903,-20.2241617570368));
#25355=CARTESIAN_POINT('Ctrl Pts',(88.5532089514316,14.3381730091277,-15.2252782912942));
#25356=CARTESIAN_POINT('Ctrl Pts',(88.6720638151754,19.868376918928,-6.52992365153576));
#25357=CARTESIAN_POINT('Ctrl Pts',(88.790918678919,20.5748343493,3.75079935297009));
#25358=CARTESIAN_POINT('Ctrl Pts',(88.9097735426629,16.2860279409612,13.1208840476639));
#25359=CARTESIAN_POINT('Ctrl Pts',(89.0286284064065,8.04321611663378,19.3054131992102));
#25360=CARTESIAN_POINT('Ctrl Pts',(89.1474832701505,-2.15236898069497,20.8028750909506));
#25361=CARTESIAN_POINT('Ctrl Pts',(89.2663381338938,-11.8253908946233,17.2497082436515));
#25362=CARTESIAN_POINT('Ctrl Pts',(89.383133845211,-18.5095396758491,9.64268344613609));
#25363=CARTESIAN_POINT('Ctrl Pts',(89.4603112686131,-20.0660558460732,3.15596361497391));
#25364=CARTESIAN_POINT('Ctrl Pts',(89.4978704041008,-20.0675305536619,-0.000178016227787951));
#25365=CARTESIAN_POINT('Origin',(65.9521295958992,0.,0.));
#25366=CARTESIAN_POINT('',(86.2021295958992,-20.0675576587757,0.000158315979958626));
#25367=CARTESIAN_POINT('',(86.4978704041008,-20.0653267550518,-0.000489666735370431));
#25368=CARTESIAN_POINT('',(65.9521295958992,-20.06595,-1.45722292471193E-12));
#25369=CARTESIAN_POINT('Ctrl Pts',(86.2021295958992,-20.0675576587757,0.000158315979958117));
#25370=CARTESIAN_POINT('Ctrl Pts',(86.2399263419571,-20.0662194103506,-3.17593753999125));
#25371=CARTESIAN_POINT('Ctrl Pts',(86.3173413759297,-18.4943095347506,-9.68247290148306));
#25372=CARTESIAN_POINT('Ctrl Pts',(86.4343746978168,-11.7738322969147,-17.28494074118));
#25373=CARTESIAN_POINT('Ctrl Pts',(86.5532295615605,-2.09024411951815,-20.8092090888336));
#25374=CARTESIAN_POINT('Ctrl Pts',(86.6720844253043,8.10082424882741,-19.2813108960876));
#25375=CARTESIAN_POINT('Ctrl Pts',(86.7909392890479,16.3251329462566,-13.0721971247768));
#25376=CARTESIAN_POINT('Ctrl Pts',(86.9097941527918,20.5859421139072,-3.68934827101431));
#25377=CARTESIAN_POINT('Ctrl Pts',(87.0286490165353,19.8487906427609,6.58921948350647));
#25378=CARTESIAN_POINT('Ctrl Pts',(87.1475038802793,14.2926479488024,15.2680227270453));
#25379=CARTESIAN_POINT('Ctrl Pts',(87.2663587440228,5.26646286003707,20.2399770831349));
#25380=CARTESIAN_POINT('Ctrl Pts',(87.3852136077667,-5.03834110050527,20.2979659655083));
#25381=CARTESIAN_POINT('Ctrl Pts',(87.5040684715104,-14.1199107603864,15.4279105358017));
#25382=CARTESIAN_POINT('Ctrl Pts',(87.6097071342212,-19.144732578109,7.77022286859828));
#25383=CARTESIAN_POINT('Ctrl Pts',(87.6757275090175,-20.063208358257,2.21898363026297));
#25384=CARTESIAN_POINT('Ctrl Pts',(87.7021295958992,-20.0649676983134,-0.000434282711544581));
#25385=CARTESIAN_POINT('Ctrl Pts',(86.4978704041008,-20.0653267550518,-0.000489666735369598));
#25386=CARTESIAN_POINT('Ctrl Pts',(86.5094723586633,-20.0662222709964,-0.975725602202006));
#25387=CARTESIAN_POINT('Ctrl Pts',(86.5606926011403,-19.7579380015879,-5.28063034010222));
#25388=CARTESIAN_POINT('Ctrl Pts',(86.6515311315318,-16.7292403389556,-12.5508892899555));
#25389=CARTESIAN_POINT('Ctrl Pts',(86.7703859952756,-8.70482382118687,-19.0162653149707));
#25390=CARTESIAN_POINT('Ctrl Pts',(86.8892408590193,1.432994482384,-20.8647748873721));
#25391=CARTESIAN_POINT('Ctrl Pts',(87.0080957227631,11.2229030338076,-17.6476273697347));
#25392=CARTESIAN_POINT('Ctrl Pts',(87.1269505865067,18.2880576096475,-10.1458983413729));
#25393=CARTESIAN_POINT('Ctrl Pts',(87.2458054502506,20.9131437355076,-0.180896062030789));
#25394=CARTESIAN_POINT('Ctrl Pts',(87.3646603139942,18.460829534231,9.82802509130509));
#25395=CARTESIAN_POINT('Ctrl Pts',(87.4835151777381,11.5265004287498,17.4508478921023));
#25396=CARTESIAN_POINT('Ctrl Pts',(87.6023700414816,1.79370841459017,20.8368643132955));
#25397=CARTESIAN_POINT('Ctrl Pts',(87.7212249052256,-8.37456933075415,19.1639999168141));
#25398=CARTESIAN_POINT('Ctrl Pts',(87.8400797689691,-16.5096261697931,12.8384013031585));
#25399=CARTESIAN_POINT('Ctrl Pts',(87.932294935261,-19.7114331280202,5.51225344509298));
#25400=CARTESIAN_POINT('Ctrl Pts',(87.9848918136382,-20.0659048565327,1.09144553246543));
#25401=CARTESIAN_POINT('Ctrl Pts',(87.9978704041009,-20.0650171626467,0.000444174233465294));
#25402=CARTESIAN_POINT('Origin',(65.9521295958992,0.,0.));
#25403=CARTESIAN_POINT('',(84.7021295958992,-20.0643985029825,0.000222280623257588));
#25404=CARTESIAN_POINT('',(84.9978704041008,-20.0673230876221,0.00028466991946835));
#25405=CARTESIAN_POINT('',(65.9521295958992,-20.06595,-1.45722292471193E-12));
#25406=CARTESIAN_POINT('Ctrl Pts',(84.7021295958992,-20.0643985029825,0.000222280623257826));
#25407=CARTESIAN_POINT('Ctrl Pts',(84.7248885990676,-20.0636511338426,-1.91310542372513));
#25408=CARTESIAN_POINT('Ctrl Pts',(84.7872658901506,-19.3192530083258,-7.1576742664364));
#25409=CARTESIAN_POINT('Ctrl Pts',(84.8892614691482,-14.8111651148504,-14.7655576028342));
#25410=CARTESIAN_POINT('Ctrl Pts',(85.0081163328919,-5.96198547260468,-20.0461226327294));
#25411=CARTESIAN_POINT('Ctrl Pts',(85.1269711966356,4.33467558954779,-20.4597871669124));
#25412=CARTESIAN_POINT('Ctrl Pts',(85.2458260603795,13.5789418738155,-15.9061196075446));
#25413=CARTESIAN_POINT('Ctrl Pts',(85.364680924123,19.5264429856993,-7.49068272644153));
#25414=CARTESIAN_POINT('Ctrl Pts',(85.483535787867,20.7332140926975,2.74338053655433));
#25415=CARTESIAN_POINT('Ctrl Pts',(85.6023906516105,16.9062691143363,12.3113917984773));
#25416=CARTESIAN_POINT('Ctrl Pts',(85.7212455153543,8.97473338589818,18.890380198239));
#25417=CARTESIAN_POINT('Ctrl Pts',(85.8401003790982,-1.13573415718418,20.8830651798576));
#25418=CARTESIAN_POINT('Ctrl Pts',(85.9589552428418,-10.9704623349105,17.8056524603926));
#25419=CARTESIAN_POINT('Ctrl Pts',(86.0778101065857,-18.1417253850317,10.4052920879747));
#25420=CARTESIAN_POINT('Ctrl Pts',(86.1588682242713,-20.0286087768165,3.63541879634039));
#25421=CARTESIAN_POINT('Ctrl Pts',(86.2003080540426,-20.0676221530979,0.153224178672827));
#25422=CARTESIAN_POINT('Ctrl Pts',(86.2021295958992,-20.0675576587757,0.000158315979958117));
#25423=CARTESIAN_POINT('Ctrl Pts',(84.9978704041008,-20.0673230876221,0.000284669919469217));
#25424=CARTESIAN_POINT('Ctrl Pts',(85.0340529036883,-20.0652120135904,-3.04026780378225));
#25425=CARTESIAN_POINT('Ctrl Pts',(85.1098536911904,-18.596352367802,-9.4120653334657));
#25426=CARTESIAN_POINT('Ctrl Pts',(85.225272766607,-12.122014753868,-17.0425661974441));
#25427=CARTESIAN_POINT('Ctrl Pts',(85.3441276303508,-2.51190450252216,-20.7625297123801));
#25428=CARTESIAN_POINT('Ctrl Pts',(85.4629824940945,7.70805881080918,-19.4416597454118));
#25429=CARTESIAN_POINT('Ctrl Pts',(85.5818373578382,16.0566200612769,-13.4006438835997));
#25430=CARTESIAN_POINT('Ctrl Pts',(85.700692221582,20.5068727177375,-4.10615095019311));
#25431=CARTESIAN_POINT('Ctrl Pts',(85.8195470853257,19.9783616090541,6.18525437675218));
#25432=CARTESIAN_POINT('Ctrl Pts',(85.9384019490693,14.5994013736218,14.9749719138016));
#25433=CARTESIAN_POINT('Ctrl Pts',(86.0572568128132,5.67592357316316,20.1289889432845));
#25434=CARTESIAN_POINT('Ctrl Pts',(86.1761116765568,-4.62558407166802,20.3959867690482));
#25435=CARTESIAN_POINT('Ctrl Pts',(86.2949665403008,-13.8040686848729,15.7111422891708));
#25436=CARTESIAN_POINT('Ctrl Pts',(86.4022194494818,-19.0623251133496,8.04151842586029));
#25437=CARTESIAN_POINT('Ctrl Pts',(86.4698540707486,-20.0631642682839,2.35450447826081));
#25438=CARTESIAN_POINT('Ctrl Pts',(86.4978704041008,-20.0653267550518,-0.000489666735369598));
#25439=CARTESIAN_POINT('Origin',(65.9521295958992,0.,0.));
#25440=CARTESIAN_POINT('',(83.2021295958992,-20.0663262756018,-0.000495292805329403));
#25441=CARTESIAN_POINT('',(83.4978704041008,-20.0642786305281,0.000103247315883515));
#25442=CARTESIAN_POINT('',(65.9521295958992,-20.06595,-1.45722292471193E-12));
#25443=CARTESIAN_POINT('Ctrl Pts',(83.2021295958992,-20.0663262756018,-0.000495292805329922));
#25444=CARTESIAN_POINT('Ctrl Pts',(83.2098508561781,-20.0669889354332,-0.649435220771842));
#25445=CARTESIAN_POINT('Ctrl Pts',(83.2571904043715,-19.8777692591846,-4.62774326658148));
#25446=CARTESIAN_POINT('Ctrl Pts',(83.3441482404796,-17.3211691177578,-11.7204694349677));
#25447=CARTESIAN_POINT('Ctrl Pts',(83.4630031042234,-9.62145947804478,-18.5693247290879));
#25448=CARTESIAN_POINT('Ctrl Pts',(83.581857967967,0.41419745487271,-20.9098240989816));
#25449=CARTESIAN_POINT('Ctrl Pts',(83.7007128317109,10.3492934047325,-18.1737291001251));
#25450=CARTESIAN_POINT('Ctrl Pts',(83.8195676954545,17.7717348066487,-11.025322913372));
#25451=CARTESIAN_POINT('Ctrl Pts',(83.9384225591984,20.8794632575961,-1.20013226632287));
#25452=CARTESIAN_POINT('Ctrl Pts',(84.057277422942,18.9179685006256,8.91643264940149));
#25453=CARTESIAN_POINT('Ctrl Pts',(84.1761322866858,12.3634722959219,16.8682203023895));
#25454=CARTESIAN_POINT('Ctrl Pts',(84.2949871504295,2.80730885869799,20.7246548910676));
#25455=CARTESIAN_POINT('Ctrl Pts',(84.4138420141732,-7.43042742562143,19.5494514412693));
#25456=CARTESIAN_POINT('Ctrl Pts',(84.532696877917,-15.8641664191098,13.6279318757016));
#25457=CARTESIAN_POINT('Ctrl Pts',(84.6287927384923,-19.5689046288147,6.16520005828642));
#25458=CARTESIAN_POINT('Ctrl Pts',(84.685270311153,-20.0649521348374,1.41756628034156));
#25459=CARTESIAN_POINT('Ctrl Pts',(84.7021295958992,-20.0643985029825,0.000222280623257826));
#25460=CARTESIAN_POINT('Ctrl Pts',(83.4978704041008,-20.0642786305281,0.000103247315884208));
#25461=CARTESIAN_POINT('Ctrl Pts',(83.5190151607988,-20.0639584731567,-1.77754669223435));
#25462=CARTESIAN_POINT('Ctrl Pts',(83.5797782054113,-19.3915725094379,-6.88616286129953));
#25463=CARTESIAN_POINT('Ctrl Pts',(83.6801595379384,-15.1076199452285,-14.4620926520955));
#25464=CARTESIAN_POINT('Ctrl Pts',(83.7990144016822,-6.36737098063297,-19.9210665146787));
#25465=CARTESIAN_POINT('Ctrl Pts',(83.9178692654259,3.91878097726412,-20.5435016474673));
#25466=CARTESIAN_POINT('Ctrl Pts',(84.0367241291697,13.2535111849172,-16.1782800556342));
#25467=CARTESIAN_POINT('Ctrl Pts',(84.1555789929134,19.3704859523993,-7.88521263220971));
#25468=CARTESIAN_POINT('Ctrl Pts',(84.2744338566571,20.7845947636492,2.32226716769303));
#25469=CARTESIAN_POINT('Ctrl Pts',(84.3932887204008,17.152513026647,11.9659350306595));
#25470=CARTESIAN_POINT('Ctrl Pts',(84.5121435841446,9.3560561792281,18.7044517978578));
#25471=CARTESIAN_POINT('Ctrl Pts',(84.6309984478883,-0.711911986905901,
20.901805797829));
#25472=CARTESIAN_POINT('Ctrl Pts',(84.7498533116321,-10.6070385085257,18.0245121533403));
#25473=CARTESIAN_POINT('Ctrl Pts',(84.8687081753758,-17.9269338035892,10.7711349768254));
#25474=CARTESIAN_POINT('Ctrl Pts',(84.951380539532,-19.9910515517318,3.90689779358534));
#25475=CARTESIAN_POINT('Ctrl Pts',(84.9944346157737,-20.0675235492706,0.289006975347951));
#25476=CARTESIAN_POINT('Ctrl Pts',(84.9978704041008,-20.0673230876221,0.000284669919469217));
#25477=CARTESIAN_POINT('Origin',(65.9521295958992,0.,0.));
#25478=CARTESIAN_POINT('',(81.7021295958993,-20.0664325672107,0.000484799890657325));
#25479=CARTESIAN_POINT('',(81.9978704041008,-20.0667413636039,-0.000441116259225494));
#25480=CARTESIAN_POINT('',(65.9521295958992,-20.06595,-1.45722292471193E-12));
#25481=CARTESIAN_POINT('Ctrl Pts',(81.7021295958993,-20.0664325672107,0.000484799890658819));
#25482=CARTESIAN_POINT('Ctrl Pts',(81.7344314012032,-20.0636845251475,-2.71430660379001));
#25483=CARTESIAN_POINT('Ctrl Pts',(81.8063514944216,-18.8281343099021,-8.76122511579918));
#25484=CARTESIAN_POINT('Ctrl Pts',(81.9178898755548,-12.9383761771515,-16.4313945020042));
#25485=CARTESIAN_POINT('Ctrl Pts',(82.0367447392985,-3.52102754484433,-20.6153988176417));
#25486=CARTESIAN_POINT('Ctrl Pts',(82.1555996030423,6.75117421878302,-19.7942908448273));
#25487=CARTESIAN_POINT('Ctrl Pts',(82.274454466786,15.3842912699189,-14.1674233897442));
#25488=CARTESIAN_POINT('Ctrl Pts',(82.3933093305298,20.2823311602726,-5.10091620074396));
#25489=CARTESIAN_POINT('Ctrl Pts',(82.5121641942734,20.2561226367727,5.20401759278348));
#25490=CARTESIAN_POINT('Ctrl Pts',(82.6310190580173,15.3120287392127,14.2454932968817));
#25491=CARTESIAN_POINT('Ctrl Pts',(82.7498739217609,6.65040194880476,19.8283750544846));
#25492=CARTESIAN_POINT('Ctrl Pts',(82.8687287855047,-3.62584354539574,20.5972221905355));
#25493=CARTESIAN_POINT('Ctrl Pts',(82.9875836492484,-13.0217881419229,16.3653700529151));
#25494=CARTESIAN_POINT('Ctrl Pts',(83.0987172527133,-18.8512229442922,8.69328500138972));
#25495=CARTESIAN_POINT('Ctrl Pts',(83.1702325682635,-20.0635887848047,2.68031769219749));
#25496=CARTESIAN_POINT('Ctrl Pts',(83.2021295958992,-20.0663262756018,-0.000495292805329922));
#25497=CARTESIAN_POINT('Ctrl Pts',(81.9978704041008,-20.0667413636039,-0.000441116259225702));
#25498=CARTESIAN_POINT('Ctrl Pts',(82.0039774179092,-20.0672340924104,-0.513679681067149));
#25499=CARTESIAN_POINT('Ctrl Pts',(82.0497027196323,-19.9227688913182,-4.35619568812115));
#25500=CARTESIAN_POINT('Ctrl Pts',(82.1350463092699,-17.5553415020576,-11.3667184813117));
#25501=CARTESIAN_POINT('Ctrl Pts',(82.2539011730136,-9.99613698190578,-18.3703443006992));
#25502=CARTESIAN_POINT('Ctrl Pts',(82.3727560367574,-0.0100190419482207,
-20.9139236850969));
#25503=CARTESIAN_POINT('Ctrl Pts',(82.4916109005011,9.9785313724145,-18.3799133821952));
#25504=CARTESIAN_POINT('Ctrl Pts',(82.6104657642448,17.544442747166,-11.3835334136054));
#25505=CARTESIAN_POINT('Ctrl Pts',(82.7293206279886,20.8508243032301,-1.62340080174));
#25506=CARTESIAN_POINT('Ctrl Pts',(82.8481754917323,19.0949357636439,8.53086938533054));
#25507=CARTESIAN_POINT('Ctrl Pts',(82.9670303554759,12.7030807563111,16.6139713369771));
#25508=CARTESIAN_POINT('Ctrl Pts',(83.0858852192198,3.22710663214606,20.6634480925139));
#25509=CARTESIAN_POINT('Ctrl Pts',(83.2047400829634,-7.03236099624711,19.6961469101375));
#25510=CARTESIAN_POINT('Ctrl Pts',(83.3235949467073,-15.5844759437393,13.9469141334658));
#25511=CARTESIAN_POINT('Ctrl Pts',(83.4213050537529,-19.5045880027386,6.43679091069946));
#25512=CARTESIAN_POINT('Ctrl Pts',(83.4793968728842,-20.0645583422922,1.5531819665273));
#25513=CARTESIAN_POINT('Ctrl Pts',(83.4978704041008,-20.0642786305281,0.000103247315884208));
#25514=CARTESIAN_POINT('Origin',(65.9521295958992,0.,0.));
#25515=CARTESIAN_POINT('',(80.2021295958992,-20.0643601951534,-0.000193369559137528));
#25516=CARTESIAN_POINT('',(80.4978704041008,-20.0660058932225,0.000514059632016062));
#25517=CARTESIAN_POINT('',(65.9521295958992,-20.06595,-1.45722292471193E-12));
#25518=CARTESIAN_POINT('Ctrl Pts',(80.2021295958992,-20.0643601951534,-0.000193369559138151));
#25519=CARTESIAN_POINT('Ctrl Pts',(80.2193936583136,-20.0648522124826,-1.45157457243224));
#25520=CARTESIAN_POINT('Ctrl Pts',(80.2762760086426,-19.5530566810888,-6.23330384825486));
#25521=CARTESIAN_POINT('Ctrl Pts',(80.3727766468861,-15.7946418386806,-13.7084496778365));
#25522=CARTESIAN_POINT('Ctrl Pts',(80.49163151063,-7.33089175974107,-19.586993883415));
#25523=CARTESIAN_POINT('Ctrl Pts',(80.6104863743736,2.91268983041759,-20.7101072265152));
#25524=CARTESIAN_POINT('Ctrl Pts',(80.7293412381174,12.4491136405291,-16.8051144877733));
#25525=CARTESIAN_POINT('Ctrl Pts',(80.8481961018612,18.9630777731095,-8.82008983814658));
#25526=CARTESIAN_POINT('Ctrl Pts',(80.9670509656049,20.8730885973582,1.30632147223087));
#25527=CARTESIAN_POINT('Ctrl Pts',(81.0859058293486,17.7154238864056,11.1155773537385));
#25528=CARTESIAN_POINT('Ctrl Pts',(81.2047606930925,10.2567176785937,18.2261363388843));
#25529=CARTESIAN_POINT('Ctrl Pts',(81.323615556836,0.307832932572739,20.9116604378418));
#25530=CARTESIAN_POINT('Ctrl Pts',(81.44247042058,-9.71578907209836,18.5201443322797));
#25531=CARTESIAN_POINT('Ctrl Pts',(81.5613252843235,-17.3805619607799,11.6322125715389));
#25532=CARTESIAN_POINT('Ctrl Pts',(81.6478783427634,-19.8893188630231,4.55964969297058));
#25533=CARTESIAN_POINT('Ctrl Pts',(81.6948131132886,-20.0670550092625,0.615395449919073));
#25534=CARTESIAN_POINT('Ctrl Pts',(81.7021295958993,-20.0664325672107,0.000484799890658819));
#25535=CARTESIAN_POINT('Ctrl Pts',(80.4978704041008,-20.0660058932225,0.00051405963201627));
#25536=CARTESIAN_POINT('Ctrl Pts',(80.5285579629343,-20.0633649888413,-2.57876672415488));
#25537=CARTESIAN_POINT('Ctrl Pts',(80.5988638096823,-18.9190011292246,-8.490229143316));
#25538=CARTESIAN_POINT('Ctrl Pts',(80.708787944345,-13.2690058590392,-16.1655741562136));
#25539=CARTESIAN_POINT('Ctrl Pts',(80.8276428080888,-3.93846234853991,-20.5397375498421));
#25540=CARTESIAN_POINT('Ctrl Pts',(80.9464976718324,6.34828125649317,-19.9271580857812));
#25541=CARTESIAN_POINT('Ctrl Pts',(81.0653525355762,15.0937565693877,-14.4765609490419));
#25542=CARTESIAN_POINT('Ctrl Pts',(81.1842073993199,20.1746922266295,-5.51127007576585));
#25543=CARTESIAN_POINT('Ctrl Pts',(81.3030622630637,20.3575126025494,4.7920752210601));
#25544=CARTESIAN_POINT('Ctrl Pts',(81.4219171268074,15.5978316283554,13.9319759108582));
#25545=CARTESIAN_POINT('Ctrl Pts',(81.5407719905512,7.05122906962834,19.6894000135831));
#25546=CARTESIAN_POINT('Ctrl Pts',(81.6596268542949,-3.20730705765452,20.6665305681718));
#25547=CARTESIAN_POINT('Ctrl Pts',(81.7784817180386,-12.6871567229822,16.6261348055928));
#25548=CARTESIAN_POINT('Ctrl Pts',(81.891229567974,-18.7579286033266,8.96417271615029));
#25549=CARTESIAN_POINT('Ctrl Pts',(81.9643591299947,-20.06403759207,2.81587447866636));
#25550=CARTESIAN_POINT('Ctrl Pts',(81.9978704041008,-20.0667413636039,-0.000441116259225702));
#25551=CARTESIAN_POINT('Origin',(65.9521295958992,0.,0.));
#25552=CARTESIAN_POINT('',(78.7021295958992,-20.0675097952894,-0.000191679329453545));
#25553=CARTESIAN_POINT('',(78.9978704041008,-20.0645444704692,-0.000303457117966088));
#25554=CARTESIAN_POINT('',(65.9521295958992,-20.06595,-1.45722292471193E-12));
#25555=CARTESIAN_POINT('Ctrl Pts',(78.7021295958992,-20.0675097952894,-0.000191679329453777));
#25556=CARTESIAN_POINT('Ctrl Pts',(78.7043559154241,-20.0676030240896,-0.187272685098598));
#25557=CARTESIAN_POINT('Ctrl Pts',(78.7462005228635,-20.0194521966627,-3.70349040917738));
#25558=CARTESIAN_POINT('Ctrl Pts',(78.8276634182176,-18.0885635049867,-10.4974365303172));
#25559=CARTESIAN_POINT('Ctrl Pts',(78.9465182819614,-10.8797508184065,-17.8612240765116));
#25560=CARTESIAN_POINT('Ctrl Pts',(79.0653731457051,-1.02949641157685,-20.8885720076918));
#25561=CARTESIAN_POINT('Ctrl Pts',(79.1842280094488,9.07070441569705,-18.8444852618751));
#25562=CARTESIAN_POINT('Ctrl Pts',(79.3030828731926,16.9686730893506,-12.2252377060213));
#25563=CARTESIAN_POINT('Ctrl Pts',(79.4219377369363,20.7469002557211,-2.63788422057037));
#25564=CARTESIAN_POINT('Ctrl Pts',(79.5407926006801,19.488088539859,7.58990832912952));
#25565=CARTESIAN_POINT('Ctrl Pts',(79.6596474644237,13.4978587082429,15.9749839960573));
#25566=CARTESIAN_POINT('Ctrl Pts',(79.7785023281676,4.23054949116273,20.4815710917107));
#25567=CARTESIAN_POINT('Ctrl Pts',(79.8973571919112,-6.06387423543652,20.0155372807922));
#25568=CARTESIAN_POINT('Ctrl Pts',(80.0162120556551,-14.8860794655671,14.6900286428174));
#25569=CARTESIAN_POINT('Ctrl Pts',(80.1178028569843,-19.3376741497113,7.0895961574771));
#25570=CARTESIAN_POINT('Ctrl Pts',(80.179775370399,-20.0637231106675,1.87911533061271));
#25571=CARTESIAN_POINT('Ctrl Pts',(80.2021295958992,-20.0643601951534,-0.000193369559138151));
#25572=CARTESIAN_POINT('Ctrl Pts',(78.9978704041008,-20.0645444704692,-0.000303457117966088));
#25573=CARTESIAN_POINT('Ctrl Pts',(79.0135202200448,-20.0652525743057,-1.31594117297544));
#25574=CARTESIAN_POINT('Ctrl Pts',(79.0687883239033,-19.6151483119908,-5.96170308847767));
#25575=CARTESIAN_POINT('Ctrl Pts',(79.1636747156764,-16.0694521359249,-13.3852535403135));
#25576=CARTESIAN_POINT('Ctrl Pts',(79.2825295794202,-7.72668274442983,-19.4342655650835));
#25577=CARTESIAN_POINT('Ctrl Pts',(79.401384443164,2.49201032407988,-20.7649268920441));
#25578=CARTESIAN_POINT('Ctrl Pts',(79.5202393069076,12.1056803413097,-17.0541727375234));
#25579=CARTESIAN_POINT('Ctrl Pts',(79.6390941706514,18.7802711793142,-9.20291903249607));
#25580=CARTESIAN_POINT('Ctrl Pts',(79.7579490343951,20.8952914316842,0.882666569120876));
#25581=CARTESIAN_POINT('Ctrl Pts',(79.8768038981389,17.9372456308276,10.7539538527284));
#25582=CARTESIAN_POINT('Ctrl Pts',(79.9956587618826,10.6243033119855,18.014341048792));
#25583=CARTESIAN_POINT('Ctrl Pts',(80.1145136256262,0.731938129029032,20.9011141057727));
#25584=CARTESIAN_POINT('Ctrl Pts',(80.2333684893701,-9.33813074796676,18.7134074508395));
#25585=CARTESIAN_POINT('Ctrl Pts',(80.3522233531138,-17.1410403344121,11.982363729303));
#25586=CARTESIAN_POINT('Ctrl Pts',(80.4403906580241,-19.842194915655,4.83121342860229));
#25587=CARTESIAN_POINT('Ctrl Pts',(80.4889396750197,-20.0667744522885,0.751139354692291));
#25588=CARTESIAN_POINT('Ctrl Pts',(80.4978704041008,-20.0660058932225,0.00051405963201627));
#25589=CARTESIAN_POINT('Origin',(65.9521295958992,0.,0.));
#25590=CARTESIAN_POINT('',(77.2021295958992,-20.0650526848319,0.000450787506038296));
#25591=CARTESIAN_POINT('',(77.4978704041008,-20.0676486395731,-5.41331433023817E-5));
#25592=CARTESIAN_POINT('',(65.9521295958992,-20.06595,-1.45722292471193E-12));
#25593=CARTESIAN_POINT('Ctrl Pts',(77.2021295958992,-20.0650526848319,0.00045078750603833));
#25594=CARTESIAN_POINT('Ctrl Pts',(77.2289364604492,-20.0631870683403,-2.25296626175112));
#25595=CARTESIAN_POINT('Ctrl Pts',(77.2953616129137,-19.1243638779595,-7.83825946812389));
#25596=CARTESIAN_POINT('Ctrl Pts',(77.4014050532927,-14.0412530376615,-15.4995327837435));
#25597=CARTESIAN_POINT('Ctrl Pts',(77.5202599170366,-4.93502901298443,-20.323331223571));
#25598=CARTESIAN_POINT('Ctrl Pts',(77.6391147807802,5.3693466737219,-20.2129270438343));
#25599=CARTESIAN_POINT('Ctrl Pts',(77.7579696445241,14.3701248285384,-15.1951247376979));
#25600=CARTESIAN_POINT('Ctrl Pts',(77.8768245082677,19.8820503542049,-6.48817209195593));
#25601=CARTESIAN_POINT('Ctrl Pts',(77.9956793720115,20.566909693682,3.79401226064252));
#25602=CARTESIAN_POINT('Ctrl Pts',(78.1145342357552,16.2584291829867,13.1550668521213));
#25603=CARTESIAN_POINT('Ctrl Pts',(78.2333890994989,8.002643824371,19.3222668235958));
#25604=CARTESIAN_POINT('Ctrl Pts',(78.3522439632428,-2.19606445801497,20.7983077263084));
#25605=CARTESIAN_POINT('Ctrl Pts',(78.4710988269864,-11.8616009447801,17.2248287773426));
#25606=CARTESIAN_POINT('Ctrl Pts',(78.5877273712053,-18.5202110494551,9.61468733910552));
#25607=CARTESIAN_POINT('Ctrl Pts',(78.6647376275095,-20.0659439785636,3.14191212734159));
#25608=CARTESIAN_POINT('Ctrl Pts',(78.7021295958992,-20.0675097952894,-0.000191679329453777));
#25609=CARTESIAN_POINT('Ctrl Pts',(77.4978704041008,-20.0676486395731,-5.41331433030149E-5));
#25610=CARTESIAN_POINT('Ctrl Pts',(77.4984824771553,-20.0676566429987,-0.051486524418573));
#25611=CARTESIAN_POINT('Ctrl Pts',(77.5387128381243,-20.0549310784319,-3.43203271481463));
#25612=CARTESIAN_POINT('Ctrl Pts',(77.6185614870079,-18.2977702184867,-10.1283715037868));
#25613=CARTESIAN_POINT('Ctrl Pts',(77.7374163507516,-11.2398064531836,-17.636866365152));
#25614=CARTESIAN_POINT('Ctrl Pts',(77.8562712144954,-1.45298481342087,-20.8633923276927));
#25615=CARTESIAN_POINT('Ctrl Pts',(77.975126078239,8.68659993361501,-19.0245968651264));
#25616=CARTESIAN_POINT('Ctrl Pts',(78.0939809419828,16.7172073837676,-12.5669121734563));
#25617=CARTESIAN_POINT('Ctrl Pts',(78.2128358057265,20.6891254607372,-3.05816807208725));
#25618=CARTESIAN_POINT('Ctrl Pts',(78.3316906694703,19.6380315166033,7.19305376319089));
#25619=CARTESIAN_POINT('Ctrl Pts',(78.450545533214,13.8191155315665,15.6979091032047));
#25620=CARTESIAN_POINT('Ctrl Pts',(78.5694003969578,4.6451237813503,20.3915455359125));
#25621=CARTESIAN_POINT('Ctrl Pts',(78.6882552607015,-5.65663495145375,20.1344179283447));
#25622=CARTESIAN_POINT('Ctrl Pts',(78.8071101244452,-14.5850468304206,14.9889530402125));
#25623=CARTESIAN_POINT('Ctrl Pts',(78.910315172245,-19.2630610848218,7.36107071340815));
#25624=CARTESIAN_POINT('Ctrl Pts',(78.9739019321302,-20.0634599742031,2.01466118073625));
#25625=CARTESIAN_POINT('Ctrl Pts',(78.9978704041008,-20.0645444704692,-0.000303457117966088));
#25626=CARTESIAN_POINT('Origin',(65.9521295958992,0.,0.));
#25627=CARTESIAN_POINT('',(75.7021295958992,-20.0652872327308,-0.000485265228740224));
#25628=CARTESIAN_POINT('',(75.9978704041008,-20.0647373073215,0.000375534437402902));
#25629=CARTESIAN_POINT('',(65.9521295958992,-20.06595,-1.45722292471193E-12));
#25630=CARTESIAN_POINT('Ctrl Pts',(75.7021295958992,-20.0652872327308,-0.000485265228740428));
#25631=CARTESIAN_POINT('Ctrl Pts',(75.7138987175596,-20.0661846979473,-0.989778505806707));
#25632=CARTESIAN_POINT('Ctrl Pts',(75.7652861271346,-19.752403164384,-5.30875635559926));
#25633=CARTESIAN_POINT('Ctrl Pts',(75.8562918246243,-16.7028379804262,-12.5860044009848));
#25634=CARTESIAN_POINT('Ctrl Pts',(75.9751466883679,-8.66485747623899,-19.0345094052471));
#25635=CARTESIAN_POINT('Ctrl Pts',(76.0940015521117,1.47682157948402,-20.8617185630606));
#25636=CARTESIAN_POINT('Ctrl Pts',(76.2128564158554,11.2599503155789,-17.6240126609314));
#25637=CARTESIAN_POINT('Ctrl Pts',(76.3317112795992,18.3093305469575,-10.1074585482319));
#25638=CARTESIAN_POINT('Ctrl Pts',(76.4505661433428,20.9134775754992,-0.136963794739155));
#25639=CARTESIAN_POINT('Ctrl Pts',(76.5694210070867,18.4401432255183,9.86678373150789));
#25640=CARTESIAN_POINT('Ctrl Pts',(76.6882758708303,11.4898162994893,17.4750228837036));
#25641=CARTESIAN_POINT('Ctrl Pts',(76.8071307345741,1.74993282588505,20.8405863278091));
#25642=CARTESIAN_POINT('Ctrl Pts',(76.9259855983178,-8.41480831689548,19.1463653044614));
#25643=CARTESIAN_POINT('Ctrl Pts',(77.0448404620616,-16.5365591258767,12.8036914855974));
#25644=CARTESIAN_POINT('Ctrl Pts',(77.1368884612554,-19.7171928032765,5.4841267812297));
#25645=CARTESIAN_POINT('Ctrl Pts',(77.1893181725346,-20.0659442923776,1.07739433610062));
#25646=CARTESIAN_POINT('Ctrl Pts',(77.2021295958992,-20.0650526848319,0.00045078750603833));
#25647=CARTESIAN_POINT('Ctrl Pts',(75.9978704041008,-20.0647373073215,0.000375534437402764));
#25648=CARTESIAN_POINT('Ctrl Pts',(76.0230630221803,-20.0633086611632,-2.11744145806295));
#25649=CARTESIAN_POINT('Ctrl Pts',(76.0878739281744,-19.2044230293602,-7.566900804634));
#25650=CARTESIAN_POINT('Ctrl Pts',(76.192303122083,-14.352754093941,-15.2115335915258));
#25651=CARTESIAN_POINT('Ctrl Pts',(76.3111579858267,-5.34624865537712,-20.2190486819271));
#25652=CARTESIAN_POINT('Ctrl Pts',(76.4300128495705,4.95824645968282,-20.3176794032267));
#25653=CARTESIAN_POINT('Ctrl Pts',(76.5488677133142,14.0589530618911,-15.4834796829007));
#25654=CARTESIAN_POINT('Ctrl Pts',(76.667722577058,19.7463549128656,-6.8901213300209));
#25655=CARTESIAN_POINT('Ctrl Pts',(76.7865774408017,20.6396354130593,3.3760560278593));
#25656=CARTESIAN_POINT('Ctrl Pts',(76.9054323045454,16.5219193398244,12.8225771830625));
#25657=CARTESIAN_POINT('Ctrl Pts',(77.0242871682892,8.39292692660435,19.1559672658923));
#25658=CARTESIAN_POINT('Ctrl Pts',(77.1431420320329,-1.77374334422174,20.8385733397488));
#25659=CARTESIAN_POINT('Ctrl Pts',(77.2619968957766,-11.5097751060743,17.4618836697204));
#25660=CARTESIAN_POINT('Ctrl Pts',(77.380239686466,-18.4156569494689,9.88492971059405));
#25661=CARTESIAN_POINT('Ctrl Pts',(77.4588641892407,-20.0671385969634,3.27763125149108));
#25662=CARTESIAN_POINT('Ctrl Pts',(77.4978704041008,-20.0676486395731,-5.41331433030149E-5));
#25663=CARTESIAN_POINT('Origin',(65.9521295958992,0.,0.));
#25664=CARTESIAN_POINT('',(74.2021295958992,-20.0673524071727,0.000272503390984278));
#25665=CARTESIAN_POINT('',(74.4978704041008,-20.0656858399569,-0.000513895107878692));
#25666=CARTESIAN_POINT('',(65.9521295958992,-20.06595,-1.45722292471193E-12));
#25667=CARTESIAN_POINT('Ctrl Pts',(74.2021295958992,-20.0673524071727,0.000272503390984676));
#25668=CARTESIAN_POINT('Ctrl Pts',(74.2384792625847,-20.0653052780391,-3.05431469277528));
#25669=CARTESIAN_POINT('Ctrl Pts',(74.3144472171848,-18.5859398545859,-9.44007767698859));
#25670=CARTESIAN_POINT('Ctrl Pts',(74.4300334596993,-12.0861869801001,-17.0679930766342));
#25671=CARTESIAN_POINT('Ctrl Pts',(74.5488883234432,-2.46828348179083,-20.7677605926949));
#25672=CARTESIAN_POINT('Ctrl Pts',(74.6677431871868,7.74888254330118,-19.4254246468925));
#25673=CARTESIAN_POINT('Ctrl Pts',(74.7865980509306,16.0847351103166,-13.3668844467559));
#25674=CARTESIAN_POINT('Ctrl Pts',(74.9054529146743,20.5154531674799,-4.06306346429831));
#25675=CARTESIAN_POINT('Ctrl Pts',(75.024307778418,19.9653242538903,6.22720891081994));
#25676=CARTESIAN_POINT('Ctrl Pts',(75.1431626421618,14.5679114895243,15.0056075590215));
#25677=CARTESIAN_POINT('Ctrl Pts',(75.2620175059054,5.63362643574612,20.1408678205393));
#25678=CARTESIAN_POINT('Ctrl Pts',(75.3808723696493,-4.66841934638479,20.3862248635758));
#25679=CARTESIAN_POINT('Ctrl Pts',(75.499727233393,-13.8370423291352,15.6821096464633));
#25680=CARTESIAN_POINT('Ctrl Pts',(75.6068129754763,-19.0710051864169,8.01342804802537));
#25681=CARTESIAN_POINT('Ctrl Pts',(75.6742804296451,-20.0631635688974,2.34047039194829));
#25682=CARTESIAN_POINT('Ctrl Pts',(75.7021295958992,-20.0652872327308,-0.000485265228740428));
#25683=CARTESIAN_POINT('Ctrl Pts',(74.4978704041009,-20.0656858399569,-0.000513895107878137));
#25684=CARTESIAN_POINT('Ctrl Pts',(74.5080252792908,-20.0665335258616,-0.854067493707957));
#25685=CARTESIAN_POINT('Ctrl Pts',(74.5577984423954,-19.8045579242786,-5.03716326470863));
#25686=CARTESIAN_POINT('Ctrl Pts',(74.6471898934143,-16.9546939409116,-12.2446174973853));
#25687=CARTESIAN_POINT('Ctrl Pts',(74.7660447571583,-9.04916751458383,-18.8548368218943));
#25688=CARTESIAN_POINT('Ctrl Pts',(74.8848996209018,1.05336222602103,-20.8873821315178));
#25689=CARTESIAN_POINT('Ctrl Pts',(75.0037544846458,10.9001512813116,-17.8487816483865));
#25690=CARTESIAN_POINT('Ctrl Pts',(75.1226093483893,18.1005456873079,-10.4767623867747));
#25691=CARTESIAN_POINT('Ctrl Pts',(75.2414642121331,20.9063967498254,-0.561141003802912));
#25692=CARTESIAN_POINT('Ctrl Pts',(75.3603190758769,18.6364855530042,9.4907170709027));
#25693=CARTESIAN_POINT('Ctrl Pts',(75.4791739396206,11.8419127825698,17.2383701647594));
#25694=CARTESIAN_POINT('Ctrl Pts',(75.5980288033644,2.1722996740317,20.8008033117344));
#25695=CARTESIAN_POINT('Ctrl Pts',(75.7168836671081,-8.02471549395103,19.3131107159981));
#25696=CARTESIAN_POINT('Ctrl Pts',(75.8357385308518,-16.2734490649882,13.1364820182761));
#25697=CARTESIAN_POINT('Ctrl Pts',(75.929400776516,-19.6602681817825,5.7557332003338));
#25698=CARTESIAN_POINT('Ctrl Pts',(75.9834447342657,-20.0655553714753,1.21306921353621));
#25699=CARTESIAN_POINT('Ctrl Pts',(75.9978704041008,-20.0647373073215,0.000375534437402764));
#25700=CARTESIAN_POINT('Origin',(65.9521295958992,0.,0.));
#25701=CARTESIAN_POINT('',(72.7021295958992,-20.0642869035746,0.000115967843645696));
#25702=CARTESIAN_POINT('',(72.9978704041008,-20.0670305035468,0.000378951515905696));
#25703=CARTESIAN_POINT('',(65.9521295958992,-20.06595,-1.45722292471193E-12));
#25704=CARTESIAN_POINT('Ctrl Pts',(72.7021295958992,-20.0642869035746,0.000115967843645898));
#25705=CARTESIAN_POINT('Ctrl Pts',(72.7234415196951,-20.0639242759761,-1.7915856698192));
#25706=CARTESIAN_POINT('Ctrl Pts',(72.7843717314056,-19.3842247051702,-6.91428185345562));
#25707=CARTESIAN_POINT('Ctrl Pts',(72.8849202310308,-15.0772063355693,-14.4937970351682));
#25708=CARTESIAN_POINT('Ctrl Pts',(73.0037750947745,-6.32550909580307,-19.9343983621499));
#25709=CARTESIAN_POINT('Ctrl Pts',(73.1226299585183,3.96192769410095,-20.5352241850118));
#25710=CARTESIAN_POINT('Ctrl Pts',(73.241484822262,13.2874673524912,-16.1504029280528));
#25711=CARTESIAN_POINT('Ctrl Pts',(73.3603396860058,19.3870075181409,-7.84450399155505));
#25712=CARTESIAN_POINT('Ctrl Pts',(73.4791945497494,20.7796705370668,2.36592386879463));
#25713=CARTESIAN_POINT('Ctrl Pts',(73.5980494134933,17.1273385367331,12.0019405943419));
#25714=CARTESIAN_POINT('Ctrl Pts',(73.7169042772369,9.31674341779712,18.7240646086503));
#25715=CARTESIAN_POINT('Ctrl Pts',(73.8357591409808,-0.75581846594697,20.9002641569074));
#25716=CARTESIAN_POINT('Ctrl Pts',(73.9546140047244,-10.6448788649411,18.0021903481967));
#25717=CARTESIAN_POINT('Ctrl Pts',(74.0734688684682,-17.9495209615153,10.7334524098305));
#25718=CARTESIAN_POINT('Ctrl Pts',(74.1559740655264,-19.9950700033997,3.87878284554617));
#25719=CARTESIAN_POINT('Ctrl Pts',(74.1988609746701,-20.0675364883585,0.274945958911929));
#25720=CARTESIAN_POINT('Ctrl Pts',(74.2021295958992,-20.0673524071727,0.000272503390984676));
#25721=CARTESIAN_POINT('Ctrl Pts',(72.9978704041008,-20.0670305035468,0.00037895151590521));
#25722=CARTESIAN_POINT('Ctrl Pts',(73.0326058243158,-20.0645045081021,-2.9186932831106));
#25723=CARTESIAN_POINT('Ctrl Pts',(73.1069595324454,-18.6850026481514,-9.16949023623251));
#25724=CARTESIAN_POINT('Ctrl Pts',(73.2209315284896,-12.429904644976,-16.8193274183025));
#25725=CARTESIAN_POINT('Ctrl Pts',(73.3397863922333,-2.88902535394313,-20.7134216582276));
#25726=CARTESIAN_POINT('Ctrl Pts',(73.4586412559771,7.35326633413225,-19.5786051215753));
#25727=CARTESIAN_POINT('Ctrl Pts',(73.5774961197208,15.8102942970291,-13.6903943890812));
#25728=CARTESIAN_POINT('Ctrl Pts',(73.6963509834645,20.4288178986918,-4.47835947076039));
#25729=CARTESIAN_POINT('Ctrl Pts',(73.8152058472083,20.0875282846243,5.82095453526969));
#25730=CARTESIAN_POINT('Ctrl Pts',(73.934060710952,14.8692854982535,14.7070273358924));
#25731=CARTESIAN_POINT('Ctrl Pts',(74.0529155746958,6.04100129448752,20.0224525882135));
#25732=CARTESIAN_POINT('Ctrl Pts',(74.1717704384394,-4.25394819579815,20.4767240796648));
#25733=CARTESIAN_POINT('Ctrl Pts',(74.2906253021834,-13.5161023190106,15.9595514469955));
#25734=CARTESIAN_POINT('Ctrl Pts',(74.3993252907369,-18.9857656765303,8.28463624677858));
#25735=CARTESIAN_POINT('Ctrl Pts',(74.4684069913762,-20.0632263592439,2.47599137823915));
#25736=CARTESIAN_POINT('Ctrl Pts',(74.4978704041009,-20.0656858399569,-0.000513895107878137));
#25737=CARTESIAN_POINT('Origin',(65.9521295958992,0.,0.));
#25738=CARTESIAN_POINT('',(71.2021295958992,-20.0666997414326,-0.000448233882077294));
#25739=CARTESIAN_POINT('',(71.4978704041008,-20.0642475748551,-8.67278534544269E-6));
#25740=CARTESIAN_POINT('',(65.9521295958992,-20.06595,-1.45722292471193E-12));
#25741=CARTESIAN_POINT('Ctrl Pts',(71.2021295958992,-20.0666997414326,-0.000448233882078958));
#25742=CARTESIAN_POINT('Ctrl Pts',(71.2084037768056,-20.0672110152629,-0.527738819280344));
#25743=CARTESIAN_POINT('Ctrl Pts',(71.2542962456266,-19.9182399737843,-4.38431536006082));
#25744=CARTESIAN_POINT('Ctrl Pts',(71.3398070023622,-17.5314248864508,-11.4035715815495));
#25745=CARTESIAN_POINT('Ctrl Pts',(71.458661866106,-9.95752466116282,-18.3913024557491));
#25746=CARTESIAN_POINT('Ctrl Pts',(71.5775167298497,0.0339144865576418,
-20.9138985648547));
#25747=CARTESIAN_POINT('Ctrl Pts',(71.6963715935934,10.017119701265,-18.3589110863466));
#25748=CARTESIAN_POINT('Ctrl Pts',(71.8152264573371,17.5683172038997,-11.3466529868452));
#25749=CARTESIAN_POINT('Ctrl Pts',(71.9340813210809,20.8541885247641,-1.57959626350904));
#25750=CARTESIAN_POINT('Ctrl Pts',(72.0529361848246,19.0769729670116,8.57096294462323));
#25751=CARTESIAN_POINT('Ctrl Pts',(72.1717910485684,12.6681520414353,16.640619797256));
#25752=CARTESIAN_POINT('Ctrl Pts',(72.2906459123121,3.18369217161882,20.670181603907));
#25753=CARTESIAN_POINT('Ctrl Pts',(72.4095007760559,-7.07372081696884,19.6813306761887));
#25754=CARTESIAN_POINT('Ctrl Pts',(72.5283556397995,-15.6137395751919,13.9141453154726));
#25755=CARTESIAN_POINT('Ctrl Pts',(72.6258985797474,-19.5113868904301,6.40866649789178));
#25756=CARTESIAN_POINT('Ctrl Pts',(72.6838232317806,-20.0645983908398,1.53913904642774));
#25757=CARTESIAN_POINT('Ctrl Pts',(72.7021295958992,-20.0642869035746,0.000115967843645898));
#25758=CARTESIAN_POINT('Ctrl Pts',(71.4978704041008,-20.0642475748551,-8.67278534502636E-6));
#25759=CARTESIAN_POINT('Ctrl Pts',(71.5175680814263,-20.064272580664,-1.65600928132531));
#25760=CARTESIAN_POINT('Ctrl Pts',(71.5768840466664,-19.4538205919808,-6.64273518489432));
#25761=CARTESIAN_POINT('Ctrl Pts',(71.6758182998211,-15.3680940867467,-14.1849916611866));
#25762=CARTESIAN_POINT('Ctrl Pts',(71.7946731635647,-6.72855361766429,-19.8019915791725));
#25763=CARTESIAN_POINT('Ctrl Pts',(71.9135280273086,3.54457961832131,-20.6113623910834));
#25764=CARTESIAN_POINT('Ctrl Pts',(72.0323828910522,12.9571416297572,-16.416600898898));
#25765=CARTESIAN_POINT('Ctrl Pts',(72.151237754796,19.2239023220937,-8.2361328181285));
#25766=CARTESIAN_POINT('Ctrl Pts',(72.2700926185397,20.8233853839836,1.94394584218601));
#25767=CARTESIAN_POINT('Ctrl Pts',(72.3889474822834,17.3672601118087,11.6520633578796));
#25768=CARTESIAN_POINT('Ctrl Pts',(72.5078023460272,9.69462233016103,18.5312331527829));
#25769=CARTESIAN_POINT('Ctrl Pts',(72.6266572097709,-0.331725597276454,
20.9112950917769));
#25770=CARTESIAN_POINT('Ctrl Pts',(72.7455120735146,-10.2775354823501,18.2144055268431));
#25771=CARTESIAN_POINT('Ctrl Pts',(72.8643669372584,-17.7281125760169,11.0953291424513));
#25772=CARTESIAN_POINT('Ctrl Pts',(72.9484863807871,-19.9550137979455,4.15028650086484));
#25773=CARTESIAN_POINT('Ctrl Pts',(72.9929875364012,-20.0673855907025,0.410722152746902));
#25774=CARTESIAN_POINT('Ctrl Pts',(72.9978704041008,-20.0670305035468,0.00037895151590521));
#25775=CARTESIAN_POINT('Origin',(65.9521295958992,0.,0.));
#25776=CARTESIAN_POINT('',(69.7021295958992,-20.0660502412321,0.000515820514980686));
#25777=CARTESIAN_POINT('',(69.9978704041008,-20.0670795681067,-0.000365800382556847));
#25778=CARTESIAN_POINT('',(65.9521295958992,-20.06595,-1.45722292471193E-12));
#25779=CARTESIAN_POINT('Ctrl Pts',(69.7021295958992,-20.0660502412321,0.000515820514980642));
#25780=CARTESIAN_POINT('Ctrl Pts',(69.7329843218307,-20.0633906478449,-2.59279908898246));
#25781=CARTESIAN_POINT('Ctrl Pts',(69.8034573356767,-18.9097406875408,-8.51830359478506));
#25782=CARTESIAN_POINT('Ctrl Pts',(69.9135486374375,-13.2350179122529,-16.1934098084835));
#25783=CARTESIAN_POINT('Ctrl Pts',(70.032403501181,-3.89530615487391,-20.5479670028002));
#25784=CARTESIAN_POINT('Ctrl Pts',(70.1512583649248,6.39012784832653,-19.9137776962236));
#25785=CARTESIAN_POINT('Ctrl Pts',(70.2701132286686,15.124133913895,-14.4448221531172));
#25786=CARTESIAN_POINT('Ctrl Pts',(70.3889680924123,20.1862251131474,-5.46887711782098));
#25787=CARTESIAN_POINT('Ctrl Pts',(70.5078229561561,20.3474010396572,4.83482921676092));
#25788=CARTESIAN_POINT('Ctrl Pts',(70.6266778198998,15.5685305420084,13.9647112886144));
#25789=CARTESIAN_POINT('Ctrl Pts',(70.7455326836435,7.00985233357066,19.7041689177776));
#25790=CARTESIAN_POINT('Ctrl Pts',(70.8643875473874,-3.25071379005506,20.6597474264871));
#25791=CARTESIAN_POINT('Ctrl Pts',(70.9832424111308,-12.7220549410739,16.599446414106));
#25792=CARTESIAN_POINT('Ctrl Pts',(71.0958230939684,-18.7677410467943,8.9361274774765));
#25793=CARTESIAN_POINT('Ctrl Pts',(71.168785488891,-20.063982578896,2.80183527788421));
#25794=CARTESIAN_POINT('Ctrl Pts',(71.2021295958992,-20.0666997414326,-0.000448233882078958));
#25795=CARTESIAN_POINT('Ctrl Pts',(69.9978704041008,-20.0670795681067,-0.000365800382557055));
#25796=CARTESIAN_POINT('Ctrl Pts',(70.0025303385367,-20.0674098044427,-0.391971507738714));
#25797=CARTESIAN_POINT('Ctrl Pts',(70.0468085608873,-19.9607121949208,-4.11278923178899));
#25798=CARTESIAN_POINT('Ctrl Pts',(70.1307050711525,-17.7591261183169,-11.0456210793205));
#25799=CARTESIAN_POINT('Ctrl Pts',(70.2495599348961,-10.3285220474192,-18.1855419414053));
#25800=CARTESIAN_POINT('Ctrl Pts',(70.36841479864,-0.390306419466782,-20.9102837301104));
#25801=CARTESIAN_POINT('Ctrl Pts',(70.4872696623836,9.64266981062011,-18.5583195092622));
#25802=CARTESIAN_POINT('Ctrl Pts',(70.6061245261274,17.3345491904711,-11.7006712929421));
#25803=CARTESIAN_POINT('Ctrl Pts',(70.724979389871,20.8178577880174,-2.00227405925465));
#25804=CARTESIAN_POINT('Ctrl Pts',(70.843834253615,19.2469000686554,8.18224553636222));
#25805=CARTESIAN_POINT('Ctrl Pts',(70.9626891173585,13.0030812084345,16.3802375864514));
#25806=CARTESIAN_POINT('Ctrl Pts',(71.0815439811024,3.602307582272,20.6013515178363));
#25807=CARTESIAN_POINT('Ctrl Pts',(71.200398844846,-6.67305275956469,19.8207636371352));
#25808=CARTESIAN_POINT('Ctrl Pts',(71.3192537085899,-15.3282951176304,14.2279890734018));
#25809=CARTESIAN_POINT('Ctrl Pts',(71.4184108950081,-19.4443890451087,6.68023871912706));
#25810=CARTESIAN_POINT('Ctrl Pts',(71.4779497935117,-20.0642222860368,1.6747341262207));
#25811=CARTESIAN_POINT('Ctrl Pts',(71.4978704041008,-20.0642475748551,-8.67278534502636E-6));
#25812=CARTESIAN_POINT('Origin',(157.6,0.,0.));
#25813=CARTESIAN_POINT('',(150.481156847152,-16.4244471060171,0.000374833880845693));
#25814=CARTESIAN_POINT('',(150.268843152848,-16.4246125179457,0.00027738966988146));
#25815=CARTESIAN_POINT('',(157.6,-16.425,-2.01148236759953E-15));
#25816=CARTESIAN_POINT('',(150.,7.06535955977556,14.8277213114857));
#25817=CARTESIAN_POINT('Ctrl Pts',(150.481156847152,-16.4244471060171,0.000374833880845693));
#25818=CARTESIAN_POINT('Ctrl Pts',(150.469297185807,-16.4251539191907,0.816394811968673));
#25819=CARTESIAN_POINT('Ctrl Pts',(150.457437524463,-16.3653909517533,1.63231199317137));
#25820=CARTESIAN_POINT('Ctrl Pts',(150.445577863118,-16.2442674552976,2.43901578219437));
#25821=CARTESIAN_POINT('Ctrl Pts',(150.406346587624,-15.8435958745298,5.10755897833262));
#25822=CARTESIAN_POINT('Ctrl Pts',(150.367115312129,-14.7714809451613,7.67528376569759));
#25823=CARTESIAN_POINT('Ctrl Pts',(150.327884036635,-13.1555893470951,9.83643486497512));
#25824=CARTESIAN_POINT('Ctrl Pts',(150.288652761141,-11.5396977490288,11.9975859642527));
#25825=CARTESIAN_POINT('Ctrl Pts',(150.249421485646,-9.3800294822648,13.7521633754428));
#25826=CARTESIAN_POINT('Ctrl Pts',(150.210190210152,-6.93376160152484,14.891209239928));
#25827=CARTESIAN_POINT('Ctrl Pts',(150.170958934657,-4.48749372078487,16.0302551044133));
#25828=CARTESIAN_POINT('Ctrl Pts',(150.131727659163,-1.75462622606894,16.5537694221937));
#25829=CARTESIAN_POINT('Ctrl Pts',(150.092496383669,0.939415135284274,16.399456771981));
#25830=CARTESIAN_POINT('Ctrl Pts',(150.061664255779,3.05668067779249,16.2781814041431));
#25831=CARTESIAN_POINT('Ctrl Pts',(150.03083212789,5.14996527585529,15.7382465032741));
#25832=CARTESIAN_POINT('Ctrl Pts',(150.,7.06578282810915,14.8277078846934));
#25833=CARTESIAN_POINT('',(150.,-7.06535955977601,14.8277213114855));
#25834=CARTESIAN_POINT('Origin',(150.,0.,0.));
#25835=CARTESIAN_POINT('Ctrl Pts',(150.,-7.06535955977558,14.8277213114857));
#25836=CARTESIAN_POINT('Ctrl Pts',(150.039231275494,-9.50202246794195,13.6666595940101));
#25837=CARTESIAN_POINT('Ctrl Pts',(150.078462550989,-11.6458626324014,11.8940710533159));
#25838=CARTESIAN_POINT('Ctrl Pts',(150.117693826483,-13.2424554823458,9.71901539710664));
#25839=CARTESIAN_POINT('Ctrl Pts',(150.156925101978,-14.8390483322902,7.54395974089736));
#25840=CARTESIAN_POINT('Ctrl Pts',(150.196156377472,-15.8883938677195,4.96643696917295));
#25841=CARTESIAN_POINT('Ctrl Pts',(150.235387652966,-16.2653432504906,2.29434249478256));
#25842=CARTESIAN_POINT('Ctrl Pts',(150.24653948626,-16.3724944104754,1.53477626226827));
#25843=CARTESIAN_POINT('Ctrl Pts',(150.257691319554,-16.4253139196711,0.767568349022371));
#25844=CARTESIAN_POINT('Ctrl Pts',(150.268843152848,-16.4246125179457,0.00027738966988146));
#25845=CARTESIAN_POINT('Origin',(157.6,0.,0.));
#25846=CARTESIAN_POINT('',(151.981156847152,-16.4262658875693,0.000126548556290129));
#25847=CARTESIAN_POINT('',(151.768843152848,-16.4263175731226,7.92183299041088E-5));
#25848=CARTESIAN_POINT('',(157.6,-16.425,-2.01148236759953E-15));
#25849=CARTESIAN_POINT('Ctrl Pts',(151.981156847152,-16.4262658875693,0.000126548556290129));
#25850=CARTESIAN_POINT('Ctrl Pts',(151.979303767234,-16.4263192176211,0.127589430577028));
#25851=CARTESIAN_POINT('Ctrl Pts',(151.977450687317,-16.4248658227487,0.255051093337995));
#25852=CARTESIAN_POINT('Ctrl Pts',(151.9755976074,-16.4218979730467,0.38247748338803));
#25853=CARTESIAN_POINT('Ctrl Pts',(151.936366331905,-16.3590660745457,3.08020237174462));
#25854=CARTESIAN_POINT('Ctrl Pts',(151.897135056411,-15.6174481672167,5.76211785977663));
#25855=CARTESIAN_POINT('Ctrl Pts',(151.857903780916,-14.285356483579,8.10886010496594));
#25856=CARTESIAN_POINT('Ctrl Pts',(151.818672505422,-12.9532647999413,10.4556023501552));
#25857=CARTESIAN_POINT('Ctrl Pts',(151.779441229928,-11.030699339995,12.4671713525018));
#25858=CARTESIAN_POINT('Ctrl Pts',(151.740209954433,-8.74660016284646,13.9040284681142));
#25859=CARTESIAN_POINT('Ctrl Pts',(151.700978678939,-6.46250098569791,15.3408855837265));
#25860=CARTESIAN_POINT('Ctrl Pts',(151.661747403444,-3.81686809134713,16.2030308126046));
#25861=CARTESIAN_POINT('Ctrl Pts',(151.62251612795,-1.12474477240116,16.3877994644907));
#25862=CARTESIAN_POINT('Ctrl Pts',(151.583284852456,1.56737854654481,16.5725681163767));
#25863=CARTESIAN_POINT('Ctrl Pts',(151.544053576961,4.30599229008596,16.0799601912707));
#25864=CARTESIAN_POINT('Ctrl Pts',(151.504822301467,6.76498096092394,14.9686356960831));
#25865=CARTESIAN_POINT('Ctrl Pts',(151.465591025972,9.22396963176194,13.8573112008954));
#25866=CARTESIAN_POINT('Ctrl Pts',(151.426359750478,11.4033332298968,12.127270135626));
#25867=CARTESIAN_POINT('Ctrl Pts',(151.387128474984,13.0435520428528,9.9845266415244));
#25868=CARTESIAN_POINT('Ctrl Pts',(151.347897199489,14.6837708558089,7.84178314742278));
#25869=CARTESIAN_POINT('Ctrl Pts',(151.308665923995,15.7848448835862,5.28633722448888));
#25870=CARTESIAN_POINT('Ctrl Pts',(151.2694346485,16.21565768281,2.62249268910952));
#25871=CARTESIAN_POINT('Ctrl Pts',(151.230203373006,16.6464704820338,-0.0413518462698437));
#25872=CARTESIAN_POINT('Ctrl Pts',(151.190972097512,16.407022052704,-2.81359499409468));
#25873=CARTESIAN_POINT('Ctrl Pts',(151.151740822017,15.5258260253638,-5.36411671960683));
#25874=CARTESIAN_POINT('Ctrl Pts',(151.112509546523,14.6446299980235,-7.91463844511896));
#25875=CARTESIAN_POINT('Ctrl Pts',(151.073278271028,13.1216863726727,-10.2434387483184));
#25876=CARTESIAN_POINT('Ctrl Pts',(151.034046995534,11.1383480576346,-12.0732027776573));
#25877=CARTESIAN_POINT('Ctrl Pts',(150.99481572004,9.15500974259645,-13.9029668069962));
#25878=CARTESIAN_POINT('Ctrl Pts',(150.955584444545,6.71127673787098,-15.2336945624745));
#25879=CARTESIAN_POINT('Ctrl Pts',(150.916353169051,4.0981499595583,-15.9069226094236));
#25880=CARTESIAN_POINT('Ctrl Pts',(150.877121893557,1.4850231812456,-16.5801506563726));
#25881=CARTESIAN_POINT('Ctrl Pts',(150.837890618062,-1.29749737065429,-16.5958789947925));
#25882=CARTESIAN_POINT('Ctrl Pts',(150.798659342568,-3.91806767946161,-15.9522340832658));
#25883=CARTESIAN_POINT('Ctrl Pts',(150.759428067073,-6.53863798826892,-15.3085891717391));
#25884=CARTESIAN_POINT('Ctrl Pts',(150.720196791579,-8.99725805398366,-14.0055710102659));
#25885=CARTESIAN_POINT('Ctrl Pts',(150.680965516085,-11.0011543169579,-12.198344892025));
#25886=CARTESIAN_POINT('Ctrl Pts',(150.64173424059,-13.0050505799322,-10.3911187737841));
#25887=CARTESIAN_POINT('Ctrl Pts',(150.602502965096,-14.554223040166,-8.0796846987755));
#25888=CARTESIAN_POINT('Ctrl Pts',(150.563271689601,-15.4641951541993,-5.53928685881544));
#25889=CARTESIAN_POINT('Ctrl Pts',(150.535900075452,-16.0990816134985,-3.76685431395997));
#25890=CARTESIAN_POINT('Ctrl Pts',(150.508528461302,-16.4228158100718,-1.88296595721331));
#25891=CARTESIAN_POINT('Ctrl Pts',(150.481156847152,-16.4244471060171,0.000374833880845693));
#25892=CARTESIAN_POINT('Ctrl Pts',(150.268843152848,-16.4246125179457,0.00027738966988146));
#25893=CARTESIAN_POINT('Ctrl Pts',(150.296922595049,-16.422846443374,-1.93170110895333));
#25894=CARTESIAN_POINT('Ctrl Pts',(150.325002037249,-16.0817615771842,-3.86420611402143));
#25895=CARTESIAN_POINT('Ctrl Pts',(150.35308147945,-15.4143001207446,-5.67657577670535));
#25896=CARTESIAN_POINT('Ctrl Pts',(150.392312754944,-14.4817543781148,-8.20873339674647));
#25897=CARTESIAN_POINT('Ctrl Pts',(150.431544030438,-12.9121096627423,-10.5063824597724));
#25898=CARTESIAN_POINT('Ctrl Pts',(150.470775305933,-10.892224580038,-12.2957350119018));
#25899=CARTESIAN_POINT('Ctrl Pts',(150.510006581427,-8.87233949733361,-14.0850875640313));
#25900=CARTESIAN_POINT('Ctrl Pts',(150.549237856922,-6.4022140472974,-15.3661436052642));
#25901=CARTESIAN_POINT('Ctrl Pts',(150.588469132416,-3.77601912020898,-15.9864431089081));
#25902=CARTESIAN_POINT('Ctrl Pts',(150.62770040791,-1.14982419312056,-16.6067426125519));
#25903=CARTESIAN_POINT('Ctrl Pts',(150.666931683405,1.63244021102008,-16.5662855786066));
#25904=CARTESIAN_POINT('Ctrl Pts',(150.706162958899,4.23947386602044,-15.8698463806454));
#25905=CARTESIAN_POINT('Ctrl Pts',(150.745394234394,6.84650752102081,-15.1734071826843));
#25906=CARTESIAN_POINT('Ctrl Pts',(150.784625509888,9.2783104268809,-13.8209858207073));
#25907=CARTESIAN_POINT('Ctrl Pts',(150.823856785382,11.2452958317145,-11.9736504010225));
#25908=CARTESIAN_POINT('Ctrl Pts',(150.863088060877,13.212281236548,-10.1263149813378));
#25909=CARTESIAN_POINT('Ctrl Pts',(150.902319336371,14.714449140355,-7.78406550394527));
#25910=CARTESIAN_POINT('Ctrl Pts',(150.941550611866,15.572923775988,-5.22580792961083));
#25911=CARTESIAN_POINT('Ctrl Pts',(150.98078188736,16.4313984116209,-2.6675503552764));
#25912=CARTESIAN_POINT('Ctrl Pts',(151.020013162854,16.6461797790798,0.10671531599998));
#25913=CARTESIAN_POINT('Ctrl Pts',(151.059244438349,16.1916900745551,2.7666231243286));
#25914=CARTESIAN_POINT('Ctrl Pts',(151.098475713843,15.7372003700303,5.42653093265725));
#25915=CARTESIAN_POINT('Ctrl Pts',(151.137706989338,14.6134395935219,7.97208087803814));
#25916=CARTESIAN_POINT('Ctrl Pts',(151.176938264832,12.9542264882274,10.1001500394191));
#25917=CARTESIAN_POINT('Ctrl Pts',(151.216169540326,11.2950133829329,12.2282192008));
#25918=CARTESIAN_POINT('Ctrl Pts',(151.255400815821,9.10034794885215,13.9388075781811));
#25919=CARTESIAN_POINT('Ctrl Pts',(151.294632091315,6.63157168295718,15.0282162584893));
#25920=CARTESIAN_POINT('Ctrl Pts',(151.333863366809,4.1627954170622,16.1176249387976));
#25921=CARTESIAN_POINT('Ctrl Pts',(151.373094642304,1.41990831935294,16.585853922033));
#25922=CARTESIAN_POINT('Ctrl Pts',(151.412325917798,-1.27046506139402,16.3771468466143));
#25923=CARTESIAN_POINT('Ctrl Pts',(151.451557193293,-3.96083844214098,16.1684397711956));
#25924=CARTESIAN_POINT('Ctrl Pts',(151.490788468787,-6.59869810592565,15.2827966371228));
#25925=CARTESIAN_POINT('Ctrl Pts',(151.530019744281,-8.86992648726269,13.8256799900127));
#25926=CARTESIAN_POINT('Ctrl Pts',(151.569251019776,-11.1411548685997,12.3685633429027));
#25927=CARTESIAN_POINT('Ctrl Pts',(151.60848229527,-13.0457519674892,10.3399731827554));
#25928=CARTESIAN_POINT('Ctrl Pts',(151.647713570765,-14.3569173638976,7.98147518136614));
#25929=CARTESIAN_POINT('Ctrl Pts',(151.686944846259,-15.6680827603059,5.62297717997691));
#25930=CARTESIAN_POINT('Ctrl Pts',(151.726176121753,-16.3858164542333,2.93457133734574));
#25931=CARTESIAN_POINT('Ctrl Pts',(151.765407397248,-16.4246503779292,0.236394302476631));
#25932=CARTESIAN_POINT('Ctrl Pts',(151.766552649115,-16.4257840301759,0.157628260661814));
#25933=CARTESIAN_POINT('Ctrl Pts',(151.767697900981,-16.4263391298596,0.078853891920753));
#25934=CARTESIAN_POINT('Ctrl Pts',(151.768843152848,-16.4263175731226,7.92183299041088E-5));
#25935=CARTESIAN_POINT('Origin',(157.6,0.,0.));
#25936=CARTESIAN_POINT('',(153.481156847152,-16.4251954303659,-0.000393763598601771));
#25937=CARTESIAN_POINT('',(153.268843152848,-16.4250464537185,-0.000400491521010713));
#25938=CARTESIAN_POINT('',(157.6,-16.425,-2.01148236759953E-15));
#25939=CARTESIAN_POINT('Ctrl Pts',(153.481156847152,-16.4251954303659,-0.000393763598601771));
#25940=CARTESIAN_POINT('Ctrl Pts',(153.450079073167,-16.4230658025619,2.13767372058375));
#25941=CARTESIAN_POINT('Ctrl Pts',(153.419001299182,-16.0032991920971,4.27655312283435));
#25942=CARTESIAN_POINT('Ctrl Pts',(153.387923525198,-15.1895390617785,6.25323317595138));
#25943=CARTESIAN_POINT('Ctrl Pts',(153.348692249703,-14.1622824804465,8.74851098337746));
#25944=CARTESIAN_POINT('Ctrl Pts',(153.309460974209,-12.5071784595547,10.9853164025025));
#25945=CARTESIAN_POINT('Ctrl Pts',(153.270229698715,-10.4213176161215,12.6972895220213));
#25946=CARTESIAN_POINT('Ctrl Pts',(153.23099842322,-8.33545677268826,14.4092626415401));
#25947=CARTESIAN_POINT('Ctrl Pts',(153.191767147726,-5.81883910671363,15.5964034614527));
#25948=CARTESIAN_POINT('Ctrl Pts',(153.152535872231,-3.17114471221293,16.1173466574469));
#25949=CARTESIAN_POINT('Ctrl Pts',(153.113304596737,-0.523450317712208,
16.6382898534412));
#25950=CARTESIAN_POINT('Ctrl Pts',(153.074073321243,2.25532080531457,16.4930354255172));
#25951=CARTESIAN_POINT('Ctrl Pts',(153.034842045748,4.83427119768834,15.6988803438118));
#25952=CARTESIAN_POINT('Ctrl Pts',(152.995610770254,7.41322159006212,14.9047252621064));
#25953=CARTESIAN_POINT('Ctrl Pts',(152.95637949476,9.79235125178288,13.4616695266198));
#25954=CARTESIAN_POINT('Ctrl Pts',(152.917148219265,11.6883522293468,11.5415529381808));
#25955=CARTESIAN_POINT('Ctrl Pts',(152.877916943771,13.5843532069107,9.6214363497418));
#25956=CARTESIAN_POINT('Ctrl Pts',(152.838685668276,14.9972255003178,7.22425890835048));
#25957=CARTESIAN_POINT('Ctrl Pts',(152.799454392782,15.7587235681631,4.63547770616391));
#25958=CARTESIAN_POINT('Ctrl Pts',(152.760223117288,16.5202216360085,2.04669650397737));
#25959=CARTESIAN_POINT('Ctrl Pts',(152.720991841793,16.6303454782922,-0.733688459004435));
#25960=CARTESIAN_POINT('Ctrl Pts',(152.681760566299,16.075981492637,-3.374587546725));
#25961=CARTESIAN_POINT('Ctrl Pts',(152.642529290804,15.5216175069818,-6.01548663444557));
#25962=CARTESIAN_POINT('Ctrl Pts',(152.60329801531,14.3027656933877,-8.51689984690491));
#25963=CARTESIAN_POINT('Ctrl Pts',(152.564066739816,12.5645675371996,-10.5809576440515));
#25964=CARTESIAN_POINT('Ctrl Pts',(152.524835464321,10.8263693810116,-12.645015441198));
#25965=CARTESIAN_POINT('Ctrl Pts',(152.485604188827,8.56882488222956,-14.2717178230318));
#25966=CARTESIAN_POINT('Ctrl Pts',(152.446372913332,6.06076357217012,-15.2673562539341));
#25967=CARTESIAN_POINT('Ctrl Pts',(152.407141637838,3.55270226211068,-16.2629946848364));
#25968=CARTESIAN_POINT('Ctrl Pts',(152.367910362344,0.794124140773821,-16.6275691648073));
#25969=CARTESIAN_POINT('Ctrl Pts',(152.328679086849,-1.8864779254381,-16.3176659819518));
#25970=CARTESIAN_POINT('Ctrl Pts',(152.289447811355,-4.56707999165003,-16.0077627990964));
#25971=CARTESIAN_POINT('Ctrl Pts',(152.25021653586,-7.16970600273701,-15.0233819534147));
#25972=CARTESIAN_POINT('Ctrl Pts',(152.210985260366,-9.3844339477921,-13.4817440096735));
#25973=CARTESIAN_POINT('Ctrl Pts',(152.171753984872,-11.5991618928472,-11.9401060659323));
#25974=CARTESIAN_POINT('Ctrl Pts',(152.132522709377,-13.4259917718704,-9.84121102413149));
#25975=CARTESIAN_POINT('Ctrl Pts',(152.093291433883,-14.6473837665455,-7.43499635889051));
#25976=CARTESIAN_POINT('Ctrl Pts',(152.055913238306,-15.8110836023985,-5.1424386680136));
#25977=CARTESIAN_POINT('Ctrl Pts',(152.018535042729,-16.4251901751372,-2.5709080237884));
#25978=CARTESIAN_POINT('Ctrl Pts',(151.981156847152,-16.4262658875693,0.000126548556290129));
#25979=CARTESIAN_POINT('Ctrl Pts',(151.768843152848,-16.4263175731226,7.92183299041088E-5));
#25980=CARTESIAN_POINT('Ctrl Pts',(151.806929176476,-16.4256006911727,-2.61961882950725));
#25981=CARTESIAN_POINT('Ctrl Pts',(151.845015200103,-15.7871398110322,-5.23965402112013));
#25982=CARTESIAN_POINT('Ctrl Pts',(151.883101223731,-14.5806721903752,-7.56498651285041));
#25983=CARTESIAN_POINT('Ctrl Pts',(151.922332499225,-13.3379259256609,-9.9602420662013));
#25984=CARTESIAN_POINT('Ctrl Pts',(151.96156377472,-11.4924992427678,-12.042804945796));
#25985=CARTESIAN_POINT('Ctrl Pts',(152.000795050214,-9.26414648165388,-13.5646825352884));
#25986=CARTESIAN_POINT('Ctrl Pts',(152.040026325709,-7.03579372053995,-15.0865601247808));
#25987=CARTESIAN_POINT('Ctrl Pts',(152.079257601203,-4.42451488120518,-16.0477524241709));
#25988=CARTESIAN_POINT('Ctrl Pts',(152.118488876697,-1.74126235529177,-16.3338001645162));
#25989=CARTESIAN_POINT('Ctrl Pts',(152.157720152192,0.941990170621638,-16.6198479048615));
#25990=CARTESIAN_POINT('Ctrl Pts',(152.196951427686,3.69721638311369,-16.230751086162));
#25991=CARTESIAN_POINT('Ctrl Pts',(152.236182703181,6.19632256160219,-15.2128435565597));
#25992=CARTESIAN_POINT('Ctrl Pts',(152.275413978675,8.69542874009068,-14.1949360269574));
#25993=CARTESIAN_POINT('Ctrl Pts',(152.314645254169,10.9384148845756,-12.5482177864524));
#25994=CARTESIAN_POINT('Ctrl Pts',(152.353876529664,12.6581850804413,-10.4687808672768));
#25995=CARTESIAN_POINT('Ctrl Pts',(152.393107805158,14.377955276307,-8.38934394810116));
#25996=CARTESIAN_POINT('Ctrl Pts',(152.432339080653,15.5745095235535,-5.87718835025486));
#25997=CARTESIAN_POINT('Ctrl Pts',(152.471570356147,16.1053615419439,-3.23146282334491));
#25998=CARTESIAN_POINT('Ctrl Pts',(152.510801631641,16.6362135603342,-0.585737296434967));
#25999=CARTESIAN_POINT('Ctrl Pts',(152.550032907136,16.5013633498685,2.19355815953864));
#26000=CARTESIAN_POINT('Ctrl Pts',(152.58926418263,15.7168689413851,4.77546364800653));
#26001=CARTESIAN_POINT('Ctrl Pts',(152.628495458125,14.9323745329016,7.35736913647443));
#26002=CARTESIAN_POINT('Ctrl Pts',(152.667726733619,13.4982359264005,9.74188465743662));
#26003=CARTESIAN_POINT('Ctrl Pts',(152.706958009113,11.5852310664511,11.6450609063546));
#26004=CARTESIAN_POINT('Ctrl Pts',(152.746189284608,9.67222620650168,13.5482371552725));
#26005=CARTESIAN_POINT('Ctrl Pts',(152.785420560102,7.28035509310412,14.9700741321463));
#26006=CARTESIAN_POINT('Ctrl Pts',(152.824651835597,4.69444293825117,15.7412587766719));
#26007=CARTESIAN_POINT('Ctrl Pts',(152.863883111091,2.10853078339819,16.5124434211975));
#26008=CARTESIAN_POINT('Ctrl Pts',(152.903114386585,-0.671422412910195,
16.632975733375));
#26009=CARTESIAN_POINT('Ctrl Pts',(152.94234566208,-3.31437842963123,16.0885026649596));
#26010=CARTESIAN_POINT('Ctrl Pts',(152.981576937574,-5.95733444635227,15.5440295965442));
#26011=CARTESIAN_POINT('Ctrl Pts',(153.020808213068,-8.46329328348596,14.3345511475358));
#26012=CARTESIAN_POINT('Ctrl Pts',(153.060039488563,-10.5338441056942,12.6040926183492));
#26013=CARTESIAN_POINT('Ctrl Pts',(153.099270764057,-12.6043949279025,10.8736340891626));
#26014=CARTESIAN_POINT('Ctrl Pts',(153.138502039552,-14.2395377351854,8.62219547979772));
#26015=CARTESIAN_POINT('Ctrl Pts',(153.177733315046,-15.2445589018574,6.11787922918138));
#26016=CARTESIAN_POINT('Ctrl Pts',(153.20810326098,-16.0225718038015,4.17922319074239));
#26017=CARTESIAN_POINT('Ctrl Pts',(153.238473206914,-16.4229711502018,2.08902494350394));
#26018=CARTESIAN_POINT('Ctrl Pts',(153.268843152848,-16.4250464537185,-0.000400491521010713));
#26019=CARTESIAN_POINT('Origin',(157.6,0.,0.));
#26020=CARTESIAN_POINT('',(154.981156847152,-16.4236977086378,-8.83777446403222E-5));
#26021=CARTESIAN_POINT('',(154.768843152848,-16.4236758302589,-4.56654442711846E-5));
#26022=CARTESIAN_POINT('',(157.6,-16.425,-2.01148236759953E-15));
#26023=CARTESIAN_POINT('Ctrl Pts',(154.981156847152,-16.4236977086378,-8.83777446403222E-5));
#26024=CARTESIAN_POINT('Ctrl Pts',(154.960085654594,-16.4234191421019,1.44993295162065));
#26025=CARTESIAN_POINT('Ctrl Pts',(154.939014462037,-16.233159747019,2.90002600296101));
#26026=CARTESIAN_POINT('Ctrl Pts',(154.917943269479,-15.8538585334443,4.29885934448325));
#26027=CARTESIAN_POINT('Ctrl Pts',(154.878711993985,-15.1476588077049,6.90326894504319));
#26028=CARTESIAN_POINT('Ctrl Pts',(154.839480718491,-13.7861525287593,9.32998863536398));
#26029=CARTESIAN_POINT('Ctrl Pts',(154.800249442996,-11.9314685472444,11.2900434174645));
#26030=CARTESIAN_POINT('Ctrl Pts',(154.761018167502,-10.0767845657294,13.250098199565));
#26031=CARTESIAN_POINT('Ctrl Pts',(154.721786892007,-7.72892288164514,14.7434880734452));
#26032=CARTESIAN_POINT('Ctrl Pts',(154.682555616513,-5.16746804203438,15.5923794238297));
#26033=CARTESIAN_POINT('Ctrl Pts',(154.643324341019,-2.60601320242361,16.4412707742142));
#26034=CARTESIAN_POINT('Ctrl Pts',(154.604093065524,0.169034792713642,16.6456636011031));
#26035=CARTESIAN_POINT('Ctrl Pts',(154.56486179003,2.82722183613503,16.1812187041457));
#26036=CARTESIAN_POINT('Ctrl Pts',(154.525630514535,5.48540887955642,15.7167738071883));
#26037=CARTESIAN_POINT('Ctrl Pts',(154.486399239041,8.02673497126193,14.5834911863846));
#26038=CARTESIAN_POINT('Ctrl Pts',(154.447167963547,10.1485777255062,12.9163227046816));
#26039=CARTESIAN_POINT('Ctrl Pts',(154.407936688052,12.2704204797506,11.2491542229785));
#26040=CARTESIAN_POINT('Ctrl Pts',(154.368705412558,13.9727798965336,9.04809988037614));
#26041=CARTESIAN_POINT('Ctrl Pts',(154.329474137063,15.0529381625909,6.5752623320541));
#26042=CARTESIAN_POINT('Ctrl Pts',(154.290242861569,16.1330964286481,4.10242478373211));
#26043=CARTESIAN_POINT('Ctrl Pts',(154.251011586075,16.5910535439795,1.35780402969045));
#26044=CARTESIAN_POINT('Ctrl Pts',(154.21178031058,16.3722757455772,-1.33176911396061));
#26045=CARTESIAN_POINT('Ctrl Pts',(154.172549035086,16.1534979471749,-4.02134225761174));
#26046=CARTESIAN_POINT('Ctrl Pts',(154.133317759591,15.2579852350389,-6.65586779087229));
#26047=CARTESIAN_POINT('Ctrl Pts',(154.094086484097,13.7923757121252,-8.92162509174716));
#26048=CARTESIAN_POINT('Ctrl Pts',(154.054855208603,12.3267661892115,-11.187382392622));
#26049=CARTESIAN_POINT('Ctrl Pts',(154.015623933108,10.2910598555201,-13.0843714611112));
#26050=CARTESIAN_POINT('Ctrl Pts',(153.976392657614,7.92766964238983,-14.3866978873974));
#26051=CARTESIAN_POINT('Ctrl Pts',(153.937161382119,5.56427942925962,-15.6890243136836));
#26052=CARTESIAN_POINT('Ctrl Pts',(153.897930106625,2.87320533669065,-16.3966880977669));
#26053=CARTESIAN_POINT('Ctrl Pts',(153.858698831131,0.174901817485615,-16.42542028127));
#26054=CARTESIAN_POINT('Ctrl Pts',(153.819467555636,-2.52340170171938,-16.454152464773));
#26055=CARTESIAN_POINT('Ctrl Pts',(153.780236280142,-5.22893464756042,-15.803953047696));
#26056=CARTESIAN_POINT('Ctrl Pts',(153.741005004647,-7.61952079973456,-14.5522481027684));
#26057=CARTESIAN_POINT('Ctrl Pts',(153.701773729153,-10.0101069519087,-13.3005431578408));
#26058=CARTESIAN_POINT('Ctrl Pts',(153.662542453659,-12.0857463104159,-11.4473326850627));
#26059=CARTESIAN_POINT('Ctrl Pts',(153.623311178164,-13.5992706992915,-9.21329791711442));
#26060=CARTESIAN_POINT('Ctrl Pts',(153.58407990267,-15.1127950881672,-6.97926314916609));
#26061=CARTESIAN_POINT('Ctrl Pts',(153.544848627175,-16.0642045074111,-4.36440408604759));
#26062=CARTESIAN_POINT('Ctrl Pts',(153.505617351681,-16.340204646147,-1.68009945662473));
#26063=CARTESIAN_POINT('Ctrl Pts',(153.497463850171,-16.3975662159535,-1.12221594218909));
#26064=CARTESIAN_POINT('Ctrl Pts',(153.489310348662,-16.4257541551807,-0.561332795744825));
#26065=CARTESIAN_POINT('Ctrl Pts',(153.481156847152,-16.4251954303659,-0.000393763598601771));
#26066=CARTESIAN_POINT('Ctrl Pts',(153.268843152848,-16.4250464537185,-0.000400491521010713));
#26067=CARTESIAN_POINT('Ctrl Pts',(153.277704482409,-16.4256519848721,-0.610052132384859));
#26068=CARTESIAN_POINT('Ctrl Pts',(153.286565811969,-16.3923460737495,-1.21963797963861));
#26069=CARTESIAN_POINT('Ctrl Pts',(153.295427141529,-16.324614256424,-1.8253744147469));
#26070=CARTESIAN_POINT('Ctrl Pts',(153.334658417024,-16.0247489182573,-4.50711791619102));
#26071=CARTESIAN_POINT('Ctrl Pts',(153.373889692518,-15.0501187158627,-7.11341102721143));
#26072=CARTESIAN_POINT('Ctrl Pts',(153.413120968012,-13.5167831026228,-9.3338950568178));
#26073=CARTESIAN_POINT('Ctrl Pts',(153.452352243507,-11.9834474893829,-11.5543790864242));
#26074=CARTESIAN_POINT('Ctrl Pts',(153.491583519001,-9.89140646529765,-13.3890540346165));
#26075=CARTESIAN_POINT('Ctrl Pts',(153.530814794496,-7.48978132489561,-14.6194458882782));
#26076=CARTESIAN_POINT('Ctrl Pts',(153.57004606999,-5.08815618449357,-15.84983774194));
#26077=CARTESIAN_POINT('Ctrl Pts',(153.609277345484,-2.37694692777465,-16.4759465010711));
#26078=CARTESIAN_POINT('Ctrl Pts',(153.648508620979,0.32099428701121,-16.4232148205748));
#26079=CARTESIAN_POINT('Ctrl Pts',(153.687739896473,3.01893550179707,-16.3704831400786));
#26080=CARTESIAN_POINT('Ctrl Pts',(153.726971171968,5.70360867464991,-15.6389110199551));
#26081=CARTESIAN_POINT('Ctrl Pts',(153.766202447462,8.05532157749775,-14.3156144352293));
#26082=CARTESIAN_POINT('Ctrl Pts',(153.805433722957,10.4070344803456,-12.9923178505035));
#26083=CARTESIAN_POINT('Ctrl Pts',(153.844664998451,12.4257871131884,-11.0772968011756));
#26084=CARTESIAN_POINT('Ctrl Pts',(153.883896273945,13.8711853998883,-8.79859295438607));
#26085=CARTESIAN_POINT('Ctrl Pts',(153.92312754944,15.3165836865881,-6.51988910759658));
#26086=CARTESIAN_POINT('Ctrl Pts',(153.962358824934,16.188627627145,-3.87750246334555));
#26087=CARTESIAN_POINT('Ctrl Pts',(154.001590100428,16.3834737916948,-1.18608974866797));
#26088=CARTESIAN_POINT('Ctrl Pts',(154.040821375923,16.5783199562446,1.50532296600961));
#26089=CARTESIAN_POINT('Ctrl Pts',(154.080052651417,16.0959683447872,4.24576175111375));
#26090=CARTESIAN_POINT('Ctrl Pts',(154.119283926912,14.9938576291657,6.70889378149298));
#26091=CARTESIAN_POINT('Ctrl Pts',(154.158515202406,13.8917469135441,9.17202581187224));
#26092=CARTESIAN_POINT('Ctrl Pts',(154.1977464779,12.1698770937584,11.3578510875266));
#26093=CARTESIAN_POINT('Ctrl Pts',(154.236977753395,10.0332892916491,13.0060804382075));
#26094=CARTESIAN_POINT('Ctrl Pts',(154.276209028889,7.89670148953989,14.6543097888884));
#26095=CARTESIAN_POINT('Ctrl Pts',(154.315440304384,5.34539570510719,15.764943214596));
#26096=CARTESIAN_POINT('Ctrl Pts',(154.354671579878,2.6831827109122,16.2057259298961));
#26097=CARTESIAN_POINT('Ctrl Pts',(154.393902855372,0.0209697167172235,
16.6465086451963));
#26098=CARTESIAN_POINT('Ctrl Pts',(154.433134130867,-2.75215048724,16.4174406500891));
#26099=CARTESIAN_POINT('Ctrl Pts',(154.472365406361,-5.30595335605791,15.5457994763339));
#26100=CARTESIAN_POINT('Ctrl Pts',(154.511596681856,-7.85975622487584,14.6741583025787));
#26101=CARTESIAN_POINT('Ctrl Pts',(154.55082795735,-10.1942417585544,13.1599439501754));
#26102=CARTESIAN_POINT('Ctrl Pts',(154.590059232844,-12.0314182487506,11.1834698237477));
#26103=CARTESIAN_POINT('Ctrl Pts',(154.629290508339,-13.8685947389469,9.20699569731996));
#26104=CARTESIAN_POINT('Ctrl Pts',(154.668521783833,-15.2084621856608,6.76826179686773));
#26105=CARTESIAN_POINT('Ctrl Pts',(154.707753059328,-15.8914685012518,4.15767377854104));
#26106=CARTESIAN_POINT('Ctrl Pts',(154.728116423834,-16.2459893877024,2.80262338253725));
#26107=CARTESIAN_POINT('Ctrl Pts',(154.748479788341,-16.4235369624548,1.40127158289091));
#26108=CARTESIAN_POINT('Ctrl Pts',(154.768843152848,-16.4236758302589,-4.56654442711846E-5));
#26109=CARTESIAN_POINT('Origin',(157.6,0.,0.));
#26110=CARTESIAN_POINT('',(156.481156847152,-16.4245975118847,0.000389008950720526));
#26111=CARTESIAN_POINT('',(156.268843152848,-16.4247375848135,0.000397937037689734));
#26112=CARTESIAN_POINT('',(157.6,-16.425,-2.01148236759953E-15));
#26113=CARTESIAN_POINT('Ctrl Pts',(156.481156847152,-16.4245975118847,0.000389008950720526));
#26114=CARTESIAN_POINT('Ctrl Pts',(156.470092236022,-16.4252950978913,0.761684348249804));
#26115=CARTESIAN_POINT('Ctrl Pts',(156.459027624891,-16.3733031429826,1.52288516962114));
#26116=CARTESIAN_POINT('Ctrl Pts',(156.447963013761,-16.2678244069857,2.27660078309594));
#26117=CARTESIAN_POINT('Ctrl Pts',(156.408731738266,-15.893833373596,4.94901507116341));
#26118=CARTESIAN_POINT('Ctrl Pts',(156.369500462772,-14.8474248389515,7.52732788803067));
#26119=CARTESIAN_POINT('Ctrl Pts',(156.330269187278,-13.2532056562426,9.70451245016734));
#26120=CARTESIAN_POINT('Ctrl Pts',(156.291037911783,-11.6589864735338,11.881697012304));
#26121=CARTESIAN_POINT('Ctrl Pts',(156.251806636289,-9.51695664276062,13.6577533197101));
#26122=CARTESIAN_POINT('Ctrl Pts',(156.212575360794,-7.08219015062719,14.8211876964187));
#26123=CARTESIAN_POINT('Ctrl Pts',(156.1733440853,-4.64742365849377,15.9846220731273));
#26124=CARTESIAN_POINT('Ctrl Pts',(156.134112809806,-1.91992050500006,16.5354345191385));
#26125=CARTESIAN_POINT('Ctrl Pts',(156.094881534311,0.775526866203273,16.4080340120903));
#26126=CARTESIAN_POINT('Ctrl Pts',(156.055650258817,3.4709742374066,16.280633505042));
#26127=CARTESIAN_POINT('Ctrl Pts',(156.016418983322,6.13436582631956,15.4750200449344));
#26128=CARTESIAN_POINT('Ctrl Pts',(155.977187707828,8.44854362656052,14.0871264866976));
#26129=CARTESIAN_POINT('Ctrl Pts',(155.937956432334,10.7627214268014,12.6992329284609));
#26130=CARTESIAN_POINT('Ctrl Pts',(155.898725156839,12.7276854383704,10.7290592720952));
#26131=CARTESIAN_POINT('Ctrl Pts',(155.859493881345,14.1094467611315,8.41121478485182));
#26132=CARTESIAN_POINT('Ctrl Pts',(155.82026260585,15.4912080838927,6.09337029760841));
#26133=CARTESIAN_POINT('Ctrl Pts',(155.781031330356,16.2897667178459,3.42785497948738));
#26134=CARTESIAN_POINT('Ctrl Pts',(155.741800054862,16.4100299002982,0.73207973160974));
#26135=CARTESIAN_POINT('Ctrl Pts',(155.702568779367,16.5302930827504,-1.96369551626784));
#26136=CARTESIAN_POINT('Ctrl Pts',(155.663337503873,15.9722608137017,-4.689730693902));
#26137=CARTESIAN_POINT('Ctrl Pts',(155.624106228379,14.8023838556628,-7.12140816494386));
#26138=CARTESIAN_POINT('Ctrl Pts',(155.584874952884,13.6325068976238,-9.5530856359857));
#26139=CARTESIAN_POINT('Ctrl Pts',(155.54564367739,11.8507852505947,-11.6904054004352));
#26140=CARTESIAN_POINT('Ctrl Pts',(155.506412401895,9.66938722202629,-13.2788543486488));
#26141=CARTESIAN_POINT('Ctrl Pts',(155.467181126401,7.48798919345788,-14.8673032968624));
#26142=CARTESIAN_POINT('Ctrl Pts',(155.427949850907,4.90691478335018,-15.9068814288401));
#26143=CARTESIAN_POINT('Ctrl Pts',(155.388718575412,2.23351962714189,-16.273795259167));
#26144=CARTESIAN_POINT('Ctrl Pts',(155.349487299918,-0.439875529066391,
-16.6407090894939));
#26145=CARTESIAN_POINT('Ctrl Pts',(155.310256024423,-3.20559143137527,-16.3349586181701));
#26146=CARTESIAN_POINT('Ctrl Pts',(155.271024748929,-5.73428524283742,-15.3929527646872));
#26147=CARTESIAN_POINT('Ctrl Pts',(155.231793473434,-8.26297905429957,-14.4509469112043));
#26148=CARTESIAN_POINT('Ctrl Pts',(155.19256219794,-10.554650774915,-12.8726856755622));
#26149=CARTESIAN_POINT('Ctrl Pts',(155.153330922446,-12.336406986676,-10.8461091973669));
#26150=CARTESIAN_POINT('Ctrl Pts',(155.114099646951,-14.1181631984369,-8.81953271917163));
#26151=CARTESIAN_POINT('Ctrl Pts',(155.074868371457,-15.3900039013434,-6.34464099842317));
#26152=CARTESIAN_POINT('Ctrl Pts',(155.035637095963,-16.0004776665301,-3.71614538264941));
#26153=CARTESIAN_POINT('Ctrl Pts',(155.017477013026,-16.2830648133123,-2.49941975290202));
#26154=CARTESIAN_POINT('Ctrl Pts',(154.999316930089,-16.4239377895627,-1.24978070197727));
#26155=CARTESIAN_POINT('Ctrl Pts',(154.981156847152,-16.4236977086378,-8.83777446403222E-5));
#26156=CARTESIAN_POINT('Ctrl Pts',(154.768843152848,-16.4236758302589,-4.56654442711846E-5));
#26157=CARTESIAN_POINT('Ctrl Pts',(154.787711063836,-16.4238044998294,-1.29845237510138));
#26158=CARTESIAN_POINT('Ctrl Pts',(154.806578974823,-16.2716248951007,-2.59682942189317));
#26159=CARTESIAN_POINT('Ctrl Pts',(154.825446885811,-15.966790672975,-3.85831802479324));
#26160=CARTESIAN_POINT('Ctrl Pts',(154.864678161305,-15.3329613446391,-6.48127967359964));
#26161=CARTESIAN_POINT('Ctrl Pts',(154.903909436799,-14.0391575034993,-8.9447608350113));
#26162=CARTESIAN_POINT('Ctrl Pts',(154.943140712294,-12.2394459599386,-10.9554089366298));
#26163=CARTESIAN_POINT('Ctrl Pts',(154.982371987788,-10.4397344163778,-12.9660570382483));
#26164=CARTESIAN_POINT('Ctrl Pts',(155.021603263283,-8.13411517039618,-14.5238720800737));
#26165=CARTESIAN_POINT('Ctrl Pts',(155.060834538777,-5.59714251831809,-15.4433486655156));
#26166=CARTESIAN_POINT('Ctrl Pts',(155.100065814272,-3.06016986623997,-16.3628252509574));
#26167=CARTESIAN_POINT('Ctrl Pts',(155.139297089766,-0.291843808065398,
-16.6439633800158));
#26168=CARTESIAN_POINT('Ctrl Pts',(155.17852836526,2.37818200058848,-16.2532849832618));
#26169=CARTESIAN_POINT('Ctrl Pts',(155.217759640755,5.04820780924235,-15.8626065865077));
#26170=CARTESIAN_POINT('Ctrl Pts',(155.256990916249,7.61993336837555,-14.8001116639413));
#26171=CARTESIAN_POINT('Ctrl Pts',(155.296222191744,9.78711630841292,-13.1923226438957));
#26172=CARTESIAN_POINT('Ctrl Pts',(155.335453467238,11.9542992484503,-11.5845336238501));
#26173=CARTESIAN_POINT('Ctrl Pts',(155.374684742732,13.7169395693918,-9.43145050632542));
#26174=CARTESIAN_POINT('Ctrl Pts',(155.413916018227,14.8651411776684,-6.98946350895643));
#26175=CARTESIAN_POINT('Ctrl Pts',(155.453147293721,16.0133427859449,-4.54747651158745));
#26176=CARTESIAN_POINT('Ctrl Pts',(155.492378569216,16.5471056815565,-1.81658563437417));
#26177=CARTESIAN_POINT('Ctrl Pts',(155.53160984471,16.4028691111549,0.878013267192959));
#26178=CARTESIAN_POINT('Ctrl Pts',(155.570841120204,16.2586325407533,3.57261216876009));
#26179=CARTESIAN_POINT('Ctrl Pts',(155.610072395699,15.4363965043385,6.23091909468103));
#26180=CARTESIAN_POINT('Ctrl Pts',(155.649303671193,14.0340732815655,8.53638152279379));
#26181=CARTESIAN_POINT('Ctrl Pts',(155.688534946687,12.6317500587925,10.8418439509066));
#26182=CARTESIAN_POINT('Ctrl Pts',(155.727766222182,10.6493396496614,12.7944618812111));
#26183=CARTESIAN_POINT('Ctrl Pts',(155.766997497676,8.32290848008079,14.1617165911215));
#26184=CARTESIAN_POINT('Ctrl Pts',(155.806228773171,5.99647731050022,15.5289713010318));
#26185=CARTESIAN_POINT('Ctrl Pts',(155.845460048665,3.32602538047026,16.3108627905479));
#26186=CARTESIAN_POINT('Ctrl Pts',(155.884691324159,0.629551445334231,16.4142830288966));
#26187=CARTESIAN_POINT('Ctrl Pts',(155.923922599654,-2.0669224898018,16.5177032672453));
#26188=CARTESIAN_POINT('Ctrl Pts',(155.963153875148,-4.78941843004388,15.9426522544265));
#26189=CARTESIAN_POINT('Ctrl Pts',(156.002385150643,-7.21374019320702,14.7576073534959));
#26190=CARTESIAN_POINT('Ctrl Pts',(156.041616426137,-9.63806195637014,13.5725624525653));
#26191=CARTESIAN_POINT('Ctrl Pts',(156.080847701631,-11.7642095424543,11.7775236635228));
#26192=CARTESIAN_POINT('Ctrl Pts',(156.120078977126,-13.3390002304198,9.5862451057704));
#26193=CARTESIAN_POINT('Ctrl Pts',(156.15931025262,-14.9137909183852,7.39496654801799));
#26194=CARTESIAN_POINT('Ctrl Pts',(156.198541528115,-15.9372247082318,4.80744822155563));
#26195=CARTESIAN_POINT('Ctrl Pts',(156.237772803609,-16.287430590904,2.13181310661377));
#26196=CARTESIAN_POINT('Ctrl Pts',(156.248129586689,-16.3798825011303,1.42546409968821));
#26197=CARTESIAN_POINT('Ctrl Pts',(156.258486369768,-16.425415598584,0.712974029600022));
#26198=CARTESIAN_POINT('Ctrl Pts',(156.268843152848,-16.4247375848135,0.000397937037689734));
#26199=CARTESIAN_POINT('Origin',(157.6,0.,0.));
#26200=CARTESIAN_POINT('',(157.981156847152,-16.4263224034013,7.32633077222405E-5));
#26201=CARTESIAN_POINT('',(157.768843152848,-16.4263481654919,2.43998567653511E-5));
#26202=CARTESIAN_POINT('',(157.6,-16.425,-2.01148236759953E-15));
#26203=CARTESIAN_POINT('Ctrl Pts',(157.981156847152,-16.4263224034013,7.32633077222405E-5));
#26204=CARTESIAN_POINT('Ctrl Pts',(157.980098817449,-16.4263409280204,0.0728484104607535));
#26205=CARTESIAN_POINT('Ctrl Pts',(157.979040787745,-16.4258671636985,0.145623315585142));
#26206=CARTESIAN_POINT('Ctrl Pts',(157.977982758042,-16.4248996084331,0.218391655079058));
#26207=CARTESIAN_POINT('Ctrl Pts',(157.938751482548,-16.389023085253,2.91660964019587));
#26208=CARTESIAN_POINT('Ctrl Pts',(157.899520207053,-15.6742364830876,5.60580058104853));
#26209=CARTESIAN_POINT('Ctrl Pts',(157.860288931559,-14.3656569490643,7.96573427148533));
#26210=CARTESIAN_POINT('Ctrl Pts',(157.821057656065,-13.057077415041,10.3256679619221));
#26211=CARTESIAN_POINT('Ctrl Pts',(157.78182638057,-11.1547049491598,12.356344401943));
#26212=CARTESIAN_POINT('Ctrl Pts',(157.742595105076,-8.88507501889968,13.8159496224704));
#26213=CARTESIAN_POINT('Ctrl Pts',(157.703363829582,-6.61544508863964,15.2755548429977));
#26214=CARTESIAN_POINT('Ctrl Pts',(157.664132554087,-3.97855769400073,16.1640888440315));
#26215=CARTESIAN_POINT('Ctrl Pts',(157.624901278593,-1.28841470861576,16.3757445510345));
#26216=CARTESIAN_POINT('Ctrl Pts',(157.585670003098,1.40172827676925,16.5874002580375));
#26217=CARTESIAN_POINT('Ctrl Pts',(157.546438727604,4.14512685290032,16.1221776710096));
#26218=CARTESIAN_POINT('Ctrl Pts',(157.50720745211,6.61509574122592,15.0354757289728));
#26219=CARTESIAN_POINT('Ctrl Pts',(157.467976176615,9.08506462955151,13.9487737869359));
#26220=CARTESIAN_POINT('Ctrl Pts',(157.428744901121,11.2816038300716,12.24059248989));
#26221=CARTESIAN_POINT('Ctrl Pts',(157.389513625626,12.9431483529905,10.1143429235217));
#26222=CARTESIAN_POINT('Ctrl Pts',(157.350282350132,14.6046928759094,7.98809335715339));
#26223=CARTESIAN_POINT('Ctrl Pts',(157.311051074638,15.7312427212271,5.44377552146273));
#26224=CARTESIAN_POINT('Ctrl Pts',(157.271819799143,16.1886477682787,2.78436806056945));
#26225=CARTESIAN_POINT('Ctrl Pts',(157.232588523649,16.6460528153303,0.124960599676174));
#26226=CARTESIAN_POINT('Ctrl Pts',(157.193357248154,16.4343130641158,-2.64953648641971));
#26227=CARTESIAN_POINT('Ctrl Pts',(157.15412597266,15.5786425904199,-5.20873469300084));
#26228=CARTESIAN_POINT('Ctrl Pts',(157.114894697166,14.7229721167239,-7.76793289958189));
#26229=CARTESIAN_POINT('Ctrl Pts',(157.075663421671,13.2233709205465,-10.1118322266482));
#26230=CARTESIAN_POINT('Ctrl Pts',(157.036432146177,11.2584122645379,-11.9613199666181));
#26231=CARTESIAN_POINT('Ctrl Pts',(156.997200870682,9.29345360852907,-13.8108077065882));
#26232=CARTESIAN_POINT('Ctrl Pts',(156.957969595188,6.86313749268894,-15.1658838594618));
#26233=CARTESIAN_POINT('Ctrl Pts',(156.918738319694,4.25686717915344,-15.8651852772402));
#26234=CARTESIAN_POINT('Ctrl Pts',(156.879507044199,1.65059686561801,-16.5644866950186));
#26235=CARTESIAN_POINT('Ctrl Pts',(156.840275768705,-1.13162764561276,-16.6080133777018));
#26236=CARTESIAN_POINT('Ctrl Pts',(156.80104449321,-3.75849766416033,-15.9905821460826));
#26237=CARTESIAN_POINT('Ctrl Pts',(156.761813217716,-6.38536768270793,-15.3731509144634));
#26238=CARTESIAN_POINT('Ctrl Pts',(156.722581942222,-8.85688320857233,-14.0947617685418));
#26239=CARTESIAN_POINT('Ctrl Pts',(156.683350666727,-10.8787349332059,-12.3076459290621));
#26240=CARTESIAN_POINT('Ctrl Pts',(156.644119391233,-12.9005866578396,-10.5205300895824));
#26241=CARTESIAN_POINT('Ctrl Pts',(156.604888115738,-14.4727745812424,-8.22468755654467));
#26242=CARTESIAN_POINT('Ctrl Pts',(156.565656840244,-15.4080817768764,-5.69350841039195));
#26243=CARTESIAN_POINT('Ctrl Pts',(156.53749017588,-16.0795991701985,-3.87621155841627));
#26244=CARTESIAN_POINT('Ctrl Pts',(156.509323511516,-16.4228216997318,-1.93760502006057));
#26245=CARTESIAN_POINT('Ctrl Pts',(156.481156847152,-16.4245975118847,0.000389008950720526));
#26246=CARTESIAN_POINT('Ctrl Pts',(156.268843152848,-16.4247375848135,0.000397937037689734));
#26247=CARTESIAN_POINT('Ctrl Pts',(156.297717645263,-16.4228472967459,-1.98624915417195));
#26248=CARTESIAN_POINT('Ctrl Pts',(156.326592137678,-16.0617660728888,-3.97356488312194));
#26249=CARTESIAN_POINT('Ctrl Pts',(156.355466630092,-15.3568301421047,-5.83033364067544));
#26250=CARTESIAN_POINT('Ctrl Pts',(156.394697905587,-14.3990458351355,-8.35309336960156));
#26251=CARTESIAN_POINT('Ctrl Pts',(156.433929181081,-12.8064992456994,-10.6348609240325));
#26252=CARTESIAN_POINT('Ctrl Pts',(156.473160456575,-10.7688316204978,-12.4039222790379));
#26253=CARTESIAN_POINT('Ctrl Pts',(156.51239173207,-8.73116399529622,-14.1729836340432));
#26254=CARTESIAN_POINT('Ctrl Pts',(156.551623007564,-6.24837533432913,-15.4293387896229));
#26255=CARTESIAN_POINT('Ctrl Pts',(156.590854283059,-3.61611735672674,-16.0233803436549));
#26256=CARTESIAN_POINT('Ctrl Pts',(156.630085558553,-0.983859379124374,
-16.6174218976868));
#26257=CARTESIAN_POINT('Ctrl Pts',(156.669316834047,1.79786791511326,-16.5491498501711));
#26258=CARTESIAN_POINT('Ctrl Pts',(156.708548109542,4.39781504445652,-15.8266940707716));
#26259=CARTESIAN_POINT('Ctrl Pts',(156.747779385036,6.99776217379977,-15.1042382913721));
#26260=CARTESIAN_POINT('Ctrl Pts',(156.787010660531,9.41592913824868,-13.7275987800887));
#26261=CARTESIAN_POINT('Ctrl Pts',(156.826241936025,11.364359402709,-11.8607064604561));
#26262=CARTESIAN_POINT('Ctrl Pts',(156.865473211519,13.3127896671693,-9.99381414082351));
#26263=CARTESIAN_POINT('Ctrl Pts',(156.904704487014,14.791483231641,-7.63666901284167));
#26264=CARTESIAN_POINT('Ctrl Pts',(156.943935762508,15.6243565247449,-5.06996110070942));
#26265=CARTESIAN_POINT('Ctrl Pts',(156.983167038003,16.4572298178488,-2.50325318857716));
#26266=CARTESIAN_POINT('Ctrl Pts',(157.022398313497,16.6442828395849,0.27301750770553));
#26267=CARTESIAN_POINT('Ctrl Pts',(157.061629588991,16.1632412222978,2.92825128103057));
#26268=CARTESIAN_POINT('Ctrl Pts',(157.100860864486,15.6821996050108,5.58348505435563));
#26269=CARTESIAN_POINT('Ctrl Pts',(157.14009213998,14.5330633487007,8.11768190472299));
#26270=CARTESIAN_POINT('Ctrl Pts',(157.179323415474,12.8526721751827,10.229068400022));
#26271=CARTESIAN_POINT('Ctrl Pts',(157.218554690969,11.1722810016648,12.3404548953211));
#26272=CARTESIAN_POINT('Ctrl Pts',(157.257785966463,8.96063491093908,14.0290310355517));
#26273=CARTESIAN_POINT('Ctrl Pts',(157.297017241958,6.48109782886473,15.093720326935));
#26274=CARTESIAN_POINT('Ctrl Pts',(157.336248517452,4.00156074679037,16.1584096183183));
#26275=CARTESIAN_POINT('Ctrl Pts',(157.375479792946,1.25413267336734,16.5992120608542));
#26276=CARTESIAN_POINT('Ctrl Pts',(157.414711068441,-1.43402127829404,16.3636366785762));
#26277=CARTESIAN_POINT('Ctrl Pts',(157.453942343935,-4.12217522995539,16.1280612962983));
#26278=CARTESIAN_POINT('Ctrl Pts',(157.49317361943,-6.75105505985506,15.2161080892066));
#26279=CARTESIAN_POINT('Ctrl Pts',(157.532404894924,-9.00761243918612,13.736372902643));
#26280=CARTESIAN_POINT('Ctrl Pts',(157.571636170419,-11.2641698185172,12.2566377160794));
#26281=CARTESIAN_POINT('Ctrl Pts',(157.610867445913,-13.1484047472796,10.2091205500439));
#26282=CARTESIAN_POINT('Ctrl Pts',(157.650098721407,-14.4359415850123,7.83764077571543));
#26283=CARTESIAN_POINT('Ctrl Pts',(157.689329996902,-15.7234784227451,5.46616100138692));
#26284=CARTESIAN_POINT('Ctrl Pts',(157.728561272396,-16.4143171694482,2.77071861876541));
#26285=CARTESIAN_POINT('Ctrl Pts',(157.76779254789,-16.4261924006351,0.0722882588242302));
#26286=CARTESIAN_POINT('Ctrl Pts',(157.768142749543,-16.4262984059977,0.0482004676566812));
#26287=CARTESIAN_POINT('Ctrl Pts',(157.768492951196,-16.4263503087819,0.0241124383949297));
#26288=CARTESIAN_POINT('Ctrl Pts',(157.768843152848,-16.4263481654919,2.43998567653511E-5));
#26289=CARTESIAN_POINT('Origin',(157.6,0.,0.));
#26290=CARTESIAN_POINT('',(159.481156847152,-16.4250281341261,-0.000400964822849792));
#26291=CARTESIAN_POINT('',(159.268843152848,-16.4248806122125,-0.000401937761208326));
#26292=CARTESIAN_POINT('',(157.6,-16.425,-2.01148236759953E-15));
#26293=CARTESIAN_POINT('Ctrl Pts',(159.481156847152,-16.4250281341261,-0.000400964822849792));
#26294=CARTESIAN_POINT('Ctrl Pts',(159.450874123381,-16.4229611439312,2.08303035180522));
#26295=CARTESIAN_POINT('Ctrl Pts',(159.420591399611,-16.0249145329238,4.16722913013917));
#26296=CARTESIAN_POINT('Ctrl Pts',(159.390308675841,-15.2512553341834,6.10116651089424));
#26297=CARTESIAN_POINT('Ctrl Pts',(159.351077400346,-14.2489796672177,8.60658282510862));
#26298=CARTESIAN_POINT('Ctrl Pts',(159.311846124852,-12.6163055679695,10.8598123049093));
#26299=CARTESIAN_POINT('Ctrl Pts',(159.272614849357,-10.5476526871368,12.5925392536077));
#26300=CARTESIAN_POINT('Ctrl Pts',(159.233383573863,-8.47899980630407,14.3252662023061));
#26301=CARTESIAN_POINT('Ctrl Pts',(159.194152298369,-5.97436814388689,15.5374906199021));
#26302=CARTESIAN_POINT('Ctrl Pts',(159.154921022874,-3.33201049458475,16.0848602146892));
#26303=CARTESIAN_POINT('Ctrl Pts',(159.11568974738,-0.689652845282527,16.6322298094763));
#26304=CARTESIAN_POINT('Ctrl Pts',(159.076458471885,2.09043079090466,16.5147445814543));
#26305=CARTESIAN_POINT('Ctrl Pts',(159.037227196391,4.67718666007232,15.7463947305075));
#26306=CARTESIAN_POINT('Ctrl Pts',(158.997995920897,7.26394252923991,14.9780448795608));
#26307=CARTESIAN_POINT('Ctrl Pts',(158.958764645402,9.65737063138799,13.5588304056892));
#26308=CARTESIAN_POINT('Ctrl Pts',(158.919533369908,11.5724603475543,11.6577520803283));
#26309=CARTESIAN_POINT('Ctrl Pts',(158.880302094413,13.4875500637206,9.75667375496737));
#26310=CARTESIAN_POINT('Ctrl Pts',(158.841070818919,14.924301393905,7.37373157811711));
#26311=CARTESIAN_POINT('Ctrl Pts',(158.801839543425,15.7116252690259,4.79268749949553));
#26312=CARTESIAN_POINT('Ctrl Pts',(158.76260826793,16.4989491441468,2.21164342087391));
#26313=CARTESIAN_POINT('Ctrl Pts',(158.723376992436,16.6368455642041,-0.567502559519045));
#26314=CARTESIAN_POINT('Ctrl Pts',(158.684145716941,16.1088937543276,-3.21380834430115));
#26315=CARTESIAN_POINT('Ctrl Pts',(158.644914441447,15.5809419444511,-5.86011412908327));
#26316=CARTESIAN_POINT('Ctrl Pts',(158.605683165953,14.3871419046409,-8.37357971825453));
#26317=CARTESIAN_POINT('Ctrl Pts',(158.566451890458,12.6696519424551,-10.4549003686864));
#26318=CARTESIAN_POINT('Ctrl Pts',(158.527220614964,10.9521619802693,-12.5362210191182));
#26319=CARTESIAN_POINT('Ctrl Pts',(158.487989339469,8.71098209570786,-14.1853967308107));
#26320=CARTESIAN_POINT('Ctrl Pts',(158.448758063975,6.21299311361428,-15.2060428327785));
#26321=CARTESIAN_POINT('Ctrl Pts',(158.409526788481,3.71500413152066,-16.2266889347464));
#26322=CARTESIAN_POINT('Ctrl Pts',(158.370295512986,0.960206051894863,-16.6188054269897));
#26323=CARTESIAN_POINT('Ctrl Pts',(158.331064237492,-1.72335838811734,-16.3356988809239));
#26324=CARTESIAN_POINT('Ctrl Pts',(158.291832961997,-4.40692282812948,-16.0525923348582));
#26325=CARTESIAN_POINT('Ctrl Pts',(158.252601686503,-7.01925362852802,-15.0942627504835));
#26326=CARTESIAN_POINT('Ctrl Pts',(158.213370411009,-9.24927312724007,-13.5748284954112));
#26327=CARTESIAN_POINT('Ctrl Pts',(158.174139135514,-11.4792926259521,-12.055394240339));
#26328=CARTESIAN_POINT('Ctrl Pts',(158.13490786002,-13.3270008229777,-9.97485531456915));
#26329=CARTESIAN_POINT('Ctrl Pts',(158.095676584525,-14.572371699393,-7.58096333699378));
#26330=CARTESIAN_POINT('Ctrl Pts',(158.057503338734,-15.7841561231085,-5.25163231968812));
#26331=CARTESIAN_POINT('Ctrl Pts',(158.019330092943,-16.4256540432978,-2.62562199965823));
#26332=CARTESIAN_POINT('Ctrl Pts',(157.981156847152,-16.4263224034013,7.32633077222405E-5));
#26333=CARTESIAN_POINT('Ctrl Pts',(157.768843152848,-16.4263481654919,2.43998567653511E-5));
#26334=CARTESIAN_POINT('Ctrl Pts',(157.80772422669,-16.4261102071114,-2.67434563319392));
#26335=CARTESIAN_POINT('Ctrl Pts',(157.846605300532,-15.7596727937856,-5.34883001203914));
#26336=CARTESIAN_POINT('Ctrl Pts',(157.885486374374,-14.5043647551611,-7.71028050230903));
#26337=CARTESIAN_POINT('Ctrl Pts',(157.924717649868,-13.2377501628293,-10.0930005662402));
#26338=CARTESIAN_POINT('Ctrl Pts',(157.963948925363,-11.371609262495,-12.1570223568418));
#26339=CARTESIAN_POINT('Ctrl Pts',(158.003180200857,-9.1281630486379,-13.6565611239626));
#26340=CARTESIAN_POINT('Ctrl Pts',(158.042411476351,-6.88471683478079,-15.1560998910834));
#26341=CARTESIAN_POINT('Ctrl Pts',(158.081642751846,-4.26396530740087,-16.0911556347235));
#26342=CARTESIAN_POINT('Ctrl Pts',(158.12087402734,-1.57798887296388,-16.3503814479005));
#26343=CARTESIAN_POINT('Ctrl Pts',(158.160105302834,1.10798756147311,-16.6096072610774));
#26344=CARTESIAN_POINT('Ctrl Pts',(158.199336578329,3.85918890296716,-16.1930031437911));
#26345=CARTESIAN_POINT('Ctrl Pts',(158.238567853823,6.34800071575338,-15.1501785232993));
#26346=CARTESIAN_POINT('Ctrl Pts',(158.277799129318,8.8368125285396,-14.1073539028075));
#26347=CARTESIAN_POINT('Ctrl Pts',(158.317030404812,11.063234812618,-12.4383087791102));
#26348=CARTESIAN_POINT('Ctrl Pts',(158.356261680306,12.7621440856132,-10.3417938827408));
#26349=CARTESIAN_POINT('Ctrl Pts',(158.395492955801,14.4610533586083,-8.24527898637131));
#26350=CARTESIAN_POINT('Ctrl Pts',(158.434724231295,15.6324496205203,-5.72129431732967));
#26351=CARTESIAN_POINT('Ctrl Pts',(158.47395550679,16.1368424169009,-3.07039723605181));
#26352=CARTESIAN_POINT('Ctrl Pts',(158.513186782284,16.6412352132814,-0.419500154773992));
#26353=CARTESIAN_POINT('Ctrl Pts',(158.552418057778,16.4786245441306,2.35830933874003));
#26354=CARTESIAN_POINT('Ctrl Pts',(158.591649333273,15.6683741694975,4.93224829663603));
#26355=CARTESIAN_POINT('Ctrl Pts',(158.630880608767,14.8581237948644,7.50618725453202));
#26356=CARTESIAN_POINT('Ctrl Pts',(158.670111884262,13.4002337147489,9.87625567680998));
#26357=CARTESIAN_POINT('Ctrl Pts',(158.709343159756,11.4683102111779,11.7602246269039));
#26358=CARTESIAN_POINT('Ctrl Pts',(158.74857443525,9.53638670760697,13.6441935769979));
#26359=CARTESIAN_POINT('Ctrl Pts',(158.787805710745,7.13042978058057,15.0420630549078));
#26360=CARTESIAN_POINT('Ctrl Pts',(158.827036986239,4.53694198781206,15.7873740620242));
#26361=CARTESIAN_POINT('Ctrl Pts',(158.866268261733,1.94345419504354,16.5326850691405));
#26362=CARTESIAN_POINT('Ctrl Pts',(158.905499537228,-0.837564463467088,
16.6254376054632));
#26363=CARTESIAN_POINT('Ctrl Pts',(158.944730812722,-3.47494889088804,16.0545866524418));
#26364=CARTESIAN_POINT('Ctrl Pts',(158.983962088217,-6.11233331830896,15.4837356994203));
#26365=CARTESIAN_POINT('Ctrl Pts',(159.023193363711,-8.60608351464021,14.2492812570547));
#26366=CARTESIAN_POINT('Ctrl Pts',(159.062424639206,-10.659242455622,12.4982227795519));
#26367=CARTESIAN_POINT('Ctrl Pts',(159.1016559147,-12.7124013966038,10.7471643020491));
#26368=CARTESIAN_POINT('Ctrl Pts',(159.140887190194,-14.3249690822362,8.47950178940902));
#26369=CARTESIAN_POINT('Ctrl Pts',(159.180118465689,-15.3049201436399,5.96526963111059));
#26370=CARTESIAN_POINT('Ctrl Pts',(159.209693361409,-16.0436662100445,4.06989016766049));
#26371=CARTESIAN_POINT('Ctrl Pts',(159.239268257128,-16.4228929943252,2.03438390607463));
#26372=CARTESIAN_POINT('Ctrl Pts',(159.268843152848,-16.4248806122125,-0.000401937761208326));
#26373=CARTESIAN_POINT('Origin',(157.6,0.,0.));
#26374=CARTESIAN_POINT('',(160.981156847152,-16.4236740929622,-4.03570622692362E-5));
#26375=CARTESIAN_POINT('',(160.768843152848,-16.4236679926984,2.89616052317413E-6));
#26376=CARTESIAN_POINT('',(157.6,-16.425,-2.01148236759953E-15));
#26377=CARTESIAN_POINT('Ctrl Pts',(160.981156847152,-16.4236740929622,-4.03570622692362E-5));
#26378=CARTESIAN_POINT('Ctrl Pts',(160.960880704809,-16.4235519097392,1.39527506482232));
#26379=CARTESIAN_POINT('Ctrl Pts',(160.940604562465,-16.2475393266592,2.79062075644783));
#26380=CARTESIAN_POINT('Ctrl Pts',(160.920328420122,-15.8960160304352,4.14025318335245));
#26381=CARTESIAN_POINT('Ctrl Pts',(160.881097144628,-15.2158715017878,6.7515882519092));
#26382=CARTESIAN_POINT('Ctrl Pts',(160.841865869133,-13.8786778735385,9.19178926895033));
#26383=CARTESIAN_POINT('Ctrl Pts',(160.802634593639,-12.0436688336838,11.1702758733465));
#26384=CARTESIAN_POINT('Ctrl Pts',(160.763403318144,-10.2086597938292,13.1487624777426));
#26385=CARTESIAN_POINT('Ctrl Pts',(160.72417204265,-7.8758353423693,14.6655346694938));
#26386=CARTESIAN_POINT('Ctrl Pts',(160.684940767156,-5.32298938514325,15.5399744551839));
#26387=CARTESIAN_POINT('Ctrl Pts',(160.645709491661,-2.77014342791723,16.4144142408739));
#26388=CARTESIAN_POINT('Ctrl Pts',(160.606478216167,0.00272403507491303,
16.6465216205029));
#26389=CARTESIAN_POINT('Ctrl Pts',(160.567246940672,2.66541855545244,16.2086571308781));
#26390=CARTESIAN_POINT('Ctrl Pts',(160.528015665178,5.32811307583003,15.7707926412532));
#26391=CARTESIAN_POINT('Ctrl Pts',(160.488784389684,7.88063465359301,14.6629562823745));
#26392=CARTESIAN_POINT('Ctrl Pts',(160.449553114189,10.0190277389006,13.0170697635549));
#26393=CARTESIAN_POINT('Ctrl Pts',(160.410321838695,12.157420824208,11.3711832447354));
#26394=CARTESIAN_POINT('Ctrl Pts',(160.3710905632,13.8816854170602,9.18724656597482));
#26395=CARTESIAN_POINT('Ctrl Pts',(160.331859287706,14.9864952248381,6.72532400245657));
#26396=CARTESIAN_POINT('Ctrl Pts',(160.292628012212,16.0913050326161,4.26340143893821));
#26397=CARTESIAN_POINT('Ctrl Pts',(160.253396736717,16.57666005532,1.52349299066212));
#26398=CARTESIAN_POINT('Ctrl Pts',(160.214165461223,16.384763973389,-1.16813166999598));
#26399=CARTESIAN_POINT('Ctrl Pts',(160.174934185728,16.1928678914581,-3.85975633065405));
#26400=CARTESIAN_POINT('Ctrl Pts',(160.135702910234,15.3237207048923,-6.50309720369402));
#26401=CARTESIAN_POINT('Ctrl Pts',(160.09647163474,13.8808208966376,-8.783383932038));
#26402=CARTESIAN_POINT('Ctrl Pts',(160.057240359245,12.4379210883829,-11.063670660382));
#26403=CARTESIAN_POINT('Ctrl Pts',(160.018009083751,10.4212686584393,-12.98090324403));
#26404=CARTESIAN_POINT('Ctrl Pts',(159.978777808256,8.07100758972996,-14.3067766652253));
#26405=CARTESIAN_POINT('Ctrl Pts',(159.939546532762,5.7207465210206,-15.6326500864207));
#26406=CARTESIAN_POINT('Ctrl Pts',(159.900315257268,3.03687681354547,-16.3671643451634));
#26407=CARTESIAN_POINT('Ctrl Pts',(159.861083981773,0.338995018316543,-16.4228531150854));
#26408=CARTESIAN_POINT('Ctrl Pts',(159.821852706279,-2.35888677691235,-16.4785418850075));
#26409=CARTESIAN_POINT('Ctrl Pts',(159.782621430785,-5.07078065989505,-15.8554051661089));
#26410=CARTESIAN_POINT('Ctrl Pts',(159.74339015529,-7.47375294674307,-14.6276463914453));
#26411=CARTESIAN_POINT('Ctrl Pts',(159.704158879796,-9.87672523359113,-13.3998876167818));
#26412=CARTESIAN_POINT('Ctrl Pts',(159.664927604301,-11.9707759243045,-11.5675067863533));
#26413=CARTESIAN_POINT('Ctrl Pts',(159.625696328807,-13.5065444122441,-9.34870472858095));
#26414=CARTESIAN_POINT('Ctrl Pts',(159.586465053313,-15.0423129001837,-7.12990267080861));
#26415=CARTESIAN_POINT('Ctrl Pts',(159.547233777818,-16.0197991853496,-4.52467938569242));
#26416=CARTESIAN_POINT('Ctrl Pts',(159.508002502324,-16.3226037105909,-1.84326616882031));
#26417=CARTESIAN_POINT('Ctrl Pts',(159.4990539506,-16.3916726338472,-1.23164280042124));
#26418=CARTESIAN_POINT('Ctrl Pts',(159.490105398876,-16.4256389301963,-0.616055390147352));
#26419=CARTESIAN_POINT('Ctrl Pts',(159.481156847152,-16.4250281341261,-0.000400964822849792));
#26420=CARTESIAN_POINT('Ctrl Pts',(159.268843152848,-16.4248806122125,-0.000401937761208326));
#26421=CARTESIAN_POINT('Ctrl Pts',(159.278499532623,-16.4255295813027,-0.664771646930069));
#26422=CARTESIAN_POINT('Ctrl Pts',(159.288155912397,-16.3859625378202,-1.32906455514114));
#26423=CARTESIAN_POINT('Ctrl Pts',(159.297812292172,-16.3055626961613,-1.98837811710903));
#26424=CARTESIAN_POINT('Ctrl Pts',(159.337043567666,-15.9789197501039,-4.66699190307352));
#26425=CARTESIAN_POINT('Ctrl Pts',(159.376274843161,-14.9782994208139,-7.26341767104574));
#26426=CARTESIAN_POINT('Ctrl Pts',(159.415506118655,-13.4228560790206,-9.46847173819219));
#26427=CARTESIAN_POINT('Ctrl Pts',(159.45473739415,-11.8674127372274,-11.6735258053386));
#26428=CARTESIAN_POINT('Ctrl Pts',(159.493968669644,-9.75714638293084,-13.4872081716593));
#26429=CARTESIAN_POINT('Ctrl Pts',(159.533199945138,-7.34334859212344,-14.6935446312183));
#26430=CARTESIAN_POINT('Ctrl Pts',(159.572431220633,-4.92955080131603,-15.8998810907773));
#26431=CARTESIAN_POINT('Ctrl Pts',(159.611662496127,-2.21222157399777,-16.4988716435747));
#26432=CARTESIAN_POINT('Ctrl Pts',(159.650893771621,0.485058162412974,-16.4191881941259));
#26433=CARTESIAN_POINT('Ctrl Pts',(159.690125047116,3.18233789882364,-16.339504744677));
#26434=CARTESIAN_POINT('Ctrl Pts',(159.72935632261,5.85956814432678,-15.5811472929821));
#26435=CARTESIAN_POINT('Ctrl Pts',(159.768587598105,8.19794297837249,-14.2344214247857));
#26436=CARTESIAN_POINT('Ctrl Pts',(159.807818873599,10.5363178124183,-12.8876955565893));
#26437=CARTESIAN_POINT('Ctrl Pts',(159.847050149093,12.5358372350066,-10.9526012718913));
#26438=CARTESIAN_POINT('Ctrl Pts',(159.886281424588,13.9583974703242,-8.65957056876912));
#26439=CARTESIAN_POINT('Ctrl Pts',(159.925512700082,15.3809577056418,-6.36653986564693));
#26440=CARTESIAN_POINT('Ctrl Pts',(159.964743975577,16.2265587536887,-3.71557274410037));
#26441=CARTESIAN_POINT('Ctrl Pts',(160.003975251071,16.3945060175047,-1.02234769870506));
#26442=CARTESIAN_POINT('Ctrl Pts',(160.043206526566,16.5624532813207,1.67087734669029));
#26443=CARTESIAN_POINT('Ctrl Pts',(160.08243780206,16.0527467609058,4.40636031593449));
#26444=CARTESIAN_POINT('Ctrl Pts',(160.121669077554,14.926082564383,6.8583585249146));
#26445=CARTESIAN_POINT('Ctrl Pts',(160.160900353049,13.7994183678601,9.3103567338947));
#26446=CARTESIAN_POINT('Ctrl Pts',(160.200131628543,12.0557964952294,11.4788701826107));
#26447=CARTESIAN_POINT('Ctrl Pts',(160.239362904037,9.90284831369518,13.1056712018496));
#26448=CARTESIAN_POINT('Ctrl Pts',(160.278594179532,7.74990013216097,14.7324722210885));
#26449=CARTESIAN_POINT('Ctrl Pts',(160.317825455026,5.18762564172333,15.8175608108503));
#26450=CARTESIAN_POINT('Ctrl Pts',(160.357056730521,2.52114177395646,16.231724077579));
#26451=CARTESIAN_POINT('Ctrl Pts',(160.396288006015,-0.145342093810331,
16.6458873443076));
#26452=CARTESIAN_POINT('Ctrl Pts',(160.435519281509,-2.91603533890632,16.3891252880031));
#26453=CARTESIAN_POINT('Ctrl Pts',(160.474750557004,-5.46100241990846,15.4920132631237));
#26454=CARTESIAN_POINT('Ctrl Pts',(160.513981832498,-8.00596950091064,14.5949012382442));
#26455=CARTESIAN_POINT('Ctrl Pts',(160.553213107993,-10.325210417819,13.0574392447898));
#26456=CARTESIAN_POINT('Ctrl Pts',(160.592444383487,-12.1425487989022,11.0627090281415));
#26457=CARTESIAN_POINT('Ctrl Pts',(160.631675658981,-13.9598871799855,9.06797881149322));
#26458=CARTESIAN_POINT('Ctrl Pts',(160.670906934476,-15.2753230252437,6.61598037165108));
#26459=CARTESIAN_POINT('Ctrl Pts',(160.71013820997,-15.9322135743927,3.99869891276921));
#26460=CARTESIAN_POINT('Ctrl Pts',(160.729706524263,-16.2598664625444,2.69321532768862));
#26461=CARTESIAN_POINT('Ctrl Pts',(160.749274838555,-16.4236764509222,1.34661012305833));
#26462=CARTESIAN_POINT('Ctrl Pts',(160.768843152848,-16.4236679926984,2.89616052317413E-6));
#26463=CARTESIAN_POINT('Origin',(157.6,0.,0.));
#26464=CARTESIAN_POINT('',(162.481156847152,-16.4247551753985,0.000398700478366487));
#26465=CARTESIAN_POINT('',(162.268843152848,-16.4249001992122,0.000402101984826423));
#26466=CARTESIAN_POINT('',(157.6,-16.425,-2.01148236759953E-15));
#26467=CARTESIAN_POINT('Ctrl Pts',(162.481156847152,-16.4247551753985,0.000398700478366487));
#26468=CARTESIAN_POINT('Ctrl Pts',(162.470887286236,-16.4254300789369,0.706971482165368));
#26469=CARTESIAN_POINT('Ctrl Pts',(162.46061772532,-16.38066296943,1.41345935288586));
#26470=CARTESIAN_POINT('Ctrl Pts',(162.450348164403,-16.2897574053744,2.11395972898341));
#26471=CARTESIAN_POINT('Ctrl Pts',(162.411116888909,-15.9424844054321,4.78997708386633));
#26472=CARTESIAN_POINT('Ctrl Pts',(162.371885613415,-14.9218873213385,7.37861560534905));
#26473=CARTESIAN_POINT('Ctrl Pts',(162.33265433792,-13.3494993657526,9.57161891980958));
#26474=CARTESIAN_POINT('Ctrl Pts',(162.293423062426,-11.7771114101666,11.7646222342701));
#26475=CARTESIAN_POINT('Ctrl Pts',(162.254191786932,-9.65293258308827,13.5619903417085));
#26476=CARTESIAN_POINT('Ctrl Pts',(162.214960511437,-7.22991116477318,14.749691746323));
#26477=CARTESIAN_POINT('Ctrl Pts',(162.175729235943,-4.80688974645808,15.9373931509376));
#26478=CARTESIAN_POINT('Ctrl Pts',(162.136497960448,-2.08502573690623,16.5154278527283));
#26479=CARTESIAN_POINT('Ctrl Pts',(162.097266684954,0.611559932333494,16.4149631894586));
#26480=CARTESIAN_POINT('Ctrl Pts',(162.058035409459,3.30814560157322,16.314498526189));
#26481=CARTESIAN_POINT('Ctrl Pts',(162.018804133965,5.97945293050085,15.5355344978588));
#26482=CARTESIAN_POINT('Ctrl Pts',(161.979572858471,8.30738130243708,14.1708305316958));
#26483=CARTESIAN_POINT('Ctrl Pts',(161.940341582976,10.6353096743733,12.8061265655328));
#26484=CARTESIAN_POINT('Ctrl Pts',(161.901110307482,12.6198590893181,10.8556826615369));
#26485=CARTESIAN_POINT('Ctrl Pts',(161.861879031988,14.0247084074806,8.55175865815035));
#26486=CARTESIAN_POINT('Ctrl Pts',(161.822647756493,15.429557725643,6.24783465476382));
#26487=CARTESIAN_POINT('Ctrl Pts',(161.783416480999,16.254706947023,3.5904305519868));
#26488=CARTESIAN_POINT('Ctrl Pts',(161.744185205504,16.4018968884372,0.895991363348477));
#26489=CARTESIAN_POINT('Ctrl Pts',(161.70495393001,16.5490868298513,-1.79844782528973));
#26490=CARTESIAN_POINT('Ctrl Pts',(161.665722654515,16.0183174912997,-4.52992209978915));
#26491=CARTESIAN_POINT('Ctrl Pts',(161.626491379021,14.872793151855,-6.97316613341791));
#26492=CARTESIAN_POINT('Ctrl Pts',(161.587260103527,13.7272688124102,-9.41641016704681));
#26493=CARTESIAN_POINT('Ctrl Pts',(161.548028828032,11.9669894720722,-11.571423959805));
#26494=CARTESIAN_POINT('Ctrl Pts',(161.508797552538,9.80157007765527,-13.1815873882825));
#26495=CARTESIAN_POINT('Ctrl Pts',(161.469566277044,7.63615068323841,-14.7917508167599));
#26496=CARTESIAN_POINT('Ctrl Pts',(161.430335001549,5.0655912347426,-15.8570638809565));
#26497=CARTESIAN_POINT('Ctrl Pts',(161.391103726055,2.3959952407036,-16.2506685668203));
#26498=CARTESIAN_POINT('Ctrl Pts',(161.35187245056,-0.273600753335407,-16.644273252684));
#26499=CARTESIAN_POINT('Ctrl Pts',(161.312641175066,-3.04223329291763,-16.3661695602148));
#26500=CARTESIAN_POINT('Ctrl Pts',(161.273409899572,-5.58021222646632,-15.4494742166104));
#26501=CARTESIAN_POINT('Ctrl Pts',(161.234178624077,-8.11819116001507,-14.532778873006));
#26502=CARTESIAN_POINT('Ctrl Pts',(161.194947348583,-10.4255164875303,-12.9774918782664));
#26503=CARTESIAN_POINT('Ctrl Pts',(161.155716073088,-12.2274307516426,-10.9688175878669));
#26504=CARTESIAN_POINT('Ctrl Pts',(161.116484797594,-14.0293450157549,-8.96014329746748));
#26505=CARTESIAN_POINT('Ctrl Pts',(161.0772535221,-15.3258482164643,-6.49808171140809));
#26506=CARTESIAN_POINT('Ctrl Pts',(161.038022246605,-15.9625521022962,-3.87581635834224));
#26507=CARTESIAN_POINT('Ctrl Pts',(161.019067113454,-16.2701843875503,-2.60883259861186));
#26508=CARTESIAN_POINT('Ctrl Pts',(161.000111980303,-16.4237883158366,-1.30444970484835));
#26509=CARTESIAN_POINT('Ctrl Pts',(160.981156847152,-16.4236740929622,-4.03570622692362E-5));
#26510=CARTESIAN_POINT('Ctrl Pts',(160.768843152848,-16.4236679926984,2.89616052317413E-6));
#26511=CARTESIAN_POINT('Ctrl Pts',(160.78850611405,-16.4236594935644,-1.35311752394874));
#26512=CARTESIAN_POINT('Ctrl Pts',(160.808169075252,-16.2582440199641,-2.70623998593522));
#26513=CARTESIAN_POINT('Ctrl Pts',(160.827832036453,-15.9274463816101,-4.01764534721292));
#26514=CARTESIAN_POINT('Ctrl Pts',(160.867063311948,-15.2674433866387,-6.63414367039156));
#26515=CARTESIAN_POINT('Ctrl Pts',(160.906294587442,-13.9490921436561,-9.0845758388273));
#26516=CARTESIAN_POINT('Ctrl Pts',(160.945525862937,-12.12938257997,-11.0771431607507));
#26517=CARTESIAN_POINT('Ctrl Pts',(160.984757138431,-10.3096730162838,-13.0697104826741));
#26518=CARTESIAN_POINT('Ctrl Pts',(161.023988413925,-7.98860513189412,-14.6044129580852));
#26519=CARTESIAN_POINT('Ctrl Pts',(161.06321968942,-5.44257285473611,-15.4984974463957));
#26520=CARTESIAN_POINT('Ctrl Pts',(161.102450964914,-2.89654057757807,-16.3925819347062));
#26521=CARTESIAN_POINT('Ctrl Pts',(161.141682240409,-0.125543907651698,
-16.6460484359161));
#26522=CARTESIAN_POINT('Ctrl Pts',(161.180913515903,2.54044548163889,-16.2287140319209));
#26523=CARTESIAN_POINT('Ctrl Pts',(161.220144791397,5.20643487092948,-15.8113796279257));
#26524=CARTESIAN_POINT('Ctrl Pts',(161.259376066892,7.76741697958431,-14.7232443187254));
#26525=CARTESIAN_POINT('Ctrl Pts',(161.298607342386,9.91842877350012,-13.093883802755));
#26526=CARTESIAN_POINT('Ctrl Pts',(161.33783861788,12.0694405674159,-11.4645232867847));
#26527=CARTESIAN_POINT('Ctrl Pts',(161.377069893375,13.8104820465927,-9.29393756404428));
#26528=CARTESIAN_POINT('Ctrl Pts',(161.416301168869,14.9342291183729,-6.84060107117715));
#26529=CARTESIAN_POINT('Ctrl Pts',(161.455532444364,16.057976190153,-4.38726457831001));
#26530=CARTESIAN_POINT('Ctrl Pts',(161.494763719858,16.5644288545364,-1.65117731531621));
#26531=CARTESIAN_POINT('Ctrl Pts',(161.533994995353,16.3932784742086,1.04184607408865));
#26532=CARTESIAN_POINT('Ctrl Pts',(161.573226270847,16.2221280938808,3.73486946349348));
#26533=CARTESIAN_POINT('Ctrl Pts',(161.612457546341,15.3733746688418,6.3848289793093));
#26534=CARTESIAN_POINT('Ctrl Pts',(161.651688821836,13.9480881826851,8.6761661131565));
#26535=CARTESIAN_POINT('Ctrl Pts',(161.69092009733,12.5228016965284,10.9675032470038));
#26536=CARTESIAN_POINT('Ctrl Pts',(161.730151372824,10.5209821492541,12.9002179988825));
#26537=CARTESIAN_POINT('Ctrl Pts',(161.769382648319,8.18100721667673,14.244161726677));
#26538=CARTESIAN_POINT('Ctrl Pts',(161.808613923813,5.84103228409951,15.5881054544714));
#26539=CARTESIAN_POINT('Ctrl Pts',(161.847845199308,3.16290196621933,16.3432781581817));
#26540=CARTESIAN_POINT('Ctrl Pts',(161.887076474802,0.465529364656197,16.4197534934507));
#26541=CARTESIAN_POINT('Ctrl Pts',(161.926307750296,-2.23184323690693,16.4962288287198));
#26542=CARTESIAN_POINT('Ctrl Pts',(161.965539025791,-4.94845812215303,15.8940067955476));
#26543=CARTESIAN_POINT('Ctrl Pts',(162.004770301285,-7.36081942787581,14.6848002957225));
#26544=CARTESIAN_POINT('Ctrl Pts',(162.04400157678,-9.77318073359862,13.4755937958975));
#26545=CARTESIAN_POINT('Ctrl Pts',(162.083232852274,-11.8812884597981,11.6594028294195));
#26546=CARTESIAN_POINT('Ctrl Pts',(162.122464127769,-13.4341080809988,9.4525003275898));
#26547=CARTESIAN_POINT('Ctrl Pts',(162.161695403263,-14.9869277021995,7.24559782576006));
#26548=CARTESIAN_POINT('Ctrl Pts',(162.200926678757,-15.9844592184014,4.6479837885785));
#26549=CARTESIAN_POINT('Ctrl Pts',(162.240157954252,-16.3079160762864,1.96898339857192));
#26550=CARTESIAN_POINT('Ctrl Pts',(162.249719687117,-16.386751343038,1.31603786588246));
#26551=CARTESIAN_POINT('Ctrl Pts',(162.259281419983,-16.4255445549274,0.658257739925561));
#26552=CARTESIAN_POINT('Ctrl Pts',(162.268843152848,-16.4249001992122,0.000402101984826423));
#26553=CARTESIAN_POINT('Origin',(157.6,0.,0.));
#26554=CARTESIAN_POINT('',(163.981156847152,-16.426349720506,1.83455734200678E-5));
#26555=CARTESIAN_POINT('',(163.768843152848,-16.4263461654774,-3.0980125475399E-5));
#26556=CARTESIAN_POINT('',(157.6,-16.425,-2.01148236759953E-15));
#26557=CARTESIAN_POINT('Ctrl Pts',(163.981156847152,-16.426349720506,1.83455734200678E-5));
#26558=CARTESIAN_POINT('Ctrl Pts',(163.980893867663,-16.4263509381512,0.0181069480969145));
#26559=CARTESIAN_POINT('Ctrl Pts',(163.980630888174,-16.4263216708674,0.0361955466634846));
#26560=CARTESIAN_POINT('Ctrl Pts',(163.980367908685,-16.4262618946208,0.054284044404482));
#26561=CARTESIAN_POINT('Ctrl Pts',(163.94113663319,-16.4173444752216,2.75272581608827));
#26562=CARTESIAN_POINT('Ctrl Pts',(163.901905357696,-15.7294602457597,5.44892374822015));
#26563=CARTESIAN_POINT('Ctrl Pts',(163.862674082202,-14.444523408231,7.82181331292719));
#26564=CARTESIAN_POINT('Ctrl Pts',(163.823442806707,-13.1595865707024,10.1947028776342));
#26565=CARTESIAN_POINT('Ctrl Pts',(163.784211531213,-11.2775971251071,12.2442840749163));
#26566=CARTESIAN_POINT('Ctrl Pts',(163.744980255719,-9.02266302473022,13.7264917114902));
#26567=CARTESIAN_POINT('Ctrl Pts',(163.705748980224,-6.76772892435329,15.2086993480642));
#26568=CARTESIAN_POINT('Ctrl Pts',(163.66651770473,-4.13985016919475,16.1235334239298));
#26569=CARTESIAN_POINT('Ctrl Pts',(163.627286429235,-1.45195602286144,16.3620550561079));
#26570=CARTESIAN_POINT('Ctrl Pts',(163.588055153741,1.23593812347187,16.6005766882859));
#26571=CARTESIAN_POINT('Ctrl Pts',(163.548823878247,3.98384766097998,16.1627858767762));
#26572=CARTESIAN_POINT('Ctrl Pts',(163.509592602752,6.46455021341737,15.1008149624023));
#26573=CARTESIAN_POINT('Ctrl Pts',(163.470361327258,8.94525276585476,14.0388440480284));
#26574=CARTESIAN_POINT('Ctrl Pts',(163.431130051763,11.1587483332215,12.3526930307903));
#26575=CARTESIAN_POINT('Ctrl Pts',(163.391898776269,12.8414527190008,10.2431496238017));
#26576=CARTESIAN_POINT('Ctrl Pts',(163.352667500774,14.5241571047801,8.13360621681312));
#26577=CARTESIAN_POINT('Ctrl Pts',(163.31343622528,15.676070308972,5.60067042007414));
#26578=CARTESIAN_POINT('Ctrl Pts',(163.274204949786,16.1600219460145,2.94596549675071));
#26579=CARTESIAN_POINT('Ctrl Pts',(163.234973674291,16.643973583057,0.291260573427248));
#26580=CARTESIAN_POINT('Ctrl Pts',(163.195742398797,16.45996365295,-2.48521347648057));
#26581=CARTESIAN_POINT('Ctrl Pts',(163.156511123302,15.6299041423788,-5.05283272941568));
#26582=CARTESIAN_POINT('Ctrl Pts',(163.117279847808,14.7998446318076,-7.62045198235076));
#26583=CARTESIAN_POINT('Ctrl Pts',(163.078048572314,13.3237355407723,-9.97921643831304));
#26584=CARTESIAN_POINT('Ctrl Pts',(163.038817296819,11.3773526842037,-11.8482432432018));
#26585=CARTESIAN_POINT('Ctrl Pts',(162.999586021325,9.43096982763521,-13.7172700480906));
#26586=CARTESIAN_POINT('Ctrl Pts',(162.960354745831,7.01431320553354,-15.0965592019059));
#26587=CARTESIAN_POINT('Ctrl Pts',(162.921123470336,4.41515949874548,-15.8218642601142));
#26588=CARTESIAN_POINT('Ctrl Pts',(162.881892194842,1.81600579195742,-16.5471693183225));
#26589=CARTESIAN_POINT('Ctrl Pts',(162.842660919347,-0.965644999517052,
-16.6184902809239));
#26590=CARTESIAN_POINT('Ctrl Pts',(162.803429643853,-3.59855250319817,-16.0273342120322));
#26591=CARTESIAN_POINT('Ctrl Pts',(162.764198368359,-6.23146000687928,-15.4361781431406));
#26592=CARTESIAN_POINT('Ctrl Pts',(162.724967092864,-8.71562422276706,-14.182545042756));
#26593=CARTESIAN_POINT('Ctrl Pts',(162.68573581737,-10.7552296304183,-12.4157181692461));
#26594=CARTESIAN_POINT('Ctrl Pts',(162.646504541875,-12.7948350380696,-10.6488912957361));
#26595=CARTESIAN_POINT('Ctrl Pts',(162.607273266381,-14.3898816374843,-8.36887064910085));
#26596=CARTESIAN_POINT('Ctrl Pts',(162.568041990887,-15.3504304792961,-5.84716223164164));
#26597=CARTESIAN_POINT('Ctrl Pts',(162.539080276308,-16.0595366973441,-3.98556077933925));
#26598=CARTESIAN_POINT('Ctrl Pts',(162.51011856173,-16.4228518453724,-1.99224338023886));
#26599=CARTESIAN_POINT('Ctrl Pts',(162.481156847152,-16.4247551753985,0.000398700478366487));
#26600=CARTESIAN_POINT('Ctrl Pts',(162.268843152848,-16.4249001992122,0.000402101984826423));
#26601=CARTESIAN_POINT('Ctrl Pts',(162.298512695477,-16.4229007980964,-2.04088854774718));
#26602=CARTESIAN_POINT('Ctrl Pts',(162.328182238106,-16.041185646821,-4.08290624763289));
#26603=CARTESIAN_POINT('Ctrl Pts',(162.357851780735,-15.2978144185396,-5.98346859195882));
#26604=CARTESIAN_POINT('Ctrl Pts',(162.397083056229,-14.3148737033398,-8.49653344965138));
#26605=CARTESIAN_POINT('Ctrl Pts',(162.436314331724,-12.699610073372,-10.7622764222049));
#26606=CARTESIAN_POINT('Ctrl Pts',(162.475545607218,-10.6443699319163,-12.5108916999377));
#26607=CARTESIAN_POINT('Ctrl Pts',(162.514776882712,-8.58912979046056,-14.2595069776706));
#26608=CARTESIAN_POINT('Ctrl Pts',(162.554008158207,-6.09391313751689,-15.4909945605828));
#26609=CARTESIAN_POINT('Ctrl Pts',(162.593239433701,-3.45585162373997,-16.0587082895774));
#26610=CARTESIAN_POINT('Ctrl Pts',(162.632470709196,-0.817790109963057,
-16.6264220185721));
#26611=CARTESIAN_POINT('Ctrl Pts',(162.67170198469,1.96311626464708,-16.5303618936492));
#26612=CARTESIAN_POINT('Ctrl Pts',(162.710933260184,4.55571577409399,-15.7819668026727));
#26613=CARTESIAN_POINT('Ctrl Pts',(162.750164535679,7.1483152835409,-15.0335717116962));
#26614=CARTESIAN_POINT('Ctrl Pts',(162.789395811173,9.55260792782455,-13.6328416546661));
#26615=CARTESIAN_POINT('Ctrl Pts',(162.828627086668,11.4822893328306,-11.7465762693808));
#26616=CARTESIAN_POINT('Ctrl Pts',(162.867858362162,13.4119707378367,-9.86031088409554));
#26617=CARTESIAN_POINT('Ctrl Pts',(162.907089637656,14.8670409035652,-7.4885101705551));
#26618=CARTESIAN_POINT('Ctrl Pts',(162.946320913151,15.6742293448598,-4.91360934745356));
#26619=CARTESIAN_POINT('Ctrl Pts',(162.985552188645,16.4814177861543,-2.33870852435206));
#26620=CARTESIAN_POINT('Ctrl Pts',(163.02478346414,16.6407245030151,0.439292408310395));
#26621=CARTESIAN_POINT('Ctrl Pts',(163.064014739634,16.1331791715844,3.08958770604198));
#26622=CARTESIAN_POINT('Ctrl Pts',(163.103246015128,15.6256338401538,5.73988300377354));
#26623=CARTESIAN_POINT('Ctrl Pts',(163.142477290623,14.4512364604316,8.26247266657433));
#26624=CARTESIAN_POINT('Ctrl Pts',(163.181708566117,12.7498348616949,10.3569654519852));
#26625=CARTESIAN_POINT('Ctrl Pts',(163.220939841612,11.0484332629582,12.4514582373962));
#26626=CARTESIAN_POINT('Ctrl Pts',(163.260171117106,8.82002744520687,14.1178541454175));
#26627=CARTESIAN_POINT('Ctrl Pts',(163.2994023926,6.32997709056114,15.157717915582));
#26628=CARTESIAN_POINT('Ctrl Pts',(163.338633668095,3.83992673591541,16.1975816857465));
#26629=CARTESIAN_POINT('Ctrl Pts',(163.377864943589,1.08823184437532,16.6109133180543));
#26630=CARTESIAN_POINT('Ctrl Pts',(163.417096219084,-1.59743437520489,16.348493074124));
#26631=CARTESIAN_POINT('Ctrl Pts',(163.456327494578,-4.2831005947851,16.0860728301938));
#26632=CARTESIAN_POINT('Ctrl Pts',(163.495558770072,-6.90273814240541,15.1479007100255));
#26633=CARTESIAN_POINT('Ctrl Pts',(163.534790045567,-9.14439926671966,13.6456947208487));
#26634=CARTESIAN_POINT('Ctrl Pts',(163.574021321061,-11.3860603910339,12.1434887316718));
#26635=CARTESIAN_POINT('Ctrl Pts',(163.613252596556,-13.249745092042,10.0772488734865));
#26636=CARTESIAN_POINT('Ctrl Pts',(163.65248387205,-14.5135248569151,7.69302402388132));
#26637=CARTESIAN_POINT('Ctrl Pts',(163.691270298983,-15.7629744578162,5.33583421154308));
#26638=CARTESIAN_POINT('Ctrl Pts',(163.730056725915,-16.4260467902704,2.66782986936085));
#26639=CARTESIAN_POINT('Ctrl Pts',(163.768843152848,-16.4263461654774,-3.0980125475399E-5));
#26640=CARTESIAN_POINT('Origin',(157.6,0.,0.));
#26641=CARTESIAN_POINT('',(165.275,-16.425,-2.01148236759953E-15));
#26642=CARTESIAN_POINT('',(165.268843152848,-16.4247445391107,-0.000389063610209933));
#26643=CARTESIAN_POINT('',(157.6,-16.425,-2.01148236759953E-15));
#26644=CARTESIAN_POINT('',(165.275,-10.6720568218313,12.4855047231421));
#26645=CARTESIAN_POINT('Origin',(165.275,0.,0.));
#26646=CARTESIAN_POINT('Ctrl Pts',(165.275,-10.6720568218312,12.4855047231422));
#26647=CARTESIAN_POINT('Ctrl Pts',(165.235768724506,-8.6202940722137,14.2392607093338));
#26648=CARTESIAN_POINT('Ctrl Pts',(165.196537449011,-6.12897562101673,15.4767795574399));
#26649=CARTESIAN_POINT('Ctrl Pts',(165.157306173517,-3.49257059628647,16.0506648722972));
#26650=CARTESIAN_POINT('Ctrl Pts',(165.118074898022,-0.856165571556061,
16.6245501871546));
#26651=CARTESIAN_POINT('Ctrl Pts',(165.078843622528,1.92532602670759,16.5348019687632));
#26652=CARTESIAN_POINT('Ctrl Pts',(165.039612347034,4.51972495057751,15.7923235953478));
#26653=CARTESIAN_POINT('Ctrl Pts',(165.000381071539,7.11412387444743,15.0498452219324));
#26654=CARTESIAN_POINT('Ctrl Pts',(164.961149796045,9.52143012392356,13.654636693493));
#26655=CARTESIAN_POINT('Ctrl Pts',(164.92191852055,11.4553706815436,11.7727924865797));
#26656=CARTESIAN_POINT('Ctrl Pts',(164.882687245056,13.3893112391636,9.89094827966651));
#26657=CARTESIAN_POINT('Ctrl Pts',(164.843455969562,14.8498861049275,7.52246839427947));
#26658=CARTESIAN_POINT('Ctrl Pts',(164.804224694067,15.6629797279521,4.94941629810398));
#26659=CARTESIAN_POINT('Ctrl Pts',(164.764993418573,16.4760733509766,2.37636420192853));
#26660=CARTESIAN_POINT('Ctrl Pts',(164.725762143078,16.6416857312619,-0.401260105035436));
#26661=CARTESIAN_POINT('Ctrl Pts',(164.686530867584,16.1401878137618,-3.052707085354));
#26662=CARTESIAN_POINT('Ctrl Pts',(164.64729959209,15.6386898962617,-5.70415406567245));
#26663=CARTESIAN_POINT('Ctrl Pts',(164.608068316595,14.4700816809762,-8.22942371934558));
#26664=CARTESIAN_POINT('Ctrl Pts',(164.568837041101,12.773476700623,-10.3278001313319));
#26665=CARTESIAN_POINT('Ctrl Pts',(164.529605765607,11.0768717202696,-12.4261765433184));
#26666=CARTESIAN_POINT('Ctrl Pts',(164.490374490112,8.85226997484841,-14.0976597136181));
#26667=CARTESIAN_POINT('Ctrl Pts',(164.451143214618,6.36460005341017,-15.1432112869903));
#26668=CARTESIAN_POINT('Ctrl Pts',(164.411911939123,3.87693013197185,-16.1887628603625));
#26669=CARTESIAN_POINT('Ctrl Pts',(164.372680663629,1.1261920345165,-16.6083828368073));
#26670=CARTESIAN_POINT('Ctrl Pts',(164.333449388134,-1.56006564138621,-16.3521013432403));
#26671=CARTESIAN_POINT('Ctrl Pts',(164.29421811264,-4.24632331728882,-16.0958198496733));
#26672=CARTESIAN_POINT('Ctrl Pts',(164.254986837146,-6.86810057163888,-15.1636368860945));
#26673=CARTESIAN_POINT('Ctrl Pts',(164.215755561651,-9.11318964993117,-13.6665579088443));
#26674=CARTESIAN_POINT('Ctrl Pts',(164.176524286157,-11.3582787282235,-12.169478931594));
#26675=CARTESIAN_POINT('Ctrl Pts',(164.137293010662,-13.2266796304581,-10.1075039406724));
#26676=CARTESIAN_POINT('Ctrl Pts',(164.098061735168,-14.4959047769073,-7.72617363959368));
#26677=CARTESIAN_POINT('Ctrl Pts',(164.059093439163,-15.7566219109044,-5.36080613905552));
#26678=CARTESIAN_POINT('Ctrl Pts',(164.020125143157,-16.4261692898643,-2.68035045503792));
#26679=CARTESIAN_POINT('Ctrl Pts',(163.981156847152,-16.426349720506,1.83455734200678E-5));
#26680=CARTESIAN_POINT('Ctrl Pts',(163.768843152848,-16.4263461654774,-3.0980125475399E-5));
#26681=CARTESIAN_POINT('Ctrl Pts',(163.76928800141,-16.4263495990659,-0.0306291598356519));
#26682=CARTESIAN_POINT('Ctrl Pts',(163.769732849971,-16.426265850095,-0.0612273206704939));
#26683=CARTESIAN_POINT('Ctrl Pts',(163.770177698533,-16.4260948033082,-0.0918249934937266));
#26684=CARTESIAN_POINT('Ctrl Pts',(163.809408974028,-16.4110101560904,-2.79023932023853));
#26685=CARTESIAN_POINT('Ctrl Pts',(163.848640249522,-15.7169660329169,-5.48485813270309));
#26686=CARTESIAN_POINT('Ctrl Pts',(163.887871525016,-14.4266095401332,-7.85480487595506));
#26687=CARTESIAN_POINT('Ctrl Pts',(163.927102800511,-13.1362530473495,-10.224751619207));
#26688=CARTESIAN_POINT('Ctrl Pts',(163.966334076005,-11.2495841849556,-12.2700262932464));
#26689=CARTESIAN_POINT('Ctrl Pts',(164.0055653515,-8.99126846022917,-13.7470765539275));
#26690=CARTESIAN_POINT('Ctrl Pts',(164.044796626994,-6.73295273550269,-15.2241268146085));
#26691=CARTESIAN_POINT('Ctrl Pts',(164.084027902488,-4.10299014844364,-16.1329526619312));
#26692=CARTESIAN_POINT('Ctrl Pts',(164.123259177983,-1.41455789588256,-16.3653306787166));
#26693=CARTESIAN_POINT('Ctrl Pts',(164.162490453477,1.27387435667852,-16.5977086955021));
#26694=CARTESIAN_POINT('Ctrl Pts',(164.201721728972,4.02077627474165,-16.1536388817503));
#26695=CARTESIAN_POINT('Ctrl Pts',(164.240953004466,6.49904526210118,-15.0860012513868));
#26696=CARTESIAN_POINT('Ctrl Pts',(164.28018427996,8.97731424946063,-14.0183636210233));
#26697=CARTESIAN_POINT('Ctrl Pts',(164.319415555455,11.1869503061165,-12.3271581740481));
#26698=CARTESIAN_POINT('Ctrl Pts',(164.358646830949,12.8648291450421,-10.2137745900656));
#26699=CARTESIAN_POINT('Ctrl Pts',(164.397878106443,14.5427079839677,-8.10039100608284));
#26700=CARTESIAN_POINT('Ctrl Pts',(164.437109381938,15.688829605163,-5.5648292850926));
#26701=CARTESIAN_POINT('Ctrl Pts',(164.476340657432,16.1667126905997,-2.90902521091257));
#26702=CARTESIAN_POINT('Ctrl Pts',(164.515571932927,16.6445957760363,-0.253221136732651));
#26703=CARTESIAN_POINT('Ctrl Pts',(164.554803208421,16.4542403257145,2.52282529063697));
#26704=CARTESIAN_POINT('Ctrl Pts',(164.594034483915,15.6183151529188,5.08854070546535));
#26705=CARTESIAN_POINT('Ctrl Pts',(164.63326575941,14.782389980123,7.65425612029377));
#26706=CARTESIAN_POINT('Ctrl Pts',(164.672497034904,13.3008950848533,10.0096405225808));
#26707=CARTESIAN_POINT('Ctrl Pts',(164.711728310399,11.3502451796235,11.8742143043212));
#26708=CARTESIAN_POINT('Ctrl Pts',(164.750959585893,9.39959527439374,13.7387880860616));
#26709=CARTESIAN_POINT('Ctrl Pts',(164.790190861387,6.97979035920383,15.1125512472554));
#26710=CARTESIAN_POINT('Ctrl Pts',(164.829422136882,4.37898702814889,15.8319138469491));
#26711=CARTESIAN_POINT('Ctrl Pts',(164.868653412376,1.77818369709394,16.5512764466429));
#26712=CARTESIAN_POINT('Ctrl Pts',(164.907884687871,-1.00361804982606,16.6162384848367));
#26713=CARTESIAN_POINT('Ctrl Pts',(164.947115963365,-3.63517014472577,16.0190673975602));
#26714=CARTESIAN_POINT('Ctrl Pts',(164.986347238859,-6.26672223962549,15.4218963102837));
#26715=CARTESIAN_POINT('Ctrl Pts',(165.025578514354,-8.74802468250493,14.1625920975368));
#26716=CARTESIAN_POINT('Ctrl Pts',(165.064809789848,-10.7835816465719,12.3911068786316));
#26717=CARTESIAN_POINT('Ctrl Pts',(165.104041065343,-12.8191386106389,10.6196216597264));
#26718=CARTESIAN_POINT('Ctrl Pts',(165.143272340837,-14.4089500958934,8.33595543466287));
#26719=CARTESIAN_POINT('Ctrl Pts',(165.182503616331,-15.3637438128742,5.81206157253249));
#26720=CARTESIAN_POINT('Ctrl Pts',(165.211283461837,-16.0641751732649,3.96054707270523));
#26721=CARTESIAN_POINT('Ctrl Pts',(165.240063307342,-16.4228648636352,1.97975147559551));
#26722=CARTESIAN_POINT('Ctrl Pts',(165.268843152848,-16.4247445391107,-0.000389063610209933));
#26723=CARTESIAN_POINT('Origin',(147.227129595899,0.,0.));
#26724=CARTESIAN_POINT('',(164.477129595899,-15.5672291282746,1.73860745367607E-5));
#26725=CARTESIAN_POINT('',(164.772870404101,-15.5657079000652,-0.000368715050692581));
#26726=CARTESIAN_POINT('',(147.227129595899,-15.56595,-7.64522432085395E-13));
#26727=CARTESIAN_POINT('',(165.275,15.2541446685787,3.10078767190799));
#26728=CARTESIAN_POINT('Ctrl Pts',(164.477129595899,-15.5672291282746,1.73860745367725E-5));
#26729=CARTESIAN_POINT('Ctrl Pts',(164.516097891905,-15.5670581344026,-2.54016445452667));
#26730=CARTESIAN_POINT('Ctrl Pts',(164.594297463404,-14.293717715194,-7.63783591380272));
#26731=CARTESIAN_POINT('Ctrl Pts',(164.711728310399,-8.99354421585697,-13.4871293872258));
#26732=CARTESIAN_POINT('Ctrl Pts',(164.829422136882,-1.53958007844154,-16.1374149400877));
#26733=CARTESIAN_POINT('Ctrl Pts',(164.947115963365,6.2810321020304,-14.9443951095233));
#26734=CARTESIAN_POINT('Ctrl Pts',(165.064809789848,12.6057881822385,-10.1922081771534));
#26735=CARTESIAN_POINT('Ctrl Pts',(165.174104468727,15.6911477082268,-3.52499098687683));
#26736=CARTESIAN_POINT('Ctrl Pts',(165.24416787211,15.652577916973,1.13042150275773));
#26737=CARTESIAN_POINT('Ctrl Pts',(165.275,15.2541446685787,3.100787671908));
#26738=CARTESIAN_POINT('',(165.275,7.90291568084493,-13.4105452217259));
#26739=CARTESIAN_POINT('Origin',(165.275,0.,0.));
#26740=CARTESIAN_POINT('Ctrl Pts',(164.772870404101,-15.5657079000652,-0.000368715050694315));
#26741=CARTESIAN_POINT('Ctrl Pts',(164.78332183409,-15.5663548048828,-0.681849359511778));
#26742=CARTESIAN_POINT('Ctrl Pts',(164.833004539573,-15.3574419571854,-3.92099794181115));
#26743=CARTESIAN_POINT('Ctrl Pts',(164.92191852055,-13.1524493936104,-9.4760867792538));
#26744=CARTESIAN_POINT('Ctrl Pts',(165.039612347034,-7.10203868245562,-14.5722070548038));
#26745=CARTESIAN_POINT('Ctrl Pts',(165.157306173517,0.641239642833148,-16.1982319284135));
#26746=CARTESIAN_POINT('Ctrl Pts',(165.235768724506,5.69913956220702,-14.7092438620197));
#26747=CARTESIAN_POINT('Ctrl Pts',(165.275,7.90291568084474,-13.410545221726));
#26748=CARTESIAN_POINT('Origin',(147.227129595899,0.,0.));
#26749=CARTESIAN_POINT('',(162.977129595899,-15.5657179800606,0.000377847897364862));
#26750=CARTESIAN_POINT('',(163.272870404101,-15.5672257591788,-2.9359822512065E-5));
#26751=CARTESIAN_POINT('',(147.227129595899,-15.56595,-7.64522432085395E-13));
#26752=CARTESIAN_POINT('Ctrl Pts',(162.977129595899,-15.5657179800606,0.000377847897364836));
#26753=CARTESIAN_POINT('Ctrl Pts',(163.006091310478,-15.5639141968021,-1.88804632235174));
#26754=CARTESIAN_POINT('Ctrl Pts',(163.07428430055,-14.7531973033115,-6.33601965434617));
#26755=CARTESIAN_POINT('Ctrl Pts',(163.181708566117,-10.6140241611372,-12.2527121369471));
#26756=CARTESIAN_POINT('Ctrl Pts',(163.2994023926,-3.55130708784071,-15.8169112527338));
#26757=CARTESIAN_POINT('Ctrl Pts',(163.417096219084,4.35719284595873,-15.6141389170616));
#26758=CARTESIAN_POINT('Ctrl Pts',(163.534790045567,11.2279793567904,-11.692687592161));
#26759=CARTESIAN_POINT('Ctrl Pts',(163.65248387205,15.4246990473113,-4.9864940609672));
#26760=CARTESIAN_POINT('Ctrl Pts',(163.770177698533,15.9478569233932,2.90728790015858));
#26761=CARTESIAN_POINT('Ctrl Pts',(163.887871525016,12.672857226445,10.108667254542));
#26762=CARTESIAN_POINT('Ctrl Pts',(164.005565351499,6.37967707542191,14.902556282264));
#26763=CARTESIAN_POINT('Ctrl Pts',(164.123259177983,-1.43289323788845,16.1472375393268));
#26764=CARTESIAN_POINT('Ctrl Pts',(164.240953004466,-8.90420452717788,13.5462765378252));
#26765=CARTESIAN_POINT('Ctrl Pts',(164.358646830949,-14.2548809857467,7.71912065876858));
#26766=CARTESIAN_POINT('Ctrl Pts',(164.437372361427,-15.5630648054341,2.59162629500307));
#26767=CARTESIAN_POINT('Ctrl Pts',(164.47686661641,-15.5672302822353,0.0171599299072187));
#26768=CARTESIAN_POINT('Ctrl Pts',(164.477129595899,-15.5672291282746,1.73860745367725E-5));
#26769=CARTESIAN_POINT('Ctrl Pts',(163.272870404101,-15.5672257591788,-2.93598225131189E-5));
#26770=CARTESIAN_POINT('Ctrl Pts',(163.273315252662,-15.567229013186,-0.0290272128185329));
#26771=CARTESIAN_POINT('Ctrl Pts',(163.312991376719,-15.5601500968341,-2.61534939581951));
#26772=CARTESIAN_POINT('Ctrl Pts',(163.391898776269,-14.2372025145188,-7.75167909617249));
#26773=CARTESIAN_POINT('Ctrl Pts',(163.509592602752,-8.87322202528032,-13.5665911166955));
#26774=CARTESIAN_POINT('Ctrl Pts',(163.627286429235,-1.39598620207817,-16.1504701483178));
#26775=CARTESIAN_POINT('Ctrl Pts',(163.744980255718,6.413719352529,-14.8879370857845));
#26776=CARTESIAN_POINT('Ctrl Pts',(163.862674082202,12.6959265445113,-10.0796778296488));
#26777=CARTESIAN_POINT('Ctrl Pts',(163.980367908685,15.9544602156426,-2.87083272081841));
#26778=CARTESIAN_POINT('Ctrl Pts',(164.098061735168,15.4132614171153,5.0217334684266));
#26779=CARTESIAN_POINT('Ctrl Pts',(164.215755561651,11.2012293687092,11.7183171829071));
#26780=CARTESIAN_POINT('Ctrl Pts',(164.333449388134,4.32149195873656,15.6240575808949));
#26781=CARTESIAN_POINT('Ctrl Pts',(164.451143214618,-3.58743715586971,15.8087508847164));
#26782=CARTESIAN_POINT('Ctrl Pts',(164.568837041101,-10.6420179340868,12.2284282526787));
#26783=CARTESIAN_POINT('Ctrl Pts',(164.676079437595,-14.7606212533428,6.31230839705082));
#26784=CARTESIAN_POINT('Ctrl Pts',(164.744090558595,-15.563926534192,1.87620776143336));
#26785=CARTESIAN_POINT('Ctrl Pts',(164.772870404101,-15.5657079000652,-0.000368715050694315));
#26786=CARTESIAN_POINT('Origin',(147.227129595899,0.,0.));
#26787=CARTESIAN_POINT('',(161.477129595899,-15.5646934397166,-3.82463327799083E-5));
#26788=CARTESIAN_POINT('',(161.772870404101,-15.5658554189301,0.000381071499603314));
#26789=CARTESIAN_POINT('',(147.227129595899,-15.56595,-7.64522432085395E-13));
#26790=CARTESIAN_POINT('Ctrl Pts',(161.477129595899,-15.5646934397166,-3.82463327805449E-5));
#26791=CARTESIAN_POINT('Ctrl Pts',(161.49608472905,-15.5648016885781,-1.23622519836749));
#26792=CARTESIAN_POINT('Ctrl Pts',(161.554271137696,-15.1179460024313,-5.03086065784982));
#26793=CARTESIAN_POINT('Ctrl Pts',(161.651688821836,-12.0668967458695,-10.8248079212624));
#26794=CARTESIAN_POINT('Ctrl Pts',(161.769382648319,-5.50694958937003,-15.2466379844161));
#26795=CARTESIAN_POINT('Ctrl Pts',(161.887076474802,2.3645382059743,-16.0373134495834));
#26796=CARTESIAN_POINT('Ctrl Pts',(162.004770301285,9.67288521004985,-13.0085262547648));
#26797=CARTESIAN_POINT('Ctrl Pts',(162.122464127768,14.67752816854,-6.88161539679513));
#26798=CARTESIAN_POINT('Ctrl Pts',(162.240157954252,16.1865562937323,0.884227887797634));
#26799=CARTESIAN_POINT('Ctrl Pts',(162.357851780735,13.840577933451,8.43948257156437));
#26800=CARTESIAN_POINT('Ctrl Pts',(162.475545607218,8.19831364750381,13.9847816194923));
#26801=CARTESIAN_POINT('Ctrl Pts',(162.593239433701,0.603530758605001,16.1994510472156));
#26802=CARTESIAN_POINT('Ctrl Pts',(162.710933260184,-7.13498962120933,14.5560429620394));
#26803=CARTESIAN_POINT('Ctrl Pts',(162.828627086668,-13.1742337149738,9.44595308222564));
#26804=CARTESIAN_POINT('Ctrl Pts',(162.917359198573,-15.361859159625,3.89726831243747));
#26805=CARTESIAN_POINT('Ctrl Pts',(162.966860034983,-15.5663575852194,0.669995905194144));
#26806=CARTESIAN_POINT('Ctrl Pts',(162.977129595899,-15.5657179800606,0.000377847897364836));
#26807=CARTESIAN_POINT('Ctrl Pts',(161.772870404101,-15.5658554189301,0.000381071499603106));
#26808=CARTESIAN_POINT('Ctrl Pts',(161.80253994673,-15.5639605892315,-1.93414728096267));
#26809=CARTESIAN_POINT('Ctrl Pts',(161.871440764853,-14.7238756891141,-6.42825297656992));
#26810=CARTESIAN_POINT('Ctrl Pts',(161.979572858471,-10.5046199403779,-12.3466361338107));
#26811=CARTESIAN_POINT('Ctrl Pts',(162.097266684954,-3.41047972870878,-15.8478734198804));
#26812=CARTESIAN_POINT('Ctrl Pts',(162.214960511437,4.49590375656297,-15.5747652734798));
#26813=CARTESIAN_POINT('Ctrl Pts',(162.33265433792,11.3315382928711,-11.5923554047623));
#26814=CARTESIAN_POINT('Ctrl Pts',(162.450348164404,15.4684423013133,-4.84909854322174));
#26815=CARTESIAN_POINT('Ctrl Pts',(162.568041990887,15.9213665733349,3.04902449198908));
#26816=CARTESIAN_POINT('Ctrl Pts',(162.68573581737,12.5824422093376,10.2209887954907));
#26817=CARTESIAN_POINT('Ctrl Pts',(162.803429643853,6.24687078672089,14.9587121533836));
#26818=CARTESIAN_POINT('Ctrl Pts',(162.921123470336,-1.57646165108159,16.1338536185746));
#26819=CARTESIAN_POINT('Ctrl Pts',(163.038817296819,-9.02434239708718,13.466540319226));
#26820=CARTESIAN_POINT('Ctrl Pts',(163.156066274741,-14.3029494091455,7.61422624586815));
#26821=CARTESIAN_POINT('Ctrl Pts',(163.234083977168,-15.5669420417053,2.52829871263177));
#26822=CARTESIAN_POINT('Ctrl Pts',(163.272870404101,-15.5672257591788,-2.93598225131189E-5));
#26823=CARTESIAN_POINT('Origin',(147.227129595899,0.,0.));
#26824=CARTESIAN_POINT('',(159.977129595899,-15.5659766626728,-0.000379993813608694));
#26825=CARTESIAN_POINT('',(160.272870404101,-15.564687658505,2.74468699046349E-6));
#26826=CARTESIAN_POINT('',(147.227129595899,-15.56595,-7.64522432085395E-13));
#26827=CARTESIAN_POINT('Ctrl Pts',(159.977129595899,-15.5659766626728,-0.000379993813609536));
#26828=CARTESIAN_POINT('Ctrl Pts',(159.986078147623,-15.5665555132718,-0.583834849331341));
#26829=CARTESIAN_POINT('Ctrl Pts',(160.034257974841,-15.3932425959096,-3.72486762104057));
#26830=CARTESIAN_POINT('Ctrl Pts',(160.121669077554,-13.3292169161666,-9.22596553264098));
#26831=CARTESIAN_POINT('Ctrl Pts',(160.239362904037,-7.37563000308724,-14.4355999413));
#26832=CARTESIAN_POINT('Ctrl Pts',(160.357056730521,0.334544350851575,-16.2072373859648));
#26833=CARTESIAN_POINT('Ctrl Pts',(160.474750557004,7.96504328657251,-14.1189429154851));
#26834=CARTESIAN_POINT('Ctrl Pts',(160.592444383487,13.6985795225324,-8.66806683595355));
#26835=CARTESIAN_POINT('Ctrl Pts',(160.71013820997,16.1696483168198,-1.15279526285827));
#26836=CARTESIAN_POINT('Ctrl Pts',(160.827832036453,14.7897374463801,6.6370271865379));
#26837=CARTESIAN_POINT('Ctrl Pts',(160.945525862937,9.88748786846115,12.8461685828396));
#26838=CARTESIAN_POINT('Ctrl Pts',(161.06321968942,2.63042426053809,15.9958535820154));
#26839=CARTESIAN_POINT('Ctrl Pts',(161.180913515903,-5.25310382814925,15.3359500448582));
#26840=CARTESIAN_POINT('Ctrl Pts',(161.298607342386,-11.8855474391451,11.0236212598008));
#26841=CARTESIAN_POINT('Ctrl Pts',(161.397346035718,-15.0750246160597,5.20324843830764));
#26842=CARTESIAN_POINT('Ctrl Pts',(161.456853453556,-15.5645776468435,1.32230026759633));
#26843=CARTESIAN_POINT('Ctrl Pts',(161.477129595899,-15.5646934397166,-3.82463327805449E-5));
#26844=CARTESIAN_POINT('Ctrl Pts',(160.272870404101,-15.564687658505,2.74468699018593E-6));
#26845=CARTESIAN_POINT('Ctrl Pts',(160.292533365303,-15.5646796038872,-1.28234762386084));
#26846=CARTESIAN_POINT('Ctrl Pts',(160.351427601999,-15.095142128267,-5.12323198115841));
#26847=CARTESIAN_POINT('Ctrl Pts',(160.449553114189,-11.9701358491835,-10.9317112871024));
#26848=CARTESIAN_POINT('Ctrl Pts',(160.567246940672,-5.37111728571021,-15.2950175879472));
#26849=CARTESIAN_POINT('Ctrl Pts',(160.684940767156,2.50709195889985,-16.0156471558938));
#26850=CARTESIAN_POINT('Ctrl Pts',(160.802634593639,9.78820966743234,-12.9219741300954));
#26851=CARTESIAN_POINT('Ctrl Pts',(160.920328420122,14.7381575419149,-6.75079078198745));
#26852=CARTESIAN_POINT('Ctrl Pts',(161.038022246605,16.1780510307112,1.02816767123628));
#26853=CARTESIAN_POINT('Ctrl Pts',(161.155716073088,13.7649636560103,8.56225668040771));
#26854=CARTESIAN_POINT('Ctrl Pts',(161.273409899572,8.07359872781038,14.0571500488103));
#26855=CARTESIAN_POINT('Ctrl Pts',(161.391103726055,0.459417427060223,16.2041784592796));
#26856=CARTESIAN_POINT('Ctrl Pts',(161.508797552538,-7.2641791890122,14.4920034716527));
#26857=CARTESIAN_POINT('Ctrl Pts',(161.626491379021,-13.2577316019136,9.32839839865786));
#26858=CARTESIAN_POINT('Ctrl Pts',(161.714515662875,-15.3788599629686,3.80489090455934));
#26859=CARTESIAN_POINT('Ctrl Pts',(161.763308671235,-15.5664660739587,0.623829958404114));
#26860=CARTESIAN_POINT('Ctrl Pts',(161.772870404101,-15.5658554189301,0.000381071499603106));
#26861=CARTESIAN_POINT('Origin',(147.227129595899,0.,0.));
#26862=CARTESIAN_POINT('',(158.477129595899,-15.5672032398919,6.94315363263075E-5));
#26863=CARTESIAN_POINT('',(158.772870404101,-15.5658368563573,-0.000380915866178277));
#26864=CARTESIAN_POINT('',(147.227129595899,-15.56595,-7.64522432085395E-13));
#26865=CARTESIAN_POINT('Ctrl Pts',(158.477129595899,-15.5672032398919,6.94315363258292E-5));
#26866=CARTESIAN_POINT('Ctrl Pts',(158.51530284169,-15.5665698359374,-2.48829837233368));
#26867=CARTESIAN_POINT('Ctrl Pts',(158.592707362976,-14.3338262659127,-7.5346083212108));
#26868=CARTESIAN_POINT('Ctrl Pts',(158.709343159756,-9.12783936934241,-13.3966044972293));
#26869=CARTESIAN_POINT('Ctrl Pts',(158.827036986239,-1.70073240633521,-16.1212274002243));
#26870=CARTESIAN_POINT('Ctrl Pts',(158.944730812722,6.13142269276078,-15.0064026125651));
#26871=CARTESIAN_POINT('Ctrl Pts',(159.062424639206,12.503312012229,-10.3176379240867));
#26872=CARTESIAN_POINT('Ctrl Pts',(159.180118465689,15.8973999993859,-3.17161423682451));
#26873=CARTESIAN_POINT('Ctrl Pts',(159.297812292172,15.5053472542187,4.7297642788828));
#26874=CARTESIAN_POINT('Ctrl Pts',(159.415506118655,11.4205254518286,11.5046973889728));
#26875=CARTESIAN_POINT('Ctrl Pts',(159.533199945138,4.61577985061722,15.5396602272488));
#26876=CARTESIAN_POINT('Ctrl Pts',(159.650893771622,-3.28826451042518,15.8736819962219));
#26877=CARTESIAN_POINT('Ctrl Pts',(159.768587598105,-10.4091724968367,12.4272117362987));
#26878=CARTESIAN_POINT('Ctrl Pts',(159.877332872864,-14.698090296236,6.5081394447137));
#26879=CARTESIAN_POINT('Ctrl Pts',(159.946846872129,-15.5640177788966,1.97408501093939));
#26880=CARTESIAN_POINT('Ctrl Pts',(159.977129595899,-15.5659766626728,-0.000379993813609536));
#26881=CARTESIAN_POINT('Ctrl Pts',(158.772870404101,-15.5658368563573,-0.000380915866179943));
#26882=CARTESIAN_POINT('Ctrl Pts',(158.782526783875,-15.5664518834751,-0.630003179149869));
#26883=CARTESIAN_POINT('Ctrl Pts',(158.831414439144,-15.376611447023,-3.81724297589167));
#26884=CARTESIAN_POINT('Ctrl Pts',(158.919533369908,-13.2466273275316,-9.34416012052252));
#26885=CARTESIAN_POINT('Ctrl Pts',(159.037227196391,-7.24693772795856,-14.5006330027196));
#26886=CARTESIAN_POINT('Ctrl Pts',(159.154921022874,0.478689831123546,-16.2036205817727));
#26887=CARTESIAN_POINT('Ctrl Pts',(159.272614849357,8.0903121397976,-14.0475376273962));
#26888=CARTESIAN_POINT('Ctrl Pts',(159.390308675841,13.7751375929553,-8.54587901901382));
#26889=CARTESIAN_POINT('Ctrl Pts',(159.508002502324,16.1792624575846,-1.00892529013043));
#26890=CARTESIAN_POINT('Ctrl Pts',(159.625696328807,14.7301179440772,6.76831509801693));
#26891=CARTESIAN_POINT('Ctrl Pts',(159.74339015529,9.77283376357005,12.9336067723623));
#26892=CARTESIAN_POINT('Ctrl Pts',(159.861083981773,2.48804168970207,16.0186176826459));
#26893=CARTESIAN_POINT('Ctrl Pts',(159.978777808256,-5.3893048890199,15.2886185355531));
#26894=CARTESIAN_POINT('Ctrl Pts',(160.09647163474,-11.9831292087549,10.9174666602997));
#26895=CARTESIAN_POINT('Ctrl Pts',(160.194502500021,-15.0982173014888,5.11088082725593));
#26896=CARTESIAN_POINT('Ctrl Pts',(160.253302089808,-15.5646956743521,1.27618056895072));
#26897=CARTESIAN_POINT('Ctrl Pts',(160.272870404101,-15.564687658505,2.74468699018593E-6));
#26898=CARTESIAN_POINT('Origin',(147.227129595899,0.,0.));
#26899=CARTESIAN_POINT('',(156.977129595899,-15.5655685625645,0.000368663249558582));
#26900=CARTESIAN_POINT('',(157.272870404101,-15.5672276545898,2.31237102392076E-5));
#26901=CARTESIAN_POINT('',(147.227129595899,-15.56595,-7.64522432085395E-13));
#26902=CARTESIAN_POINT('Ctrl Pts',(156.977129595899,-15.5655685625645,0.000368663249558365));
#26903=CARTESIAN_POINT('Ctrl Pts',(157.005296260263,-15.5638856278198,-1.83626562325807));
#26904=CARTESIAN_POINT('Ctrl Pts',(157.072694200122,-14.7855673246138,-6.23240172064292));
#26905=CARTESIAN_POINT('Ctrl Pts',(157.179323415475,-10.7359079622712,-12.1460587777823));
#26906=CARTESIAN_POINT('Ctrl Pts',(157.297017241958,-3.70915232759935,-15.780641704898));
#26907=CARTESIAN_POINT('Ctrl Pts',(157.414711068441,4.20097874648159,-15.6568911722382));
#26908=CARTESIAN_POINT('Ctrl Pts',(157.532404894924,11.1106005078261,-11.8042797308094));
#26909=CARTESIAN_POINT('Ctrl Pts',(157.650098721407,15.3741105059335,-5.14034918648998));
#26910=CARTESIAN_POINT('Ctrl Pts',(157.76779254789,15.976106922448,2.74781207694638));
#26911=CARTESIAN_POINT('Ctrl Pts',(157.885486374374,12.7732176868821,9.98155165949782));
#26912=CARTESIAN_POINT('Ctrl Pts',(158.003180200857,6.52824611275682,14.8380748852059));
#26913=CARTESIAN_POINT('Ctrl Pts',(158.12087402734,-1.27149910480069,16.1607473105111));
#26914=CARTESIAN_POINT('Ctrl Pts',(158.238567853823,-8.76842281997508,13.6345599436814));
#26915=CARTESIAN_POINT('Ctrl Pts',(158.356261680306,-14.1770501597529,7.86115210230364));
#26916=CARTESIAN_POINT('Ctrl Pts',(158.435782260998,-15.5501236141346,2.69533522288462));
#26917=CARTESIAN_POINT('Ctrl Pts',(158.476071566196,-15.5672207956481,0.069038338801308));
#26918=CARTESIAN_POINT('Ctrl Pts',(158.477129595899,-15.5672032398919,6.94315363258292E-5));
#26919=CARTESIAN_POINT('Ctrl Pts',(157.272870404101,-15.5672276545898,2.31237102390775E-5));
#26920=CARTESIAN_POINT('Ctrl Pts',(157.311751477943,-15.5670021417586,-2.53447369309111));
#26921=CARTESIAN_POINT('Ctrl Pts',(157.389863827279,-14.2981498398272,-7.6265132345712));
#26922=CARTESIAN_POINT('Ctrl Pts',(157.507207452109,-9.00831934563013,-13.4772640576497));
#26923=CARTESIAN_POINT('Ctrl Pts',(157.624901278593,-1.55727144834802,-16.135717199698));
#26924=CARTESIAN_POINT('Ctrl Pts',(157.742595105076,6.26465777934683,-14.9512717459131));
#26925=CARTESIAN_POINT('Ctrl Pts',(157.860288931559,12.5945898255295,-10.2060164138188));
#26926=CARTESIAN_POINT('Ctrl Pts',(157.977982758042,15.9249817238141,-3.03008597380632));
#26927=CARTESIAN_POINT('Ctrl Pts',(158.095676584526,15.4626639986145,4.86749278154799));
#26928=CARTESIAN_POINT('Ctrl Pts',(158.213370411009,11.3177427031671,11.6058245729193));
#26929=CARTESIAN_POINT('Ctrl Pts',(158.331064237492,4.47737645143262,15.5801015408959));
#26930=CARTESIAN_POINT('Ctrl Pts',(158.448758063975,-3.42932626773513,15.8438058957402));
#26931=CARTESIAN_POINT('Ctrl Pts',(158.566451890458,-10.5192972026361,12.3341335437509));
#26932=CARTESIAN_POINT('Ctrl Pts',(158.674489337167,-14.7278239251552,6.41592101404979));
#26933=CARTESIAN_POINT('Ctrl Pts',(158.743295508381,-15.5639531936083,1.92798284095932));
#26934=CARTESIAN_POINT('Ctrl Pts',(158.772870404101,-15.5658368563573,-0.000380915866179943));
#26935=CARTESIAN_POINT('Origin',(147.227129595899,0.,0.));
#26936=CARTESIAN_POINT('',(155.477129595899,-15.56471582026,-8.37554675685322E-5));
#26937=CARTESIAN_POINT('',(155.772870404101,-15.5657013094872,0.000377124385127214));
#26938=CARTESIAN_POINT('',(147.227129595899,-15.56595,-7.64522432085395E-13));
#26939=CARTESIAN_POINT('Ctrl Pts',(155.477129595899,-15.56471582026,-8.37554675685304E-5));
#26940=CARTESIAN_POINT('Ctrl Pts',(155.495289678836,-15.5649433446237,-1.18441545923554));
#26941=CARTESIAN_POINT('Ctrl Pts',(155.552681037267,-15.1430267377089,-4.92710253995072));
#26942=CARTESIAN_POINT('Ctrl Pts',(155.649303671193,-12.1744422313121,-10.703710569898));
#26943=CARTESIAN_POINT('Ctrl Pts',(155.766997497676,-5.65899978025936,-15.1908586029469));
#26944=CARTESIAN_POINT('Ctrl Pts',(155.884691324159,2.20419573563924,-16.0601365114588));
#26945=CARTESIAN_POINT('Ctrl Pts',(156.002385150643,9.54243778386128,-13.104516196672));
#26946=CARTESIAN_POINT('Ctrl Pts',(156.120078977126,14.6080432763861,-7.02791115787139));
#26947=CARTESIAN_POINT('Ctrl Pts',(156.237772803609,16.1945825272352,0.72246825277614));
#26948=CARTESIAN_POINT('Ctrl Pts',(156.355466630092,13.9242037567905,8.30078389955334));
#26949=CARTESIAN_POINT('Ctrl Pts',(156.473160456575,8.3376226506933,13.9021765253628));
#26950=CARTESIAN_POINT('Ctrl Pts',(156.590854283059,0.765344969699789,16.1926128430546));
#26951=CARTESIAN_POINT('Ctrl Pts',(156.708548109542,-6.9892080370811,14.626600241413));
#26952=CARTESIAN_POINT('Ctrl Pts',(156.826241936025,-13.0792042460899,9.5771018526883));
#26953=CARTESIAN_POINT('Ctrl Pts',(156.915769098144,-15.3422530299605,4.00103142563335));
#26954=CARTESIAN_POINT('Ctrl Pts',(156.966064984769,-15.5662296638674,0.72184721343301));
#26955=CARTESIAN_POINT('Ctrl Pts',(156.977129595899,-15.5655685625645,0.000368663249558365));
#26956=CARTESIAN_POINT('Ctrl Pts',(155.772870404101,-15.5657013094872,0.000377124385127978));
#26957=CARTESIAN_POINT('Ctrl Pts',(155.801744896515,-15.563909886075,-1.88236560251977));
#26958=CARTESIAN_POINT('Ctrl Pts',(155.869850664425,-14.7567776476042,-6.3246530627241));
#26959=CARTESIAN_POINT('Ctrl Pts',(155.977187707828,-10.6274475707617,-12.2410711150283));
#26960=CARTESIAN_POINT('Ctrl Pts',(156.094881534311,-3.56864133200721,-15.8130092947535));
#26961=CARTESIAN_POINT('Ctrl Pts',(156.212575360794,4.34007610648377,-15.6189053170316));
#26962=CARTESIAN_POINT('Ctrl Pts',(156.330269187278,11.215156665436,-11.7049871799245));
#26963=CARTESIAN_POINT('Ctrl Pts',(156.447963013761,15.4192242617626,-5.00339755345713));
#26964=CARTESIAN_POINT('Ctrl Pts',(156.565656840244,15.9510339391494,2.88980625381255));
#26965=CARTESIAN_POINT('Ctrl Pts',(156.683350666727,12.6839293713117,10.0947709045845));
#26966=CARTESIAN_POINT('Ctrl Pts',(156.80104449321,6.39600745972602,14.8955547895202));
#26967=CARTESIAN_POINT('Ctrl Pts',(156.918738319694,-1.41519400502264,16.1487984023771));
#26968=CARTESIAN_POINT('Ctrl Pts',(157.036432146177,-8.88935144579475,13.5560279870475));
#26969=CARTESIAN_POINT('Ctrl Pts',(157.15412597266,-14.246412028328,7.7347403467461));
#26970=CARTESIAN_POINT('Ctrl Pts',(157.232938725301,-15.5616701988428,2.60300355025934));
#26971=CARTESIAN_POINT('Ctrl Pts',(157.272520202448,-15.5672296857829,0.0228513248357287));
#26972=CARTESIAN_POINT('Ctrl Pts',(157.272870404101,-15.5672276545898,2.31237102390775E-5));
#26973=CARTESIAN_POINT('Origin',(147.227129595899,0.,0.));
#26974=CARTESIAN_POINT('',(153.977129595899,-15.56613520909,-0.000373169223084742));
#26975=CARTESIAN_POINT('',(154.272870404101,-15.5646950861503,-4.32770794628334E-5));
#26976=CARTESIAN_POINT('',(147.227129595899,-15.56595,-7.64522432085395E-13));
#26977=CARTESIAN_POINT('Ctrl Pts',(153.977129595899,-15.56613520909,-0.000373169223085931));
#26978=CARTESIAN_POINT('Ctrl Pts',(153.985283097409,-15.5666647118316,-0.531974321578409));
#26979=CARTESIAN_POINT('Ctrl Pts',(154.032667874413,-15.4114159073324,-3.62111245429205));
#26980=CARTESIAN_POINT('Ctrl Pts',(154.119283926912,-13.4207257992801,-9.09233647794895));
#26981=CARTESIAN_POINT('Ctrl Pts',(154.236977753395,-7.51948406913288,-14.3611915571709));
#26982=CARTESIAN_POINT('Ctrl Pts',(154.354671579878,0.172605530559356,-16.2097708478104));
#26983=CARTESIAN_POINT('Ctrl Pts',(154.472365406361,7.82358722393355,-14.1978148514905));
#26984=CARTESIAN_POINT('Ctrl Pts',(154.590059232844,13.6112955353353,-8.80449302671448));
#26985=CARTESIAN_POINT('Ctrl Pts',(154.707753059327,16.1573240470198,-1.31428430991864));
#26986=CARTESIAN_POINT('Ctrl Pts',(154.825446885811,14.8553080544366,6.48893567663383));
#26987=CARTESIAN_POINT('Ctrl Pts',(154.943140712294,10.0153369925782,12.7467442326578));
#26988=CARTESIAN_POINT('Ctrl Pts',(155.060834538777,2.79010322505614,15.968775394539));
#26989=CARTESIAN_POINT('Ctrl Pts',(155.17852836526,-5.09962432561176,15.3876669883817));
#26990=CARTESIAN_POINT('Ctrl Pts',(155.296222191744,-11.7748202308851,11.1418163751715));
#26991=CARTESIAN_POINT('Ctrl Pts',(155.39575593529,-15.0484368117828,5.30699215271008));
#26992=CARTESIAN_POINT('Ctrl Pts',(155.456058403342,-15.5644518231355,1.37409947204133));
#26993=CARTESIAN_POINT('Ctrl Pts',(155.477129595899,-15.56471582026,-8.37554675685304E-5));
#26994=CARTESIAN_POINT('Ctrl Pts',(154.272870404101,-15.5646950861503,-4.32770794628334E-5));
#26995=CARTESIAN_POINT('Ctrl Pts',(154.291738315088,-15.5648170261259,-1.23054153718203));
#26996=CARTESIAN_POINT('Ctrl Pts',(154.34983750157,-15.1207250389303,-5.01947793156282));
#26997=CARTESIAN_POINT('Ctrl Pts',(154.447167963547,-12.0787542064295,-10.8115753122814));
#26998=CARTESIAN_POINT('Ctrl Pts',(154.56486179003,-5.52365760332652,-15.2405928557154));
#26999=CARTESIAN_POINT('Ctrl Pts',(154.682555616513,2.34695883598703,-16.039895515079));
#27000=CARTESIAN_POINT('Ctrl Pts',(154.800249442996,9.65862120442349,-13.0191205671478));
#27001=CARTESIAN_POINT('Ctrl Pts',(154.917943269479,14.6699766571649,-6.8976988040002));
#27002=CARTESIAN_POINT('Ctrl Pts',(155.035637095963,16.1875157521321,0.86648582616573));
#27003=CARTESIAN_POINT('Ctrl Pts',(155.153330922446,13.8498198560533,8.4243073227026));
#27004=CARTESIAN_POINT('Ctrl Pts',(155.271024748929,8.21363696874461,13.9757873358942));
#27005=CARTESIAN_POINT('Ctrl Pts',(155.388718575412,0.621286060936392,16.1987798164848));
#27006=CARTESIAN_POINT('Ctrl Pts',(155.506412401895,-7.11903095842639,14.563854645163));
#27007=CARTESIAN_POINT('Ctrl Pts',(155.624106228379,-13.1638724228295,9.4603872409082));
#27008=CARTESIAN_POINT('Ctrl Pts',(155.712925562447,-15.3597346541413,3.90865167943404));
#27009=CARTESIAN_POINT('Ctrl Pts',(155.762513621021,-15.5663438622087,0.675684511174927));
#27010=CARTESIAN_POINT('Ctrl Pts',(155.772870404101,-15.5657013094872,0.000377124385127978));
#27011=CARTESIAN_POINT('Origin',(147.227129595899,0.,0.));
#27012=CARTESIAN_POINT('',(152.477129595899,-15.5671496799154,0.000119929893292461));
#27013=CARTESIAN_POINT('',(152.772870404101,-15.5659940241253,-0.000379545266269155));
#27014=CARTESIAN_POINT('',(147.227129595899,-15.56595,-7.64522432085395E-13));
#27015=CARTESIAN_POINT('Ctrl Pts',(152.477129595899,-15.5671496799154,0.000119929893292372));
#27016=CARTESIAN_POINT('Ctrl Pts',(152.514507791476,-15.566130228717,-2.43644601235259));
#27017=CARTESIAN_POINT('Ctrl Pts',(152.591117262548,-14.3733013902904,-7.43133785604296));
#27018=CARTESIAN_POINT('Ctrl Pts',(152.706958009113,-9.26122566274478,-13.3047421182903));
#27019=CARTESIAN_POINT('Ctrl Pts',(152.824651835596,-1.8617103463467,-16.1034312552471));
#27020=CARTESIAN_POINT('Ctrl Pts',(152.94234566208,5.98119177380371,-15.0669110494933));
#27021=CARTESIAN_POINT('Ctrl Pts',(153.060039488563,12.3996072607107,-10.44204019278));
#27022=CARTESIAN_POINT('Ctrl Pts',(153.177733315046,15.86491984296,-3.3302825682171));
#27023=CARTESIAN_POINT('Ctrl Pts',(153.295427141529,15.551827199527,4.5746184937969));
#27024=CARTESIAN_POINT('Ctrl Pts',(153.413120968012,11.5348957884658,11.3900238260024));
#27025=CARTESIAN_POINT('Ctrl Pts',(153.530814794496,4.77080202447272,15.4927696571985));
#27026=CARTESIAN_POINT('Ctrl Pts',(153.648508620979,-3.12951073579735,15.9057419242933));
#27027=CARTESIAN_POINT('Ctrl Pts',(153.766202447462,-10.2844960796655,12.5305867378607));
#27028=CARTESIAN_POINT('Ctrl Pts',(153.875742772435,-14.6641232704987,6.61169964040524));
#27029=CARTESIAN_POINT('Ctrl Pts',(153.946051821915,-15.5641169637375,2.02587045667698));
#27030=CARTESIAN_POINT('Ctrl Pts',(153.977129595899,-15.56613520909,-0.000373169223085931));
#27031=CARTESIAN_POINT('Ctrl Pts',(152.772870404101,-15.5659940241253,-0.000379545266269155));
#27032=CARTESIAN_POINT('Ctrl Pts',(152.781731733661,-15.5665678851702,-0.578145570173576));
#27033=CARTESIAN_POINT('Ctrl Pts',(152.829824338716,-15.3952625119623,-3.71348484017464));
#27034=CARTESIAN_POINT('Ctrl Pts',(152.917148219265,-13.3393211827226,-9.21135029713916));
#27035=CARTESIAN_POINT('Ctrl Pts',(153.034842045748,-7.39144794457472,-14.4275071025847));
#27036=CARTESIAN_POINT('Ctrl Pts',(153.152535872232,0.316779951246796,-16.2075943426206));
#27037=CARTESIAN_POINT('Ctrl Pts',(153.270229698715,7.94956321608139,-14.1276646543581));
#27038=CARTESIAN_POINT('Ctrl Pts',(153.387923525198,13.689070530273,-8.68307617896328));
#27039=CARTESIAN_POINT('Ctrl Pts',(153.505617351681,16.1683750739281,-1.17051756981636));
#27040=CARTESIAN_POINT('Ctrl Pts',(153.623311178164,14.7970031896607,6.62081267803603));
#27041=CARTESIAN_POINT('Ctrl Pts',(153.741005004647,9.90156218120505,12.8353235364053));
#27042=CARTESIAN_POINT('Ctrl Pts',(153.858698831131,2.64795519030276,15.9929608647873));
#27043=CARTESIAN_POINT('Ctrl Pts',(153.976392657614,-5.23629146518378,15.3416985892734));
#27044=CARTESIAN_POINT('Ctrl Pts',(154.094086484097,-11.8734576922091,11.0366419867544));
#27045=CARTESIAN_POINT('Ctrl Pts',(154.192912399593,-15.0721355684421,5.21463012093322));
#27046=CARTESIAN_POINT('Ctrl Pts',(154.252507039594,-15.5645634813227,1.32798315955527));
#27047=CARTESIAN_POINT('Ctrl Pts',(154.272870404101,-15.5646950861503,-4.32770794628334E-5));
#27048=CARTESIAN_POINT('Origin',(147.227129595899,0.,0.));
#27049=CARTESIAN_POINT('',(150.977129595899,-15.5654260231298,0.00035522955525607));
#27050=CARTESIAN_POINT('',(151.272870404101,-15.5671986622434,7.50751021387497E-5));
#27051=CARTESIAN_POINT('',(147.227129595899,-15.56595,-7.64522432085395E-13));
#27052=CARTESIAN_POINT('Ctrl Pts',(150.977129595899,-15.5654260231298,0.000355229555255854));
#27053=CARTESIAN_POINT('Ctrl Pts',(151.004501210049,-15.563880046197,-1.78448425824574));
#27054=CARTESIAN_POINT('Ctrl Pts',(151.071104099693,-14.8173427789448,-6.12876694614427));
#27055=CARTESIAN_POINT('Ctrl Pts',(151.176938264832,-10.8567200010544,-12.0381919340435));
#27056=CARTESIAN_POINT('Ctrl Pts',(151.294632091315,-3.86662739613892,-15.7427975140589));
#27057=CARTESIAN_POINT('Ctrl Pts',(151.412325917798,4.04434534995169,-15.6980803397344));
#27058=CARTESIAN_POINT('Ctrl Pts',(151.530019744281,10.9921126129483,-11.9146937268782));
#27059=CARTESIAN_POINT('Ctrl Pts',(151.647713570765,15.3219873755107,-5.293691155264));
#27060=CARTESIAN_POINT('Ctrl Pts',(151.765407397248,16.0027622209035,2.58806194553672));
#27061=CARTESIAN_POINT('Ctrl Pts',(151.883101223731,12.8723031774915,9.8534397471975));
#27062=CARTESIAN_POINT('Ctrl Pts',(152.000795050214,6.67616348792316,14.772112390107));
#27063=CARTESIAN_POINT('Ctrl Pts',(152.118488876698,-1.1099779917617,16.1726439575597));
#27064=CARTESIAN_POINT('Ctrl Pts',(152.23618270318,-8.63176600122648,13.7214824003989));
#27065=CARTESIAN_POINT('Ctrl Pts',(152.353876529664,-14.0978039594459,8.00239883654923));
#27066=CARTESIAN_POINT('Ctrl Pts',(152.43419216057,-15.5366625291471,2.79904944997984));
#27067=CARTESIAN_POINT('Ctrl Pts',(152.475276515982,-15.5672002207324,0.120916328577713));
#27068=CARTESIAN_POINT('Ctrl Pts',(152.477129595899,-15.5671496799154,0.000119929893292372));
#27069=CARTESIAN_POINT('Ctrl Pts',(151.272870404101,-15.5671986622434,7.50751021387757E-5));
#27070=CARTESIAN_POINT('Ctrl Pts',(151.310956427728,-15.5665192742014,-2.48260917620549));
#27071=CARTESIAN_POINT('Ctrl Pts',(151.38827372685,-14.3381877797512,-7.52328095819091));
#27072=CARTESIAN_POINT('Ctrl Pts',(151.504822301467,-9.14251744982534,-13.3865917383038));
#27073=CARTESIAN_POINT('Ctrl Pts',(151.62251612795,-1.71840131299559,-16.1193536145945));
#27074=CARTESIAN_POINT('Ctrl Pts',(151.740209954433,6.11497100889316,-15.0131140483778));
#27075=CARTESIAN_POINT('Ctrl Pts',(151.857903780916,12.491995698527,-10.3313361861333));
#27076=CARTESIAN_POINT('Ctrl Pts',(151.9755976074,15.8939141615272,-3.18903692982364));
#27077=CARTESIAN_POINT('Ctrl Pts',(152.093291433883,15.510522082331,4.71276655929273));
#27078=CARTESIAN_POINT('Ctrl Pts',(152.210985260366,11.4331285039078,11.4921728375615));
#27079=CARTESIAN_POINT('Ctrl Pts',(152.328679086849,4.63280957101442,15.5345917033455));
#27080=CARTESIAN_POINT('Ctrl Pts',(152.446372913332,-3.2708639369447,15.8772766247591));
#27081=CARTESIAN_POINT('Ctrl Pts',(152.564066739816,-10.3955452083385,12.4386134168428));
#27082=CARTESIAN_POINT('Ctrl Pts',(152.672899236738,-14.6943933737833,6.51950183076509));
#27083=CARTESIAN_POINT('Ctrl Pts',(152.742500458167,-15.5640272618256,1.97976607728038));
#27084=CARTESIAN_POINT('Ctrl Pts',(152.772870404101,-15.5659940241253,-0.000379545266269155));
#27085=CARTESIAN_POINT('Origin',(110.25,0.,0.));
#27086=CARTESIAN_POINT('',(110.,4.5,-5.51091059616309E-16));
#27087=CARTESIAN_POINT('Origin',(110.,0.,0.));
#27088=CARTESIAN_POINT('',(110.5,4.,4.89858719658941E-16));
#27089=CARTESIAN_POINT('',(110.25,4.25,-5.20474889637625E-16));
#27090=CARTESIAN_POINT('',(110.5,-4.,-4.89858719658941E-16));
#27091=CARTESIAN_POINT('Origin',(110.5,0.,0.));
#27092=CARTESIAN_POINT('Origin',(110.5,0.,0.));
#27093=CARTESIAN_POINT('Origin',(138.,0.,0.));
#27094=CARTESIAN_POINT('',(165.5,4.,-4.89858719658941E-16));
#27095=CARTESIAN_POINT('',(165.5,-4.,-4.89858719658941E-16));
#27096=CARTESIAN_POINT('Origin',(165.5,0.,0.));
#27097=CARTESIAN_POINT('Origin',(165.5,0.,0.));
#27098=CARTESIAN_POINT('',(138.,-4.,-4.89858719658941E-16));
#27099=CARTESIAN_POINT('Origin',(110.,18.,0.));
#27100=CARTESIAN_POINT('',(110.,-18.,-2.20436423846524E-15));
#27101=CARTESIAN_POINT('Origin',(110.,0.,0.));
#27102=CARTESIAN_POINT('Origin',(165.75,0.,0.));
#27103=CARTESIAN_POINT('',(166.,4.5,5.51091059616309E-16));
#27104=CARTESIAN_POINT('',(165.75,4.25,-5.20474889637625E-16));
#27105=CARTESIAN_POINT('Origin',(166.,0.,0.));
#27106=CARTESIAN_POINT('Origin',(166.,4.,0.));
#27107=CARTESIAN_POINT('',(166.,-15.7,-1.92269547466135E-15));
#27108=CARTESIAN_POINT('Origin',(166.,0.,0.));
#27109=CARTESIAN_POINT('Origin',(149.823223304703,0.,-7.76228700170039E-16));
#27110=CARTESIAN_POINT('',(150.,24.5,-3.00038465791102E-15));
#27111=CARTESIAN_POINT('Origin',(150.,0.,0.));
#27112=CARTESIAN_POINT('',(149.646446609407,25.3535533905933,3.10491480068016E-15));
#27113=CARTESIAN_POINT('',(149.823223304703,24.9267766952966,3.05264972929559E-15));
#27114=CARTESIAN_POINT('',(149.646446609407,-25.3535533905933,-3.10491480068016E-15));
#27115=CARTESIAN_POINT('Origin',(149.646446609407,0.,-1.55245740034008E-15));
#27116=CARTESIAN_POINT('Origin',(149.646446609407,0.,-1.55245740034008E-15));
#27117=CARTESIAN_POINT('Origin',(149.5,0.,0.));
#27118=CARTESIAN_POINT('',(149.,-26.,0.));
#27119=CARTESIAN_POINT('',(149.5,-25.5,-3.12284933782575E-15));
#27120=CARTESIAN_POINT('Origin',(149.,0.,0.));
#27121=CARTESIAN_POINT('Origin',(150.,16.5,0.));
#27122=CARTESIAN_POINT('',(150.,9.03673727728063,-12.6742328676692));
#27123=CARTESIAN_POINT('Ctrl Pts',(150.,7.06578282810886,14.8277078846935));
#27124=CARTESIAN_POINT('Ctrl Pts',(150.,7.3876419804473,14.6646824144564));
#27125=CARTESIAN_POINT('Ctrl Pts',(150.,7.70374682458374,14.491245032939));
#27126=CARTESIAN_POINT('Ctrl Pts',(150.,8.01354498609211,14.3075878423168));
#27127=CARTESIAN_POINT('Ctrl Pts',(150.,8.20003860763413,14.1970291016367));
#27128=CARTESIAN_POINT('Ctrl Pts',(150.,8.38424640275821,14.0827659317836));
#27129=CARTESIAN_POINT('Ctrl Pts',(150.,8.5660435295279,13.9648322169156));
#27130=CARTESIAN_POINT('Ctrl Pts',(150.,8.86854267759597,13.7685978269121));
#27131=CARTESIAN_POINT('Ctrl Pts',(150.,9.16436931521678,13.562202911389));
#27132=CARTESIAN_POINT('Ctrl Pts',(150.,9.4531259487604,13.3461003396371));
#27133=CARTESIAN_POINT('Ctrl Pts',(150.,9.68471359963282,13.1727824617919));
#27134=CARTESIAN_POINT('Ctrl Pts',(150.,9.91175309910759,12.9932193970716));
#27135=CARTESIAN_POINT('Ctrl Pts',(150.,10.1340225547111,12.8076273523271));
#27136=CARTESIAN_POINT('Ctrl Pts',(150.,10.2312654415376,12.7264308327514));
#27137=CARTESIAN_POINT('Ctrl Pts',(150.,10.3275951052629,12.6440801438521));
#27138=CARTESIAN_POINT('Ctrl Pts',(150.,10.4229919550846,12.5605925759226));
#27139=CARTESIAN_POINT('Ctrl Pts',(150.,10.4640372264647,12.5246713700449));
#27140=CARTESIAN_POINT('Ctrl Pts',(150.,10.5049098053371,12.4885396969055));
#27141=CARTESIAN_POINT('Ctrl Pts',(150.,10.5456080940746,12.4521989078195));
#27142=CARTESIAN_POINT('Ctrl Pts',(150.,10.5768828741308,12.4242726676509));
#27143=CARTESIAN_POINT('Ctrl Pts',(150.,10.6080543978282,12.3962231908927));
#27144=CARTESIAN_POINT('Ctrl Pts',(150.,10.6391119118545,12.3680603239059));
#27145=CARTESIAN_POINT('Ctrl Pts',(150.,10.9051224416353,12.1268427183698));
#27146=CARTESIAN_POINT('Ctrl Pts',(150.,11.1629640541356,11.8771392131954));
#27147=CARTESIAN_POINT('Ctrl Pts',(150.,11.4122648034249,11.6194163080923));
#27148=CARTESIAN_POINT('Ctrl Pts',(150.,11.663316550501,11.3598832510432));
#27149=CARTESIAN_POINT('Ctrl Pts',(150.,11.9057074706405,11.0922173370697));
#27150=CARTESIAN_POINT('Ctrl Pts',(150.,12.139020104929,10.8168575422661));
#27151=CARTESIAN_POINT('Ctrl Pts',(150.,12.3696205173147,10.5446987608535));
#27152=CARTESIAN_POINT('Ctrl Pts',(150.,12.5913527847256,10.2650234491502));
#27153=CARTESIAN_POINT('Ctrl Pts',(150.,12.8037719291964,9.97822590843219));
#27154=CARTESIAN_POINT('Ctrl Pts',(150.,12.9118552877259,9.83229724698291));
#27155=CARTESIAN_POINT('Ctrl Pts',(150.,13.0175267866837,9.68452421806683));
#27156=CARTESIAN_POINT('Ctrl Pts',(150.,13.1207231838825,9.53495638439154));
#27157=CARTESIAN_POINT('Ctrl Pts',(150.,13.1753746187829,9.45574725551507));
#27158=CARTESIAN_POINT('Ctrl Pts',(150.,13.2293318270461,9.37603472741769));
#27159=CARTESIAN_POINT('Ctrl Pts',(150.,13.2825850354999,9.29582600723517));
#27160=CARTESIAN_POINT('Ctrl Pts',(150.,13.3133564873096,9.24947877597002));
#27161=CARTESIAN_POINT('Ctrl Pts',(150.,13.3438963544375,9.20296040961011));
#27162=CARTESIAN_POINT('Ctrl Pts',(150.,13.3741837495123,9.15630179064984));
#27163=CARTESIAN_POINT('Ctrl Pts',(150.,13.5688092517606,8.85647550559098));
#27164=CARTESIAN_POINT('Ctrl Pts',(150.,13.7531325481106,8.55068502662042));
#27165=CARTESIAN_POINT('Ctrl Pts',(150.,13.9267868768619,8.23937315101738));
#27166=CARTESIAN_POINT('Ctrl Pts',(150.,13.9442701936976,8.20803063168576));
#27167=CARTESIAN_POINT('Ctrl Pts',(150.,13.9616453336674,8.17663211865198));
#27168=CARTESIAN_POINT('Ctrl Pts',(150.,13.978911899393,8.14517804578991));
#27169=CARTESIAN_POINT('Ctrl Pts',(150.,14.149665119914,7.83412115555321));
#27170=CARTESIAN_POINT('Ctrl Pts',(150.,14.3098038877351,7.5176329213665));
#27171=CARTESIAN_POINT('Ctrl Pts',(150.,14.4592458812746,7.19630664194355));
#27172=CARTESIAN_POINT('Ctrl Pts',(150.,14.6095351561267,6.8731585603258));
#27173=CARTESIAN_POINT('Ctrl Pts',(150.,14.7490061923864,6.5451168640693));
#27174=CARTESIAN_POINT('Ctrl Pts',(150.,14.8775272777826,6.21276242824458));
#27175=CARTESIAN_POINT('Ctrl Pts',(150.,15.0060195745878,5.88048243947166));
#27176=CARTESIAN_POINT('Ctrl Pts',(150.,15.1235669606131,5.54389106936735));
#27177=CARTESIAN_POINT('Ctrl Pts',(150.,15.2299877412795,5.20355481059925));
#27178=CARTESIAN_POINT('Ctrl Pts',(150.,15.3357635135699,4.86528130438908));
#27179=CARTESIAN_POINT('Ctrl Pts',(150.,15.4305472375715,4.52330760271481));
#27180=CARTESIAN_POINT('Ctrl Pts',(150.,15.5141094203472,4.17818464278366));
#27181=CARTESIAN_POINT('Ctrl Pts',(150.,15.5500452320262,4.02976494762718));
#27182=CARTESIAN_POINT('Ctrl Pts',(150.,15.5839050579811,3.88076280523603));
#27183=CARTESIAN_POINT('Ctrl Pts',(150.,15.6156676469,3.73122212516282));
#27184=CARTESIAN_POINT('Ctrl Pts',(150.,15.6317105670279,3.65569083920871));
#27185=CARTESIAN_POINT('Ctrl Pts',(150.,15.6472184227117,3.58002216691571));
#27186=CARTESIAN_POINT('Ctrl Pts',(150.,15.6621882966678,3.50422178644977));
#27187=CARTESIAN_POINT('Ctrl Pts',(150.,15.6710144670918,3.45953022270224));
#27188=CARTESIAN_POINT('Ctrl Pts',(150.,15.6796543727474,3.41478865442006));
#27189=CARTESIAN_POINT('Ctrl Pts',(150.,15.6881022820279,3.37002604753674));
#27190=CARTESIAN_POINT('Ctrl Pts',(150.,15.7539079983008,3.02134386944905));
#27191=CARTESIAN_POINT('Ctrl Pts',(150.,15.8081300769565,2.67108305809694));
#27192=CARTESIAN_POINT('Ctrl Pts',(150.,15.850673220764,2.31981577884298));
#27193=CARTESIAN_POINT('Ctrl Pts',(150.,15.8931832860664,1.96882161989506));
#27194=CARTESIAN_POINT('Ctrl Pts',(150.,15.9240326794299,1.61682198581937));
#27195=CARTESIAN_POINT('Ctrl Pts',(150.,15.9430758712819,1.26437592001532));
#27196=CARTESIAN_POINT('Ctrl Pts',(150.,15.955887932133,1.02725388307379));
#27197=CARTESIAN_POINT('Ctrl Pts',(150.,15.9633549233283,0.789929536529496));
#27198=CARTESIAN_POINT('Ctrl Pts',(150.,15.9654192721832,0.552572077685281));
#27199=CARTESIAN_POINT('Ctrl Pts',(150.,15.9684942852131,0.199009123944068));
#27200=CARTESIAN_POINT('Ctrl Pts',(150.,15.959583998504,-0.154627786657829));
#27201=CARTESIAN_POINT('Ctrl Pts',(150.,15.9388380541415,-0.507759999674467));
#27202=CARTESIAN_POINT('Ctrl Pts',(150.,15.9181162996423,-0.860480458961035));
#27203=CARTESIAN_POINT('Ctrl Pts',(150.,15.8855863159675,-1.21269796963108));
#27204=CARTESIAN_POINT('Ctrl Pts',(150.,15.8413465220212,-1.56382488170133));
#27205=CARTESIAN_POINT('Ctrl Pts',(150.,15.8116151333713,-1.7998000017681));
#27206=CARTESIAN_POINT('Ctrl Pts',(150.,15.7765939397513,-2.03528231493771));
#27207=CARTESIAN_POINT('Ctrl Pts',(150.,15.7363004455236,-2.27008868110735));
#27208=CARTESIAN_POINT('Ctrl Pts',(150.,15.718672041799,-2.37281646630657));
#27209=CARTESIAN_POINT('Ctrl Pts',(150.,15.700034360781,-2.47541481223874));
#27210=CARTESIAN_POINT('Ctrl Pts',(150.,15.6803882863496,-2.577868081932));
#27211=CARTESIAN_POINT('Ctrl Pts',(150.,15.6725708481322,-2.6186356209535));
#27212=CARTESIAN_POINT('Ctrl Pts',(150.,15.6645937418988,-2.65938018708575));
#27213=CARTESIAN_POINT('Ctrl Pts',(150.,15.6564570079706,-2.70010078606003));
#27214=CARTESIAN_POINT('Ctrl Pts',(150.,15.6496235725067,-2.7342989775701));
#27215=CARTESIAN_POINT('Ctrl Pts',(150.,15.6426774366298,-2.76848066450812));
#27216=CARTESIAN_POINT('Ctrl Pts',(150.,15.6356218052556,-2.80263028884055));
#27217=CARTESIAN_POINT('Ctrl Pts',(150.,15.5646458610471,-3.14615756553515));
#27218=CARTESIAN_POINT('Ctrl Pts',(150.,15.4825212883806,-3.4868094060629));
#27219=CARTESIAN_POINT('Ctrl Pts',(150.,15.3894544689962,-3.82403800229257));
#27220=CARTESIAN_POINT('Ctrl Pts',(150.,15.2958691082522,-4.16314553857796));
#27221=CARTESIAN_POINT('Ctrl Pts',(150.,15.1912191037315,-4.49879215189183));
#27222=CARTESIAN_POINT('Ctrl Pts',(150.,15.075662546082,-4.83041256132867));
#27223=CARTESIAN_POINT('Ctrl Pts',(150.,14.9604081100008,-5.1611659522229));
#27224=CARTESIAN_POINT('Ctrl Pts',(150.,14.8343038948605,-5.48791471934051));
#27225=CARTESIAN_POINT('Ctrl Pts',(150.,14.6974578001503,-5.81008135591099));
#27226=CARTESIAN_POINT('Ctrl Pts',(150.,14.5620425815663,-6.12887938667728));
#27227=CARTESIAN_POINT('Ctrl Pts',(150.,14.4161087215575,-6.44319110561363));
#27228=CARTESIAN_POINT('Ctrl Pts',(150.,14.2597158771019,-6.75243283543992));
#27229=CARTESIAN_POINT('Ctrl Pts',(150.,14.2213695562824,-6.82825652560918));
#27230=CARTESIAN_POINT('Ctrl Pts',(150.,14.1823942444334,-6.90377527744399));
#27231=CARTESIAN_POINT('Ctrl Pts',(150.,14.142790426037,-6.97898021017884));
#27232=CARTESIAN_POINT('Ctrl Pts',(150.,13.9929250135453,-7.26356434176228));
#27233=CARTESIAN_POINT('Ctrl Pts',(150.,13.8340617188498,-7.54365669711128));
#27234=CARTESIAN_POINT('Ctrl Pts',(150.,13.6664743986313,-7.81889776725218));
#27235=CARTESIAN_POINT('Ctrl Pts',(150.,13.5931549460357,-7.93931573543883));
#27236=CARTESIAN_POINT('Ctrl Pts',(150.,13.5181653204488,-8.05880480754739));
#27237=CARTESIAN_POINT('Ctrl Pts',(150.,13.4415269527696,-8.1773332441067));
#27238=CARTESIAN_POINT('Ctrl Pts',(150.,13.4114222136612,-8.22389305178011));
#27239=CARTESIAN_POINT('Ctrl Pts',(150.,13.3810630576661,-8.27030461804413));
#27240=CARTESIAN_POINT('Ctrl Pts',(150.,13.3504507482978,-8.31656597356602));
#27241=CARTESIAN_POINT('Ctrl Pts',(150.,13.3224450834883,-8.3588881649692));
#27242=CARTESIAN_POINT('Ctrl Pts',(150.,13.2942238181009,-8.40109005482901));
#27243=CARTESIAN_POINT('Ctrl Pts',(150.,13.2658080686662,-8.44314055564525));
#27244=CARTESIAN_POINT('Ctrl Pts',(150.,13.071711669246,-8.73037038292888));
#27245=CARTESIAN_POINT('Ctrl Pts',(150.,12.8684114271802,-9.01074622663321));
#27246=CARTESIAN_POINT('Ctrl Pts',(150.,12.656361724003,-9.28390086392591));
#27247=CARTESIAN_POINT('Ctrl Pts',(150.,12.4426766270286,-9.55916215542676));
#27248=CARTESIAN_POINT('Ctrl Pts',(150.,12.2201062317378,-9.82709087463049));
#27249=CARTESIAN_POINT('Ctrl Pts',(150.,11.9890703934198,-10.0872836008548));
#27250=CARTESIAN_POINT('Ctrl Pts',(150.,11.7579191485341,-10.3476062980382));
#27251=CARTESIAN_POINT('Ctrl Pts',(150.,11.5182935940267,-10.6001856936534));
#27252=CARTESIAN_POINT('Ctrl Pts',(150.,11.2705750738404,-10.8445837082846));
#27253=CARTESIAN_POINT('Ctrl Pts',(150.,11.0242453255649,-11.0876115665887));
#27254=CARTESIAN_POINT('Ctrl Pts',(150.,10.7699126752476,-11.3225498984125));
#27255=CARTESIAN_POINT('Ctrl Pts',(150.,10.5079196621001,-11.5489283694475));
#27256=CARTESIAN_POINT('Ctrl Pts',(150.,10.2501511146187,-11.7716566359715));
#27257=CARTESIAN_POINT('Ctrl Pts',(150.,9.98496681714273,-11.9860991380323));
#27258=CARTESIAN_POINT('Ctrl Pts',(150.,9.71266793165041,-12.1917647788381));
#27259=CARTESIAN_POINT('Ctrl Pts',(150.,9.4919811642635,-12.3584481104644));
#27260=CARTESIAN_POINT('Ctrl Pts',(150.,9.26662069281188,-12.5193657157872));
#27261=CARTESIAN_POINT('Ctrl Pts',(150.,9.03673727728059,-12.6742328676692));
#27262=CARTESIAN_POINT('',(150.,-9.03673727728022,-12.6742328676695));
#27263=CARTESIAN_POINT('Origin',(150.,0.,0.));
#27264=CARTESIAN_POINT('Ctrl Pts',(150.,-9.03713009573235,-12.6741506013612));
#27265=CARTESIAN_POINT('Ctrl Pts',(150.,-9.32675130828298,-12.4794591630376));
#27266=CARTESIAN_POINT('Ctrl Pts',(150.,-9.60948430272415,-12.2752594880836));
#27267=CARTESIAN_POINT('Ctrl Pts',(150.,-9.88481429489231,-12.0618497574774));
#27268=CARTESIAN_POINT('Ctrl Pts',(150.,-10.0428450895277,-11.9393592541907));
#27269=CARTESIAN_POINT('Ctrl Pts',(150.,-10.1984366956213,-11.8138336902965));
#27270=CARTESIAN_POINT('Ctrl Pts',(150.,-10.3514882980122,-11.685322512026));
#27271=CARTESIAN_POINT('Ctrl Pts',(150.,-10.6171411156183,-11.4622646931721));
#27272=CARTESIAN_POINT('Ctrl Pts',(150.,-10.8751436575605,-11.2302144699766));
#27273=CARTESIAN_POINT('Ctrl Pts',(150.,-11.1251971708097,-10.989681345775));
#27274=CARTESIAN_POINT('Ctrl Pts',(150.,-11.3264658616713,-10.7960756395891));
#27275=CARTESIAN_POINT('Ctrl Pts',(150.,-11.5225841327858,-10.596973184495));
#27276=CARTESIAN_POINT('Ctrl Pts',(150.,-11.7133796840543,-10.3926215396668));
#27277=CARTESIAN_POINT('Ctrl Pts',(150.,-11.7968527377343,-10.3032176950545));
#27278=CARTESIAN_POINT('Ctrl Pts',(150.,-11.8793067872374,-10.212808930071));
#27279=CARTESIAN_POINT('Ctrl Pts',(150.,-11.9607264194818,-10.1214151270844));
#27280=CARTESIAN_POINT('Ctrl Pts',(150.,-11.9958094399868,-10.08203432204));
#27281=CARTESIAN_POINT('Ctrl Pts',(150.,-12.0307003950494,-10.0424706214301));
#27282=CARTESIAN_POINT('Ctrl Pts',(150.,-12.0653980152307,-10.0027255888958));
#27283=CARTESIAN_POINT('Ctrl Pts',(150.,-12.0915722427461,-9.97274383456447));
#27284=CARTESIAN_POINT('Ctrl Pts',(150.,-12.1176335868785,-9.94266214609465));
#27285=CARTESIAN_POINT('Ctrl Pts',(150.,-12.1435764176906,-9.91248733704835));
#27286=CARTESIAN_POINT('Ctrl Pts',(150.,-12.370855862704,-9.64813245985379));
#27287=CARTESIAN_POINT('Ctrl Pts',(150.,-12.5891632401871,-9.37649512848077));
#27288=CARTESIAN_POINT('Ctrl Pts',(150.,-12.798217773339,-9.09810414031864));
#27289=CARTESIAN_POINT('Ctrl Pts',(150.,-13.0086584353209,-8.81786729036698));
#27290=CARTESIAN_POINT('Ctrl Pts',(150.,-13.2097235351087,-8.53078649584846));
#27291=CARTESIAN_POINT('Ctrl Pts',(150.,-13.4010903795913,-8.23736297463736));
#27292=CARTESIAN_POINT('Ctrl Pts',(150.,-13.5919691678086,-7.94468779198147));
#27293=CARTESIAN_POINT('Ctrl Pts',(150.,-13.7731994468326,-7.64570171222069));
#27294=CARTESIAN_POINT('Ctrl Pts',(150.,-13.9444195937118,-7.3408712172528));
#27295=CARTESIAN_POINT('Ctrl Pts',(150.,-14.0293152641616,-7.18972785173465));
#27296=CARTESIAN_POINT('Ctrl Pts',(150.,-14.1117493216321,-7.03714723294329));
#27297=CARTESIAN_POINT('Ctrl Pts',(150.,-14.1916734971045,-6.88318395033817));
#27298=CARTESIAN_POINT('Ctrl Pts',(150.,-14.231107214406,-6.80722014432851));
#27299=CARTESIAN_POINT('Ctrl Pts',(150.,-14.2699298996688,-6.73091973174407));
#27300=CARTESIAN_POINT('Ctrl Pts',(150.,-14.3081354892757,-6.65428915565419));
#27301=CARTESIAN_POINT('Ctrl Pts',(150.,-14.3309894228917,-6.60845004894412));
#27302=CARTESIAN_POINT('Ctrl Pts',(150.,-14.3536246467107,-6.56248835872825));
#27303=CARTESIAN_POINT('Ctrl Pts',(150.,-14.3760267541699,-6.51643268441378));
#27304=CARTESIAN_POINT('Ctrl Pts',(150.,-14.5303274258899,-6.19921157045388));
#27305=CARTESIAN_POINT('Ctrl Pts',(150.,-14.6736828241265,-5.8773171309456));
#27306=CARTESIAN_POINT('Ctrl Pts',(150.,-14.8058059081092,-5.55126966129319));
#27307=CARTESIAN_POINT('Ctrl Pts',(150.,-14.8174163159938,-5.5226180131611));
#27308=CARTESIAN_POINT('Ctrl Pts',(150.,-14.8289399613271,-5.49393427291357));
#27309=CARTESIAN_POINT('Ctrl Pts',(150.,-14.8403766345866,-5.46521878133834));
#27310=CARTESIAN_POINT('Ctrl Pts',(150.,-14.969217594009,-5.14172160686549));
#27311=CARTESIAN_POINT('Ctrl Pts',(150.,-15.087024399383,-4.81419707145875));
#27312=CARTESIAN_POINT('Ctrl Pts',(150.,-15.1938238425128,-4.48324472088699));
#27313=CARTESIAN_POINT('Ctrl Pts',(150.,-15.3015591096403,-4.14939241931651));
#27314=CARTESIAN_POINT('Ctrl Pts',(150.,-15.3980934196097,-3.81205143901055));
#27315=CARTESIAN_POINT('Ctrl Pts',(150.,-15.4834062862694,-3.47181341026954));
#27316=CARTESIAN_POINT('Ctrl Pts',(150.,-15.5690125587188,-3.13040524375862));
#27317=CARTESIAN_POINT('Ctrl Pts',(150.,-15.6433201934172,-2.78607950118257));
#27318=CARTESIAN_POINT('Ctrl Pts',(150.,-15.706258362334,-2.43941835600141));
#27319=CARTESIAN_POINT('Ctrl Pts',(150.,-15.7690404765126,-2.09361675464159));
#27320=CARTESIAN_POINT('Ctrl Pts',(150.,-15.8205095189187,-1.74549073870081));
#27321=CARTESIAN_POINT('Ctrl Pts',(150.,-15.860543920808,-1.39561128848453));
#27322=CARTESIAN_POINT('Ctrl Pts',(150.,-15.8778029773184,-1.24477628363531));
#27323=CARTESIAN_POINT('Ctrl Pts',(150.,-15.8929362272837,-1.09361536384623));
#27324=CARTESIAN_POINT('Ctrl Pts',(150.,-15.9059309180032,-0.942174294848833));
#27325=CARTESIAN_POINT('Ctrl Pts',(150.,-15.9127116225689,-0.863151471594134));
#27326=CARTESIAN_POINT('Ctrl Pts',(150.,-15.9189100072436,-0.784052370778021));
#27327=CARTESIAN_POINT('Ctrl Pts',(150.,-15.9245240604719,-0.704883513438272));
#27328=CARTESIAN_POINT('Ctrl Pts',(150.,-15.9273357657567,-0.665233106590456));
#27329=CARTESIAN_POINT('Ctrl Pts',(150.,-15.930000944285,-0.625563840008872));
#27330=CARTESIAN_POINT('Ctrl Pts',(150.,-15.9325181502449,-0.58589706136608));
#27331=CARTESIAN_POINT('Ctrl Pts',(150.,-15.9549841971573,-0.231871318522656));
#27332=CARTESIAN_POINT('Ctrl Pts',(150.,-15.9656952733194,0.122328988982216));
#27333=CARTESIAN_POINT('Ctrl Pts',(150.,-15.964663028844,0.476104466719937));
#27334=CARTESIAN_POINT('Ctrl Pts',(150.,-15.963626438801,0.831369276938752));
#27335=CARTESIAN_POINT('Ctrl Pts',(150.,-15.9507475567728,1.18620625026855));
#27336=CARTESIAN_POINT('Ctrl Pts',(150.,-15.9259875244419,1.54002188838368));
#27337=CARTESIAN_POINT('Ctrl Pts',(150.,-15.9096853081207,1.77297712015682));
#27338=CARTESIAN_POINT('Ctrl Pts',(150.,-15.8882315518575,2.0054898613174));
#27339=CARTESIAN_POINT('Ctrl Pts',(150.,-15.8616028955927,2.23739204259502));
#27340=CARTESIAN_POINT('Ctrl Pts',(150.,-15.8212798853536,2.58855486272253));
#27341=CARTESIAN_POINT('Ctrl Pts',(150.,-15.7690932560903,2.93831808304219));
#27342=CARTESIAN_POINT('Ctrl Pts',(150.,-15.7052969768754,3.28614647273987));
#27343=CARTESIAN_POINT('Ctrl Pts',(150.,-15.6413364804764,3.63487020303523));
#27344=CARTESIAN_POINT('Ctrl Pts',(150.,-15.5657063273605,3.98164968446553));
#27345=CARTESIAN_POINT('Ctrl Pts',(150.,-15.4786108162115,4.32593597572798));
#27346=CARTESIAN_POINT('Ctrl Pts',(150.,-15.4190869863304,4.56123212774712));
#27347=CARTESIAN_POINT('Ctrl Pts',(150.,-15.3542068592886,4.79536356426335));
#27348=CARTESIAN_POINT('Ctrl Pts',(150.,-15.2840224182957,5.02815045121079));
#27349=CARTESIAN_POINT('Ctrl Pts',(150.,-15.2533167253613,5.1299947142503));
#27350=CARTESIAN_POINT('Ctrl Pts',(150.,-15.2215956180984,5.23158156413266));
#27351=CARTESIAN_POINT('Ctrl Pts',(150.,-15.188862825923,5.33289564289095));
#27352=CARTESIAN_POINT('Ctrl Pts',(150.,-15.1755305235451,5.37416159801956));
#27353=CARTESIAN_POINT('Ctrl Pts',(150.,-15.1620303791686,5.41538229834444));
#27354=CARTESIAN_POINT('Ctrl Pts',(150.,-15.1483626271037,5.45655669628066));
#27355=CARTESIAN_POINT('Ctrl Pts',(150.,-15.1375744047441,5.48905644886255));
#27356=CARTESIAN_POINT('Ctrl Pts',(150.,-15.1266818175398,5.52152708261994));
#27357=CARTESIAN_POINT('Ctrl Pts',(150.,-15.1156895277528,5.55395494244973));
#27358=CARTESIAN_POINT('Ctrl Pts',(150.,-15.0017362463883,5.89012339386607));
#27359=CARTESIAN_POINT('Ctrl Pts',(150.,-14.8769534065169,6.22205632476711));
#27360=CARTESIAN_POINT('Ctrl Pts',(150.,-14.7416520189261,6.54923687148926));
#27361=CARTESIAN_POINT('Ctrl Pts',(150.,-14.6048919693399,6.87994469784704));
#27362=CARTESIAN_POINT('Ctrl Pts',(150.,-14.4573852372237,7.20579767618766));
#27363=CARTESIAN_POINT('Ctrl Pts',(150.,-14.2994004327061,7.52625523447028));
#27364=CARTESIAN_POINT('Ctrl Pts',(150.,-14.1413143169204,7.84691829328636));
#27365=CARTESIAN_POINT('Ctrl Pts',(150.,-13.9727364884057,8.162179567917));
#27366=CARTESIAN_POINT('Ctrl Pts',(150.,-13.7938862061515,8.47148227089501));
#27367=CARTESIAN_POINT('Ctrl Pts',(150.,-13.6162151688029,8.77874559416266));
#27368=CARTESIAN_POINT('Ctrl Pts',(150.,-13.4284064523002,9.08012918547539));
#27369=CARTESIAN_POINT('Ctrl Pts',(150.,-13.2306291725494,9.37506419100143));
#27370=CARTESIAN_POINT('Ctrl Pts',(150.,-13.1804286520628,9.44992562506406));
#27371=CARTESIAN_POINT('Ctrl Pts',(150.,-13.129585671806,9.52437146170184));
#27372=CARTESIAN_POINT('Ctrl Pts',(150.,-13.0781025512757,9.59839209806963));
#27373=CARTESIAN_POINT('Ctrl Pts',(150.,-12.8868363481183,9.8733879788073));
#27374=CARTESIAN_POINT('Ctrl Pts',(150.,-12.6867371439721,10.1425172733571));
#27375=CARTESIAN_POINT('Ctrl Pts',(150.,-12.4781574315827,10.4054645622175));
#27376=CARTESIAN_POINT('Ctrl Pts',(150.,-12.3869038074123,10.520504001094));
#27377=CARTESIAN_POINT('Ctrl Pts',(150.,-12.2940265755823,10.6343598142344));
#27378=CARTESIAN_POINT('Ctrl Pts',(150.,-12.1995535549077,10.747003852065));
#27379=CARTESIAN_POINT('Ctrl Pts',(150.,-12.1572188161594,10.7974812886818));
#27380=CARTESIAN_POINT('Ctrl Pts',(150.,-12.1145636193238,10.8477153777883));
#27381=CARTESIAN_POINT('Ctrl Pts',(150.,-12.07159040601,10.8977035118573));
#27382=CARTESIAN_POINT('Ctrl Pts',(150.,-12.047631773304,10.9255731369437));
#27383=CARTESIAN_POINT('Ctrl Pts',(150.,-12.0235735549359,10.9533671050331));
#27384=CARTESIAN_POINT('Ctrl Pts',(150.,-11.9994275296361,10.9810720667265));
#27385=CARTESIAN_POINT('Ctrl Pts',(150.,-11.7657438596099,11.2491988928222));
#27386=CARTESIAN_POINT('Ctrl Pts',(150.,-11.5235990501437,11.5092729716365));
#27387=CARTESIAN_POINT('Ctrl Pts',(150.,-11.2735221781638,11.7610044607555));
#27388=CARTESIAN_POINT('Ctrl Pts',(150.,-11.0208038684604,12.0153948644967));
#27389=CARTESIAN_POINT('Ctrl Pts',(150.,-10.7599847006905,12.2612659227395));
#27390=CARTESIAN_POINT('Ctrl Pts',(150.,-10.4915645756216,12.4982917824595));
#27391=CARTESIAN_POINT('Ctrl Pts',(150.,-10.2214665929276,12.7367992585298));
#27392=CARTESIAN_POINT('Ctrl Pts',(150.,-9.94367193934656,12.9663510283537));
#27393=CARTESIAN_POINT('Ctrl Pts',(150.,-9.65864912466268,13.1865819124749));
#27394=CARTESIAN_POINT('Ctrl Pts',(150.,-9.37433281843848,13.4062668929887));
#27395=CARTESIAN_POINT('Ctrl Pts',(150.,-9.08282369807402,13.6166775145209));
#27396=CARTESIAN_POINT('Ctrl Pts',(150.,-8.78455265000496,13.8174125168282));
#27397=CARTESIAN_POINT('Ctrl Pts',(150.,-8.49002264483304,14.0156298149888));
#27398=CARTESIAN_POINT('Ctrl Pts',(150.,-8.1888988077542,14.2044129755868));
#27399=CARTESIAN_POINT('Ctrl Pts',(150.,-7.88156947113482,14.3833329330089));
#27400=CARTESIAN_POINT('Ctrl Pts',(150.,-7.61411854288894,14.5390366130436));
#27401=CARTESIAN_POINT('Ctrl Pts',(150.,-7.34196749469852,14.6872701843133));
#27402=CARTESIAN_POINT('Ctrl Pts',(150.,-7.06535955977555,14.8277213114857));
#27403=CARTESIAN_POINT('Origin',(124.,-2.95337249083895E-16,37.1267766952966));
#27404=CARTESIAN_POINT('',(114.353553390593,-9.86076131526265E-31,37.5535533905933));
#27405=CARTESIAN_POINT('Origin',(124.,-5.9067449816779E-16,37.5535533905933));
#27406=CARTESIAN_POINT('',(114.215409426056,6.00395323027717E-16,37.2200443578465));
#27407=CARTESIAN_POINT('',(114.176776695297,-1.79367239590926E-15,37.1267766952966));
#27408=CARTESIAN_POINT('',(114.458327956987,-2.99274032010616,36.6999999999997));
#27409=CARTESIAN_POINT('Ctrl Pts',(114.458327956987,-2.99274032010619,36.6999999999997));
#27410=CARTESIAN_POINT('Ctrl Pts',(114.404771619819,-2.64468250602247,36.8281053294846));
#27411=CARTESIAN_POINT('Ctrl Pts',(114.355518882547,-2.27707927894242,36.9352309965706));
#27412=CARTESIAN_POINT('Ctrl Pts',(114.24985583958,-1.26419506839176,37.1564542606582));
#27413=CARTESIAN_POINT('Ctrl Pts',(114.215409426056,-0.605353187125128,
37.2200443578465));
#27414=CARTESIAN_POINT('Ctrl Pts',(114.215409426056,2.63677968348475E-15,
37.2200443578465));
#27415=CARTESIAN_POINT('',(114.458327956987,2.99274032010617,36.6999999999997));
#27416=CARTESIAN_POINT('Origin',(124.,0.,36.7));
#27417=CARTESIAN_POINT('Ctrl Pts',(114.215409426056,3.05311331771918E-15,
37.2200443578465));
#27418=CARTESIAN_POINT('Ctrl Pts',(114.215409426056,0.605353187125133,37.2200443578465));
#27419=CARTESIAN_POINT('Ctrl Pts',(114.24985583958,1.26419506839177,37.1564542606582));
#27420=CARTESIAN_POINT('Ctrl Pts',(114.355518882547,2.27707927894242,36.9352309965706));
#27421=CARTESIAN_POINT('Ctrl Pts',(114.404771619819,2.64468250602248,36.8281053294846));
#27422=CARTESIAN_POINT('Ctrl Pts',(114.458327956987,2.99274032010619,36.6999999999997));
#27423=CARTESIAN_POINT('Origin',(124.,0.,37.6));
#27424=CARTESIAN_POINT('',(114.446446609407,-2.33994571605468E-15,37.6464466094067));
#27425=CARTESIAN_POINT('Origin',(124.,-5.8498642901367E-16,37.6464466094067));
#27426=CARTESIAN_POINT('',(114.4,-1.17566092718146E-15,37.6));
#27427=CARTESIAN_POINT('Origin',(124.,-2.92493214506835E-16,37.8232233047034));
#27428=CARTESIAN_POINT('',(115.3,1.0654427152582E-15,38.));
#27429=CARTESIAN_POINT('',(114.873223304703,5.32721357629098E-16,37.8232233047034));
#27430=CARTESIAN_POINT('Origin',(124.,0.,38.));
#27431=CARTESIAN_POINT('Origin',(124.,0.,38.));
#27432=CARTESIAN_POINT('',(119.59,-5.40069238423981E-16,38.));
#27433=CARTESIAN_POINT('Origin',(124.,0.,38.));
#27434=CARTESIAN_POINT('Origin',(165.275,2.00740175623163E-15,0.));
#27435=CARTESIAN_POINT('Ctrl Pts',(165.275,15.2541446685788,3.10078767190756));
#27436=CARTESIAN_POINT('Ctrl Pts',(165.275,15.1940847495464,3.44455795624862));
#27437=CARTESIAN_POINT('Ctrl Pts',(165.275,15.1225369332471,3.78590288866285));
#27438=CARTESIAN_POINT('Ctrl Pts',(165.275,15.039564239907,4.12423090934285));
#27439=CARTESIAN_POINT('Ctrl Pts',(165.275,14.9919405116494,4.31842060079662));
#27440=CARTESIAN_POINT('Ctrl Pts',(165.275,14.9405520100828,4.51161645307205));
#27441=CARTESIAN_POINT('Ctrl Pts',(165.275,14.8854029013542,4.7037062553512));
#27442=CARTESIAN_POINT('Ctrl Pts',(165.275,14.7896801790758,5.03711796806907));
#27443=CARTESIAN_POINT('Ctrl Pts',(165.275,14.6826308389638,5.3671983468427));
#27444=CARTESIAN_POINT('Ctrl Pts',(165.275,14.5645988217881,5.69346723342415));
#27445=CARTESIAN_POINT('Ctrl Pts',(165.275,14.4695945590912,5.95608186759131));
#27446=CARTESIAN_POINT('Ctrl Pts',(165.275,14.3674739018206,6.21622708849436));
#27447=CARTESIAN_POINT('Ctrl Pts',(165.275,14.2583929258337,6.47364480071921));
#27448=CARTESIAN_POINT('Ctrl Pts',(165.275,14.2106699988393,6.58626504981758));
#27449=CARTESIAN_POINT('Ctrl Pts',(165.275,14.1616145650519,6.69836313022639));
#27450=CARTESIAN_POINT('Ctrl Pts',(165.275,14.1112385188583,6.80991687450263));
#27451=CARTESIAN_POINT('Ctrl Pts',(165.275,14.0895319144857,6.85798442200299));
#27452=CARTESIAN_POINT('Ctrl Pts',(165.275,14.0675801066771,6.90595089933359));
#27453=CARTESIAN_POINT('Ctrl Pts',(165.275,14.045384007563,6.95381451081383));
#27454=CARTESIAN_POINT('Ctrl Pts',(165.275,14.0286403330267,6.98992052785015));
#27455=CARTESIAN_POINT('Ctrl Pts',(165.275,14.0117594503612,7.02596406769214));
#27456=CARTESIAN_POINT('Ctrl Pts',(165.275,13.9947452941642,7.06193721580921));
#27457=CARTESIAN_POINT('Ctrl Pts',(165.275,13.8456879753542,7.37709013584798));
#27458=CARTESIAN_POINT('Ctrl Pts',(165.275,13.6863285350277,7.68700870539031));
#27459=CARTESIAN_POINT('Ctrl Pts',(165.275,13.517035851541,7.99122134069323));
#27460=CARTESIAN_POINT('Ctrl Pts',(165.275,13.3466206778106,8.29745104907986));
#27461=CARTESIAN_POINT('Ctrl Pts',(165.275,13.1661398649656,8.59789943816228));
#27462=CARTESIAN_POINT('Ctrl Pts',(165.275,12.9759200473297,8.89206784933303));
#27463=CARTESIAN_POINT('Ctrl Pts',(165.275,12.7861853604144,9.18548602251582));
#27464=CARTESIAN_POINT('Ctrl Pts',(165.275,12.5867609800285,9.47265671684954));
#27465=CARTESIAN_POINT('Ctrl Pts',(165.275,12.3779259734097,9.75305983794163));
#27466=CARTESIAN_POINT('Ctrl Pts',(165.275,12.2743798164744,9.89209144021882));
#27467=CARTESIAN_POINT('Ctrl Pts',(165.275,12.1685194351303,10.0294588305789));
#27468=CARTESIAN_POINT('Ctrl Pts',(165.275,12.0603750665682,10.1650957095289));
#27469=CARTESIAN_POINT('Ctrl Pts',(165.275,12.0070178110528,10.2320174707235));
#27470=CARTESIAN_POINT('Ctrl Pts',(165.275,11.9531045209606,10.298517936528));
#27471=CARTESIAN_POINT('Ctrl Pts',(165.275,11.8986386160355,10.3645889469169));
#27472=CARTESIAN_POINT('Ctrl Pts',(165.275,11.8660580378524,10.4041115018543));
#27473=CARTESIAN_POINT('Ctrl Pts',(165.275,11.8332765167504,10.4434841146213));
#27474=CARTESIAN_POINT('Ctrl Pts',(165.275,11.8003143199149,10.4826819917362));
#27475=CARTESIAN_POINT('Ctrl Pts',(165.275,11.573278149431,10.7526681202608));
#27476=CARTESIAN_POINT('Ctrl Pts',(165.275,11.3375208402646,11.0145560562498));
#27477=CARTESIAN_POINT('Ctrl Pts',(165.275,11.0934009560395,11.2678719516012));
#27478=CARTESIAN_POINT('Ctrl Pts',(165.275,11.0719487514733,11.2901322620393));
#27479=CARTESIAN_POINT('Ctrl Pts',(165.275,11.0504319397965,11.3123263639781));
#27480=CARTESIAN_POINT('Ctrl Pts',(165.275,11.0288507471137,11.3344539273987));
#27481=CARTESIAN_POINT('Ctrl Pts',(165.275,10.7857257125245,11.5837341549126));
#27482=CARTESIAN_POINT('Ctrl Pts',(165.275,10.5344335063808,11.8245722558248));
#27483=CARTESIAN_POINT('Ctrl Pts',(165.275,10.2755327379732,12.0567488486662));
#27484=CARTESIAN_POINT('Ctrl Pts',(165.275,10.0143633671011,12.2909598749857));
#27485=CARTESIAN_POINT('Ctrl Pts',(165.275,9.74545109022612,12.5163572909644));
#27486=CARTESIAN_POINT('Ctrl Pts',(165.275,9.46932805581463,12.7326817440873));
#27487=CARTESIAN_POINT('Ctrl Pts',(165.275,9.19225538581756,12.9497501749778));
#27488=CARTESIAN_POINT('Ctrl Pts',(165.275,8.90792180753051,13.1576834716916));
#27489=CARTESIAN_POINT('Ctrl Pts',(165.275,8.61683035427967,13.3561801385625));
#27490=CARTESIAN_POINT('Ctrl Pts',(165.275,8.32646065840726,13.5541846355936));
#27491=CARTESIAN_POINT('Ctrl Pts',(165.275,8.02936606305868,13.7427995519239));
#27492=CARTESIAN_POINT('Ctrl Pts',(165.275,7.72601873800543,13.9216815905986));
#27493=CARTESIAN_POINT('Ctrl Pts',(165.275,7.59524399649598,13.9987986456584));
#27494=CARTESIAN_POINT('Ctrl Pts',(165.275,7.46330687339461,14.0741062414512));
#27495=CARTESIAN_POINT('Ctrl Pts',(165.275,7.33024399076646,14.1475741132254));
#27496=CARTESIAN_POINT('Ctrl Pts',(165.275,7.26081100839877,14.1859100739737));
#27497=CARTESIAN_POINT('Ctrl Pts',(165.275,7.19107149212728,14.2237450839022));
#27498=CARTESIAN_POINT('Ctrl Pts',(165.275,7.1210305810407,14.2610746530209));
#27499=CARTESIAN_POINT('Ctrl Pts',(165.275,7.08595176066735,14.279770544171));
#27500=CARTESIAN_POINT('Ctrl Pts',(165.275,7.05079611328678,14.2983402474553));
#27501=CARTESIAN_POINT('Ctrl Pts',(165.275,7.01558255289532,14.3167737591828));
#27502=CARTESIAN_POINT('Ctrl Pts',(165.275,6.70130170909565,14.481292755714));
#27503=CARTESIAN_POINT('Ctrl Pts',(165.275,6.38208021460805,14.6351440545872));
#27504=CARTESIAN_POINT('Ctrl Pts',(165.275,6.05847038177945,14.7780945032695));
#27505=CARTESIAN_POINT('Ctrl Pts',(165.275,5.73349820723714,14.9216467487436));
#27506=CARTESIAN_POINT('Ctrl Pts',(165.275,5.40410018618065,15.0542065060152));
#27507=CARTESIAN_POINT('Ctrl Pts',(165.275,5.07080270097262,15.1754968789651));
#27508=CARTESIAN_POINT('Ctrl Pts',(165.275,4.85135680028192,15.2553554927211));
#27509=CARTESIAN_POINT('Ctrl Pts',(165.275,4.63021981440457,15.330327964054));
#27510=CARTESIAN_POINT('Ctrl Pts',(165.275,4.40753578078987,15.4003245926304));
#27511=CARTESIAN_POINT('Ctrl Pts',(165.275,4.07033172827201,15.5063184819786));
#27512=CARTESIAN_POINT('Ctrl Pts',(165.275,3.72958090391352,15.6009051485531));
#27513=CARTESIAN_POINT('Ctrl Pts',(165.275,3.38587556434815,15.6840989062321));
#27514=CARTESIAN_POINT('Ctrl Pts',(165.275,3.04128550267235,15.7675068105896));
#27515=CARTESIAN_POINT('Ctrl Pts',(165.275,2.69372512292066,15.8394631567612));
#27516=CARTESIAN_POINT('Ctrl Pts',(165.275,2.34377900408581,15.8999313059081));
#27517=CARTESIAN_POINT('Ctrl Pts',(165.275,2.10461474598403,15.9412571536633));
#27518=CARTESIAN_POINT('Ctrl Pts',(165.275,1.86433590591982,15.9772160482172));
#27519=CARTESIAN_POINT('Ctrl Pts',(165.275,1.62312791409366,16.0077823333527));
#27520=CARTESIAN_POINT('Ctrl Pts',(165.275,1.51759941766972,16.0211550830995));
#27521=CARTESIAN_POINT('Ctrl Pts',(165.275,1.41189307363926,16.0334955063498));
#27522=CARTESIAN_POINT('Ctrl Pts',(165.275,1.30602442910336,16.0448007634354));
#27523=CARTESIAN_POINT('Ctrl Pts',(165.275,1.26290336082618,16.0494054768027));
#27524=CARTESIAN_POINT('Ctrl Pts',(165.275,1.2197553673707,16.0538384520432));
#27525=CARTESIAN_POINT('Ctrl Pts',(165.275,1.17658150105774,16.0580994771177));
#27526=CARTESIAN_POINT('Ctrl Pts',(165.275,1.1425035349691,16.0614627864618));
#27527=CARTESIAN_POINT('Ctrl Pts',(165.275,1.10840972125022,16.0647189100905));
#27528=CARTESIAN_POINT('Ctrl Pts',(165.275,1.07431443076556,16.0678665531613));
#27529=CARTESIAN_POINT('Ctrl Pts',(165.275,0.720860279791881,16.100497086391));
#27530=CARTESIAN_POINT('Ctrl Pts',(165.275,0.366870691155206,16.1215115836875));
#27531=CARTESIAN_POINT('Ctrl Pts',(165.275,0.0129443432266137,16.1309839397288));
#27532=CARTESIAN_POINT('Ctrl Pts',(165.275,-0.344797620542512,16.1405584155246));
#27533=CARTESIAN_POINT('Ctrl Pts',(165.275,-0.702475529007602,16.1383406631138));
#27534=CARTESIAN_POINT('Ctrl Pts',(165.275,-1.0594862910395,16.1243561991652));
#27535=CARTESIAN_POINT('Ctrl Pts',(165.275,-1.41672598806189,16.110362767607));
#27536=CARTESIAN_POINT('Ctrl Pts',(165.275,-1.77329827277413,16.0845875753289));
#27537=CARTESIAN_POINT('Ctrl Pts',(165.275,-2.12860531346392,16.0470044590823));
#27538=CARTESIAN_POINT('Ctrl Pts',(165.275,-2.48156963561219,16.0096691472787));
#27539=CARTESIAN_POINT('Ctrl Pts',(165.275,-2.83328591971421,15.9606811019099));
#27540=CARTESIAN_POINT('Ctrl Pts',(165.275,-3.18316570596867,15.899963443923));
#27541=CARTESIAN_POINT('Ctrl Pts',(165.275,-3.27197342713428,15.8845518738576));
#27542=CARTESIAN_POINT('Ctrl Pts',(165.275,-3.36066279296193,15.8683843486503));
#27543=CARTESIAN_POINT('Ctrl Pts',(165.275,-3.44922408738302,15.8514590814298));
#27544=CARTESIAN_POINT('Ctrl Pts',(165.275,-3.77824029779051,15.7885796111442));
#27545=CARTESIAN_POINT('Ctrl Pts',(165.275,-4.10548981858235,15.7152446356181));
#27546=CARTESIAN_POINT('Ctrl Pts',(165.275,-4.43054112840097,15.6316478807662));
#27547=CARTESIAN_POINT('Ctrl Pts',(165.275,-4.57275107644662,15.5950743005185));
#27548=CARTESIAN_POINT('Ctrl Pts',(165.275,-4.71454010907513,15.5565360566608));
#27549=CARTESIAN_POINT('Ctrl Pts',(165.275,-4.85587119547362,15.5160471135189));
#27550=CARTESIAN_POINT('Ctrl Pts',(165.275,-4.919203717467,15.4979034273181));
#27551=CARTESIAN_POINT('Ctrl Pts',(165.275,-4.98244427245377,15.4793680096898));
#27552=CARTESIAN_POINT('Ctrl Pts',(165.275,-5.0455894852499,15.4604420305817));
#27553=CARTESIAN_POINT('Ctrl Pts',(165.275,-5.08079450446641,15.4498903287394));
#27554=CARTESIAN_POINT('Ctrl Pts',(165.275,-5.11597091270945,15.4392168784065));
#27555=CARTESIAN_POINT('Ctrl Pts',(165.275,-5.15110172385917,15.428427010299));
#27556=CARTESIAN_POINT('Ctrl Pts',(165.275,-5.49109545342158,15.3240033611059));
#27557=CARTESIAN_POINT('Ctrl Pts',(165.275,-5.82717408722056,15.2085747292738));
#27558=CARTESIAN_POINT('Ctrl Pts',(165.275,-6.15885764664904,15.0825065615621));
#27559=CARTESIAN_POINT('Ctrl Pts',(165.275,-6.49404462112913,14.9551067959954));
#27560=CARTESIAN_POINT('Ctrl Pts',(165.275,-6.8247437019426,14.8168413986741));
#27561=CARTESIAN_POINT('Ctrl Pts',(165.275,-7.15045388014768,14.6680345158102));
#27562=CARTESIAN_POINT('Ctrl Pts',(165.275,-7.4782000433185,14.5182974545343));
#27563=CARTESIAN_POINT('Ctrl Pts',(165.275,-7.80089527981772,14.3578865204932));
#27564=CARTESIAN_POINT('Ctrl Pts',(165.275,-8.11801542201978,14.1870811873578));
#27565=CARTESIAN_POINT('Ctrl Pts',(165.275,-8.43434950295579,14.0166992377875));
#27566=CARTESIAN_POINT('Ctrl Pts',(165.275,-8.74513661663318,13.8359741036879));
#27567=CARTESIAN_POINT('Ctrl Pts',(165.275,-9.0498349367311,13.6451362127275));
#27568=CARTESIAN_POINT('Ctrl Pts',(165.275,-9.35071161395233,13.4566918835904));
#27569=CARTESIAN_POINT('Ctrl Pts',(165.275,-9.64565173079618,13.2583865792843));
#27570=CARTESIAN_POINT('Ctrl Pts',(165.275,-9.93410536768225,13.0504005429416));
#27571=CARTESIAN_POINT('Ctrl Pts',(165.275,-10.1851298454741,12.8694023529914));
#27572=CARTESIAN_POINT('Ctrl Pts',(165.275,-10.4312417515381,12.6810720241504));
#27573=CARTESIAN_POINT('Ctrl Pts',(165.275,-10.6720568218315,12.4855047231419));
#27574=CARTESIAN_POINT('',(165.275,-16.4196180283464,-0.4237456136972));
#27575=CARTESIAN_POINT('Origin',(165.275,0.,0.));
#27576=CARTESIAN_POINT('Ctrl Pts',(165.275,-16.4196979759281,-0.423941685646876));
#27577=CARTESIAN_POINT('Ctrl Pts',(165.275,-16.4016787090332,-0.7842830862408));
#27578=CARTESIAN_POINT('Ctrl Pts',(165.275,-16.3718071999858,-1.14360257033157));
#27579=CARTESIAN_POINT('Ctrl Pts',(165.275,-16.3300342719941,-1.50131738370712));
#27580=CARTESIAN_POINT('Ctrl Pts',(165.275,-16.3048876264591,-1.71665607426646));
#27581=CARTESIAN_POINT('Ctrl Pts',(165.275,-16.2754270872509,-1.93141328547431));
#27582=CARTESIAN_POINT('Ctrl Pts',(165.275,-16.2416328313117,-2.14546118660578));
#27583=CARTESIAN_POINT('Ctrl Pts',(165.275,-16.1854012842414,-2.50162362584976));
#27584=CARTESIAN_POINT('Ctrl Pts',(165.275,-16.1171736810049,-2.8558230812008));
#27585=CARTESIAN_POINT('Ctrl Pts',(165.275,-16.0372020629593,-3.20751222574865));
#27586=CARTESIAN_POINT('Ctrl Pts',(165.275,-15.9730634874233,-3.48957280316338));
#27587=CARTESIAN_POINT('Ctrl Pts',(165.275,-15.9013697500682,-3.77001858374566));
#27588=CARTESIAN_POINT('Ctrl Pts',(165.275,-15.8222281138278,-4.04855891945055));
#27589=CARTESIAN_POINT('Ctrl Pts',(165.275,-15.7876036479726,-4.17042031632144));
#27590=CARTESIAN_POINT('Ctrl Pts',(165.275,-15.7515533546878,-4.29191688532063));
#27591=CARTESIAN_POINT('Ctrl Pts',(165.275,-15.7140850611406,-4.4130236967691));
#27592=CARTESIAN_POINT('Ctrl Pts',(165.275,-15.697964022471,-4.46513088942947));
#27593=CARTESIAN_POINT('Ctrl Pts',(165.275,-15.6815804720113,-4.51716592437791));
#27594=CARTESIAN_POINT('Ctrl Pts',(165.275,-15.6649349944356,-4.56912679247947));
#27595=CARTESIAN_POINT('Ctrl Pts',(165.275,-15.6521437038709,-4.60905635045434));
#27596=CARTESIAN_POINT('Ctrl Pts',(165.275,-15.6391978329378,-4.64894170388832));
#27597=CARTESIAN_POINT('Ctrl Pts',(165.275,-15.6261020029682,-4.68876902426644));
#27598=CARTESIAN_POINT('Ctrl Pts',(165.275,-15.5139349861521,-5.02989377351528));
#27599=CARTESIAN_POINT('Ctrl Pts',(165.275,-15.390693116279,-5.36700737179514));
#27600=CARTESIAN_POINT('Ctrl Pts',(165.275,-15.2566512779005,-5.6995802871865));
#27601=CARTESIAN_POINT('Ctrl Pts',(165.275,-15.1216679786648,-6.03448907312229));
#27602=CARTESIAN_POINT('Ctrl Pts',(165.275,-14.9757322691986,-6.36479373098975));
#27603=CARTESIAN_POINT('Ctrl Pts',(165.275,-14.8190753781778,-6.6899343455592));
#27604=CARTESIAN_POINT('Ctrl Pts',(165.275,-14.6642395982279,-7.01129525296781));
#27605=CARTESIAN_POINT('Ctrl Pts',(165.275,-14.4989301264842,-7.32761195534377));
#27606=CARTESIAN_POINT('Ctrl Pts',(165.275,-14.3233261861414,-7.6383175684349));
#27607=CARTESIAN_POINT('Ctrl Pts',(165.275,-14.2339751831176,-7.79641116314956));
#27608=CARTESIAN_POINT('Ctrl Pts',(165.275,-14.1419582748423,-7.95305158643488));
#27609=CARTESIAN_POINT('Ctrl Pts',(165.275,-14.0472950161733,-8.10816090472558));
#27610=CARTESIAN_POINT('Ctrl Pts',(165.275,-13.99716261779,-8.19030472955101));
#27611=CARTESIAN_POINT('Ctrl Pts',(165.275,-13.9462879739077,-8.27201909773014));
#27612=CARTESIAN_POINT('Ctrl Pts',(165.275,-13.8946736934634,-8.3532921496216));
#27613=CARTESIAN_POINT('Ctrl Pts',(165.275,-13.8648492679751,-8.40025438680618));
#27614=CARTESIAN_POINT('Ctrl Pts',(165.275,-13.8347743088155,-8.44707466778208));
#27615=CARTESIAN_POINT('Ctrl Pts',(165.275,-13.8044685328867,-8.4937213499452));
#27616=CARTESIAN_POINT('Ctrl Pts',(165.275,-13.6097249156417,-8.79347093029817));
#27617=CARTESIAN_POINT('Ctrl Pts',(165.275,-13.4053424511432,-9.08623483394262));
#27618=CARTESIAN_POINT('Ctrl Pts',(165.275,-13.1915764793124,-9.37149790563643));
#27619=CARTESIAN_POINT('Ctrl Pts',(165.275,-13.1700547684607,-9.40021786182532));
#27620=CARTESIAN_POINT('Ctrl Pts',(165.275,-13.1484379053149,-9.42886176822469));
#27621=CARTESIAN_POINT('Ctrl Pts',(165.275,-13.1267261246103,-9.45742908533937));
#27622=CARTESIAN_POINT('Ctrl Pts',(165.275,-12.9120131061372,-9.73993815130696));
#27623=CARTESIAN_POINT('Ctrl Pts',(165.275,-12.6880210207321,-10.0149595594262));
#27624=CARTESIAN_POINT('Ctrl Pts',(165.275,-12.4552583907319,-10.2821767885852));
#27625=CARTESIAN_POINT('Ctrl Pts',(165.275,-12.2211760823525,-10.55090904101));
#27626=CARTESIAN_POINT('Ctrl Pts',(165.275,-11.9782230602433,-10.8117487534477));
#27627=CARTESIAN_POINT('Ctrl Pts',(165.275,-11.7268764081748,-11.0643393372962));
#27628=CARTESIAN_POINT('Ctrl Pts',(165.275,-11.4755860591534,-11.31687333945));
#27629=CARTESIAN_POINT('Ctrl Pts',(165.275,-11.2159053710805,-11.5611622650247));
#27630=CARTESIAN_POINT('Ctrl Pts',(165.275,-10.9482779591041,-11.7968097141648));
#27631=CARTESIAN_POINT('Ctrl Pts',(165.275,-10.6822726193024,-12.0310289195855));
#27632=CARTESIAN_POINT('Ctrl Pts',(165.275,-10.4084161143014,-12.256711394371));
#27633=CARTESIAN_POINT('Ctrl Pts',(165.275,-10.1271184072732,-12.4734233996839));
#27634=CARTESIAN_POINT('Ctrl Pts',(165.275,-10.006146678876,-12.5666201275353));
#27635=CARTESIAN_POINT('Ctrl Pts',(165.275,-9.88379847902285,-12.658157250573));
#27636=CARTESIAN_POINT('Ctrl Pts',(165.275,-9.76010527741534,-12.7479974951101));
#27637=CARTESIAN_POINT('Ctrl Pts',(165.275,-9.69762926093608,-12.7933747715105));
#27638=CARTESIAN_POINT('Ctrl Pts',(165.275,-9.63481010553126,-12.8383191222954));
#27639=CARTESIAN_POINT('Ctrl Pts',(165.275,-9.57165181189903,-12.8828255728729));
#27640=CARTESIAN_POINT('Ctrl Pts',(165.275,-9.53441395349683,-12.909066384796));
#27641=CARTESIAN_POINT('Ctrl Pts',(165.275,-9.49705465291021,-12.9351573739713));
#27642=CARTESIAN_POINT('Ctrl Pts',(165.275,-9.4595980405967,-12.9610815227979));
#27643=CARTESIAN_POINT('Ctrl Pts',(165.275,-9.16782661633503,-13.1630198551436));
#27644=CARTESIAN_POINT('Ctrl Pts',(165.275,-8.86990154943769,-13.355018095262));
#27645=CARTESIAN_POINT('Ctrl Pts',(165.275,-8.56630677828613,-13.5367564639103));
#27646=CARTESIAN_POINT('Ctrl Pts',(165.275,-8.26294806373811,-13.7183535239917));
#27647=CARTESIAN_POINT('Ctrl Pts',(165.275,-7.95392798018689,-13.8897069930093));
#27648=CARTESIAN_POINT('Ctrl Pts',(165.275,-7.6396980471573,-14.0504565393865));
#27649=CARTESIAN_POINT('Ctrl Pts',(165.275,-7.42828741870809,-14.158607161114));
#27650=CARTESIAN_POINT('Ctrl Pts',(165.275,-7.21451793583355,-14.2619571046843));
#27651=CARTESIAN_POINT('Ctrl Pts',(165.275,-6.99852075110882,-14.3603849559975));
#27652=CARTESIAN_POINT('Ctrl Pts',(165.275,-6.6767756444455,-14.5070011239802));
#27653=CARTESIAN_POINT('Ctrl Pts',(165.275,-6.3500881152452,-14.6426982553463));
#27654=CARTESIAN_POINT('Ctrl Pts',(165.275,-6.01904765523771,-14.7673776954759));
#27655=CARTESIAN_POINT('Ctrl Pts',(165.275,-5.68839318247852,-14.8919117616109));
#27656=CARTESIAN_POINT('Ctrl Pts',(165.275,-5.35339533712104,-15.0054539045506));
#27657=CARTESIAN_POINT('Ctrl Pts',(165.275,-5.01463099442199,-15.1078550161438));
#27658=CARTESIAN_POINT('Ctrl Pts',(165.275,-4.78696415456429,-15.176673762794));
#27659=CARTESIAN_POINT('Ctrl Pts',(165.275,-4.55759595885986,-15.2404595893394));
#27660=CARTESIAN_POINT('Ctrl Pts',(165.275,-4.32670083368095,-15.2991539971731));
#27661=CARTESIAN_POINT('Ctrl Pts',(165.275,-4.22568421641518,-15.3248328006003));
#27662=CARTESIAN_POINT('Ctrl Pts',(165.275,-4.1243753377578,-15.3495369356427));
#27663=CARTESIAN_POINT('Ctrl Pts',(165.275,-4.02278884229152,-15.373260849648));
#27664=CARTESIAN_POINT('Ctrl Pts',(165.275,-3.98236618547463,-15.3827009197064));
#27665=CARTESIAN_POINT('Ctrl Pts',(165.275,-3.94189957256296,-15.3919857817139));
#27666=CARTESIAN_POINT('Ctrl Pts',(165.275,-3.90138992826692,-15.4011150681005));
#27667=CARTESIAN_POINT('Ctrl Pts',(165.275,-3.86736893591951,-15.4087820666065));
#27668=CARTESIAN_POINT('Ctrl Pts',(165.275,-3.83331718190531,-15.4163393952635));
#27669=CARTESIAN_POINT('Ctrl Pts',(165.275,-3.79925018272408,-15.4237836538925));
#27670=CARTESIAN_POINT('Ctrl Pts',(165.275,-3.45655389291593,-15.4986690231305));
#27671=CARTESIAN_POINT('Ctrl Pts',(165.275,-3.11194988903074,-15.5622000687083));
#27672=CARTESIAN_POINT('Ctrl Pts',(165.275,-2.76602256136856,-15.6143425165745));
#27673=CARTESIAN_POINT('Ctrl Pts',(165.275,-2.41816781747772,-15.6667754884675));
#27674=CARTESIAN_POINT('Ctrl Pts',(165.275,-2.06897438754626,-15.7076927214654));
#27675=CARTESIAN_POINT('Ctrl Pts',(165.275,-1.71902298233414,-15.7370087185928));
#27676=CARTESIAN_POINT('Ctrl Pts',(165.275,-1.36998651456403,-15.7662480699259));
#27677=CARTESIAN_POINT('Ctrl Pts',(165.275,-1.02019544917748,-15.7839468280107));
#27678=CARTESIAN_POINT('Ctrl Pts',(165.275,-0.670221251270087,-15.7899686712479));
#27679=CARTESIAN_POINT('Ctrl Pts',(165.275,-0.32390640711229,-15.7959275496874));
#27680=CARTESIAN_POINT('Ctrl Pts',(165.275,0.0225883051757998,-15.7904524237367));
#27681=CARTESIAN_POINT('Ctrl Pts',(165.275,0.368705405399811,-15.7733603902667));
#27682=CARTESIAN_POINT('Ctrl Pts',(165.275,0.453570607697479,-15.7691695575191));
#27683=CARTESIAN_POINT('Ctrl Pts',(165.275,0.538413068762913,-15.7642800840483));
#27684=CARTESIAN_POINT('Ctrl Pts',(165.275,0.623224478572632,-15.7586888003296));
#27685=CARTESIAN_POINT('Ctrl Pts',(165.275,0.944160774763383,-15.7375307286545));
#27686=CARTESIAN_POINT('Ctrl Pts',(165.275,1.26465339880877,-15.7063257144656));
#27687=CARTESIAN_POINT('Ctrl Pts',(165.275,1.58426253506222,-15.6651777123449));
#27688=CARTESIAN_POINT('Ctrl Pts',(165.275,1.7240915321731,-15.647175461417));
#27689=CARTESIAN_POINT('Ctrl Pts',(165.275,1.86375126122269,-15.6272696157382));
#27690=CARTESIAN_POINT('Ctrl Pts',(165.275,2.00320401000376,-15.6054668437631));
#27691=CARTESIAN_POINT('Ctrl Pts',(165.275,2.05798321167464,-15.5969023769208));
#27692=CARTESIAN_POINT('Ctrl Pts',(165.275,2.11273046877317,-15.5880451935127));
#27693=CARTESIAN_POINT('Ctrl Pts',(165.275,2.16744346830565,-15.5788956468138));
#27694=CARTESIAN_POINT('Ctrl Pts',(165.275,2.21749764255649,-15.5705251862524));
#27695=CARTESIAN_POINT('Ctrl Pts',(165.275,2.26752960855478,-15.5619088337655));
#27696=CARTESIAN_POINT('Ctrl Pts',(165.275,2.31750237759088,-15.5530532358352));
#27697=CARTESIAN_POINT('Ctrl Pts',(165.275,2.65884602114199,-15.4925642511012));
#27698=CARTESIAN_POINT('Ctrl Pts',(165.275,2.99767177970771,-15.4208793715129));
#27699=CARTESIAN_POINT('Ctrl Pts',(165.275,3.3334593644421,-15.3382643317085));
#27700=CARTESIAN_POINT('Ctrl Pts',(165.275,3.67183663894271,-15.2550121411194));
#27701=CARTESIAN_POINT('Ctrl Pts',(165.275,4.00712925195428,-15.1606604008729));
#27702=CARTESIAN_POINT('Ctrl Pts',(165.275,4.3387978893757,-15.0554285812879));
#27703=CARTESIAN_POINT('Ctrl Pts',(165.275,4.67063218389584,-14.9501442020215));
#27704=CARTESIAN_POINT('Ctrl Pts',(165.275,4.99883943284626,-14.8339686718481));
#27705=CARTESIAN_POINT('Ctrl Pts',(165.275,5.32286432386021,-14.7070721822145));
#27706=CARTESIAN_POINT('Ctrl Pts',(165.275,5.64507264113224,-14.5808871096274));
#27707=CARTESIAN_POINT('Ctrl Pts',(165.275,5.96314588179039,-14.4441007160084));
#27708=CARTESIAN_POINT('Ctrl Pts',(165.275,6.2765150505169,-14.2968346236721));
#27709=CARTESIAN_POINT('Ctrl Pts',(165.275,6.58483133506045,-14.1519431060639));
#27710=CARTESIAN_POINT('Ctrl Pts',(165.275,6.88859445447486,-13.9969068404714));
#27711=CARTESIAN_POINT('Ctrl Pts',(165.275,7.1872332756858,-13.8318012043831));
#27712=CARTESIAN_POINT('Ctrl Pts',(165.275,7.42926750920022,-13.6979900142722));
#27713=CARTESIAN_POINT('Ctrl Pts',(165.275,7.66793545463417,-13.5575640477772));
#27714=CARTESIAN_POINT('Ctrl Pts',(165.275,7.90291568084398,-13.4105452217265));
#27715=CARTESIAN_POINT('Ctrl Pts',(149.504027251253,-6.69583157622459,14.052211174948));
#27716=CARTESIAN_POINT('Ctrl Pts',(149.543258526747,-9.00505367639947,12.9518745757918));
#27717=CARTESIAN_POINT('Ctrl Pts',(149.621721077736,-13.0684824505813,9.59211511216706));
#27718=CARTESIAN_POINT('Ctrl Pts',(149.739414904219,-16.0518724299814,2.26397071243674));
#27719=CARTESIAN_POINT('Ctrl Pts',(149.857108730702,-15.2118889326799,-5.60192652569123));
#27720=CARTESIAN_POINT('Ctrl Pts',(149.974802557185,-10.7492384929991,-12.1343631343868));
#27721=CARTESIAN_POINT('Ctrl Pts',(150.092496383669,-3.72643497720167,-15.7765283006024));
#27722=CARTESIAN_POINT('Ctrl Pts',(150.210190210152,4.18380951624729,-15.6615050736542));
#27723=CARTESIAN_POINT('Ctrl Pts',(150.327884036635,11.0976583641875,-11.8164414573133));
#27724=CARTESIAN_POINT('Ctrl Pts',(150.445577863118,15.3684657582085,-5.15720159382155));
#27725=CARTESIAN_POINT('Ctrl Pts',(150.563271689601,15.9791097813677,2.73030173509255));
#27726=CARTESIAN_POINT('Ctrl Pts',(150.680965516085,12.7841501358716,9.96754432364079));
#27727=CARTESIAN_POINT('Ctrl Pts',(150.798659342568,6.54450585940981,14.8309111095575));
#27728=CARTESIAN_POINT('Ctrl Pts',(150.916353169051,-1.25378517594862,16.1621310075655));
#27729=CARTESIAN_POINT('Ctrl Pts',(151.034046995534,-8.75347314553567,13.6441626527123));
#27730=CARTESIAN_POINT('Ctrl Pts',(151.151740822017,-14.1684253302768,7.87668630506945));
#27731=CARTESIAN_POINT('Ctrl Pts',(151.2694346485,-16.2090110458911,0.233290702127952));
#27732=CARTESIAN_POINT('Ctrl Pts',(151.387128474984,-14.3892424680134,-7.46566577380577));
#27733=CARTESIAN_POINT('Ctrl Pts',(151.504822301467,-9.14251744982534,-13.3865917383038));
#27734=CARTESIAN_POINT('Ctrl Pts',(151.62251612795,-1.71840131299559,-16.1193536145945));
#27735=CARTESIAN_POINT('Ctrl Pts',(151.740209954433,6.11497100889316,-15.0131140483778));
#27736=CARTESIAN_POINT('Ctrl Pts',(151.857903780916,12.491995698527,-10.3313361861333));
#27737=CARTESIAN_POINT('Ctrl Pts',(151.9755976074,15.8939141615272,-3.18903692982364));
#27738=CARTESIAN_POINT('Ctrl Pts',(152.093291433883,15.510522082331,4.71276655929273));
#27739=CARTESIAN_POINT('Ctrl Pts',(152.210985260366,11.4331285039078,11.4921728375615));
#27740=CARTESIAN_POINT('Ctrl Pts',(152.328679086849,4.63280957101442,15.5345917033455));
#27741=CARTESIAN_POINT('Ctrl Pts',(152.446372913332,-3.2708639369447,15.8772766247591));
#27742=CARTESIAN_POINT('Ctrl Pts',(152.564066739816,-10.3955452083385,12.4386134168428));
#27743=CARTESIAN_POINT('Ctrl Pts',(152.681760566299,-15.0444130039594,6.03755755904503));
#27744=CARTESIAN_POINT('Ctrl Pts',(152.799454392782,-16.1102883058211,-1.80140906399063));
#27745=CARTESIAN_POINT('Ctrl Pts',(152.917148219265,-13.3393211827226,-9.21135029713916));
#27746=CARTESIAN_POINT('Ctrl Pts',(153.034842045748,-7.39144794457472,-14.4275071025847));
#27747=CARTESIAN_POINT('Ctrl Pts',(153.152535872232,0.316779951246796,-16.2075943426206));
#27748=CARTESIAN_POINT('Ctrl Pts',(153.270229698715,7.94956321608139,-14.1276646543581));
#27749=CARTESIAN_POINT('Ctrl Pts',(153.387923525198,13.689070530273,-8.68307617896328));
#27750=CARTESIAN_POINT('Ctrl Pts',(153.505617351681,16.1683750739281,-1.17051756981636));
#27751=CARTESIAN_POINT('Ctrl Pts',(153.623311178164,14.7970031896607,6.62081267803603));
#27752=CARTESIAN_POINT('Ctrl Pts',(153.741005004647,9.90156218120505,12.8353235364053));
#27753=CARTESIAN_POINT('Ctrl Pts',(153.858698831131,2.64795519030276,15.9929608647873));
#27754=CARTESIAN_POINT('Ctrl Pts',(153.976392657614,-5.23629146518378,15.3416985892734));
#27755=CARTESIAN_POINT('Ctrl Pts',(154.094086484097,-11.8734576922091,11.0366419867544));
#27756=CARTESIAN_POINT('Ctrl Pts',(154.21178031058,-15.6828293236568,4.1030876565728));
#27757=CARTESIAN_POINT('Ctrl Pts',(154.329474137063,-15.757162590172,-3.80766214616699));
#27758=CARTESIAN_POINT('Ctrl Pts',(154.447167963547,-12.0787542064295,-10.8115753122814));
#27759=CARTESIAN_POINT('Ctrl Pts',(154.56486179003,-5.52365760332652,-15.2405928557154));
#27760=CARTESIAN_POINT('Ctrl Pts',(154.682555616513,2.34695883598703,-16.039895515079));
#27761=CARTESIAN_POINT('Ctrl Pts',(154.800249442996,9.65862120442349,-13.0191205671478));
#27762=CARTESIAN_POINT('Ctrl Pts',(154.917943269479,14.6699766571649,-6.8976988040002));
#27763=CARTESIAN_POINT('Ctrl Pts',(155.035637095963,16.1875157521321,0.86648582616573));
#27764=CARTESIAN_POINT('Ctrl Pts',(155.153330922446,13.8498198560533,8.4243073227026));
#27765=CARTESIAN_POINT('Ctrl Pts',(155.271024748929,8.21363696874461,13.9757873358942));
#27766=CARTESIAN_POINT('Ctrl Pts',(155.388718575412,0.621286060936392,16.1987798164848));
#27767=CARTESIAN_POINT('Ctrl Pts',(155.506412401895,-7.11903095842639,14.563854645163));
#27768=CARTESIAN_POINT('Ctrl Pts',(155.624106228379,-13.1638724228295,9.4603872409082));
#27769=CARTESIAN_POINT('Ctrl Pts',(155.741800054862,-16.0735928248502,2.10382452058001));
#27770=CARTESIAN_POINT('Ctrl Pts',(155.859493881345,-15.1552102344754,-5.75378715815253));
#27771=CARTESIAN_POINT('Ctrl Pts',(155.977187707828,-10.6274475707617,-12.2410711150283));
#27772=CARTESIAN_POINT('Ctrl Pts',(156.094881534311,-3.56864133200721,-15.8130092947535));
#27773=CARTESIAN_POINT('Ctrl Pts',(156.212575360794,4.34007610648377,-15.6189053170316));
#27774=CARTESIAN_POINT('Ctrl Pts',(156.330269187278,11.215156665436,-11.7049871799245));
#27775=CARTESIAN_POINT('Ctrl Pts',(156.447963013761,15.4192242617626,-5.00339755345713));
#27776=CARTESIAN_POINT('Ctrl Pts',(156.565656840244,15.9510339391494,2.88980625381255));
#27777=CARTESIAN_POINT('Ctrl Pts',(156.683350666727,12.6839293713117,10.0947709045845));
#27778=CARTESIAN_POINT('Ctrl Pts',(156.80104449321,6.39600745972602,14.8955547895202));
#27779=CARTESIAN_POINT('Ctrl Pts',(156.918738319694,-1.41519400502264,16.1487984023771));
#27780=CARTESIAN_POINT('Ctrl Pts',(157.036432146177,-8.88935144579475,13.5560279870475));
#27781=CARTESIAN_POINT('Ctrl Pts',(157.15412597266,-14.246412028328,7.7347403467461));
#27782=CARTESIAN_POINT('Ctrl Pts',(157.271819799143,-16.2105328300161,0.071339185875412));
#27783=CARTESIAN_POINT('Ctrl Pts',(157.389513625626,-14.3139368702984,-7.60905218707177));
#27784=CARTESIAN_POINT('Ctrl Pts',(157.507207452109,-9.00831934563013,-13.4772640576497));
#27785=CARTESIAN_POINT('Ctrl Pts',(157.624901278593,-1.55727144834802,-16.135717199698));
#27786=CARTESIAN_POINT('Ctrl Pts',(157.742595105076,6.26465777934683,-14.9512717459131));
#27787=CARTESIAN_POINT('Ctrl Pts',(157.860288931559,12.5945898255295,-10.2060164138188));
#27788=CARTESIAN_POINT('Ctrl Pts',(157.977982758042,15.9249817238141,-3.03008597380632));
#27789=CARTESIAN_POINT('Ctrl Pts',(158.095676584526,15.4626639986145,4.86749278154799));
#27790=CARTESIAN_POINT('Ctrl Pts',(158.213370411009,11.3177427031671,11.6058245729193));
#27791=CARTESIAN_POINT('Ctrl Pts',(158.331064237492,4.47737645143262,15.5801015408959));
#27792=CARTESIAN_POINT('Ctrl Pts',(158.448758063975,-3.42932626773513,15.8438058957402));
#27793=CARTESIAN_POINT('Ctrl Pts',(158.566451890458,-10.5192972026361,12.3341335437509));
#27794=CARTESIAN_POINT('Ctrl Pts',(158.684145716941,-15.1039817626669,5.886951573225));
#27795=CARTESIAN_POINT('Ctrl Pts',(158.801839543424,-16.0914868735976,-1.96227268984356));
#27796=CARTESIAN_POINT('Ctrl Pts',(158.919533369908,-13.2466273275316,-9.34416012052252));
#27797=CARTESIAN_POINT('Ctrl Pts',(159.037227196391,-7.24693772795856,-14.5006330027196));
#27798=CARTESIAN_POINT('Ctrl Pts',(159.154921022874,0.478689831123546,-16.2036205817727));
#27799=CARTESIAN_POINT('Ctrl Pts',(159.272614849357,8.0903121397976,-14.0475376273962));
#27800=CARTESIAN_POINT('Ctrl Pts',(159.390308675841,13.7751375929553,-8.54587901901382));
#27801=CARTESIAN_POINT('Ctrl Pts',(159.508002502324,16.1792624575846,-1.00892529013043));
#27802=CARTESIAN_POINT('Ctrl Pts',(159.625696328807,14.7301179440772,6.76831509801693));
#27803=CARTESIAN_POINT('Ctrl Pts',(159.74339015529,9.77283376357005,12.9336067723623));
#27804=CARTESIAN_POINT('Ctrl Pts',(159.861083981773,2.48804168970207,16.0186176826459));
#27805=CARTESIAN_POINT('Ctrl Pts',(159.978777808256,-5.3893048890199,15.2886185355531));
#27806=CARTESIAN_POINT('Ctrl Pts',(160.09647163474,-11.9831292087549,10.9174666602997));
#27807=CARTESIAN_POINT('Ctrl Pts',(160.214165461223,-15.7230394545078,3.94619997269045));
#27808=CARTESIAN_POINT('Ctrl Pts',(160.331859287706,-15.7183348502254,-3.9648976592919));
#27809=CARTESIAN_POINT('Ctrl Pts',(160.449553114189,-11.9701358491835,-10.9317112871024));
#27810=CARTESIAN_POINT('Ctrl Pts',(160.567246940672,-5.37111728571021,-15.2950175879472));
#27811=CARTESIAN_POINT('Ctrl Pts',(160.684940767156,2.50709195889985,-16.0156471558938));
#27812=CARTESIAN_POINT('Ctrl Pts',(160.802634593639,9.78820966743234,-12.9219741300954));
#27813=CARTESIAN_POINT('Ctrl Pts',(160.920328420122,14.7381575419149,-6.75079078198745));
#27814=CARTESIAN_POINT('Ctrl Pts',(161.038022246605,16.1780510307112,1.02816767123628));
#27815=CARTESIAN_POINT('Ctrl Pts',(161.155716073088,13.7649636560103,8.56225668040771));
#27816=CARTESIAN_POINT('Ctrl Pts',(161.273409899572,8.07359872781038,14.0571500488103));
#27817=CARTESIAN_POINT('Ctrl Pts',(161.391103726055,0.459417427060223,16.2041784592796));
#27818=CARTESIAN_POINT('Ctrl Pts',(161.508797552538,-7.2641791890122,14.4920034716527));
#27819=CARTESIAN_POINT('Ctrl Pts',(161.626491379021,-13.2577316019136,9.32839839865786));
#27820=CARTESIAN_POINT('Ctrl Pts',(161.744185205504,-16.0938093561825,1.94313260467315));
#27821=CARTESIAN_POINT('Ctrl Pts',(161.861879031987,-15.0969693286697,-5.90491159981625));
#27822=CARTESIAN_POINT('Ctrl Pts',(161.979572858471,-10.5046199403779,-12.3466361338107));
#27823=CARTESIAN_POINT('Ctrl Pts',(162.097266684954,-3.41047972870878,-15.8478734198804));
#27824=CARTESIAN_POINT('Ctrl Pts',(162.214960511437,4.49590375656297,-15.5747652734798));
#27825=CARTESIAN_POINT('Ctrl Pts',(162.33265433792,11.3315382928711,-11.5923554047623));
#27826=CARTESIAN_POINT('Ctrl Pts',(162.450348164404,15.4684423013133,-4.84909854322174));
#27827=CARTESIAN_POINT('Ctrl Pts',(162.568041990887,15.9213665733349,3.04902449198908));
#27828=CARTESIAN_POINT('Ctrl Pts',(162.68573581737,12.5824422093376,10.2209887954907));
#27829=CARTESIAN_POINT('Ctrl Pts',(162.803429643853,6.24687078672089,14.9587121533836));
#27830=CARTESIAN_POINT('Ctrl Pts',(162.921123470336,-1.57646165108159,16.1338536185746));
#27831=CARTESIAN_POINT('Ctrl Pts',(163.038817296819,-9.02434239708718,13.466540319226));
#27832=CARTESIAN_POINT('Ctrl Pts',(163.156511123303,-14.3229767115452,7.59202226981592));
#27833=CARTESIAN_POINT('Ctrl Pts',(163.274204949786,-16.2104365088772,-0.0906194242304325));
#27834=CARTESIAN_POINT('Ctrl Pts',(163.391898776269,-14.2372025145188,-7.75167909617249));
#27835=CARTESIAN_POINT('Ctrl Pts',(163.509592602752,-8.87322202528032,-13.5665911166955));
#27836=CARTESIAN_POINT('Ctrl Pts',(163.627286429235,-1.39598620207817,-16.1504701483178));
#27837=CARTESIAN_POINT('Ctrl Pts',(163.744980255718,6.413719352529,-14.8879370857845));
#27838=CARTESIAN_POINT('Ctrl Pts',(163.862674082202,12.6959265445113,-10.0796778296488));
#27839=CARTESIAN_POINT('Ctrl Pts',(163.980367908685,15.9544602156426,-2.87083272081841));
#27840=CARTESIAN_POINT('Ctrl Pts',(164.098061735168,15.4132614171153,5.0217334684266));
#27841=CARTESIAN_POINT('Ctrl Pts',(164.215755561651,11.2012293687092,11.7183171829071));
#27842=CARTESIAN_POINT('Ctrl Pts',(164.333449388134,4.32149195873656,15.6240575808949));
#27843=CARTESIAN_POINT('Ctrl Pts',(164.451143214618,-3.58743715586971,15.8087508847164));
#27844=CARTESIAN_POINT('Ctrl Pts',(164.568837041101,-10.6420179340868,12.2284282526787));
#27845=CARTESIAN_POINT('Ctrl Pts',(164.686530867584,-15.1620044343422,5.73574619313003));
#27846=CARTESIAN_POINT('Ctrl Pts',(164.804224694067,-16.0711581199633,-2.12291628183429));
#27847=CARTESIAN_POINT('Ctrl Pts',(164.92191852055,-13.1524493936104,-9.4760867792538));
#27848=CARTESIAN_POINT('Ctrl Pts',(165.039612347034,-7.10203868245562,-14.5722070548038));
#27849=CARTESIAN_POINT('Ctrl Pts',(165.157306173517,0.641239642833148,-16.1982319284135));
#27850=CARTESIAN_POINT('Ctrl Pts',(165.235768724506,5.69913956220702,-14.7092438620197));
#27851=CARTESIAN_POINT('Ctrl Pts',(165.275,7.90291568084474,-13.410545221726));
#27852=CARTESIAN_POINT('Ctrl Pts',(149.669351500835,-6.81900757074158,14.3107145537939));
#27853=CARTESIAN_POINT('Ctrl Pts',(149.708582776329,-9.17070994024695,13.1901362485313));
#27854=CARTESIAN_POINT('Ctrl Pts',(149.787045327318,-13.3088892326745,9.76857091231863));
#27855=CARTESIAN_POINT('Ctrl Pts',(149.904739153801,-16.3471614210372,2.30561854077401));
#27856=CARTESIAN_POINT('Ctrl Pts',(150.022432980285,-15.491725652949,-5.70497912836769));
#27857=CARTESIAN_POINT('Ctrl Pts',(150.140126806768,-10.946980644456,-12.3575859305239));
#27858=CARTESIAN_POINT('Ctrl Pts',(150.257820633251,-3.79498618388818,-16.0667520825673));
#27859=CARTESIAN_POINT('Ctrl Pts',(150.375514459734,4.26077454921843,-15.9496128973232));
#27860=CARTESIAN_POINT('Ctrl Pts',(150.493208286218,11.301810020372,-12.033815791119));
#27861=CARTESIAN_POINT('Ctrl Pts',(150.610902112701,15.6511828535263,-5.25207307139863));
#27862=CARTESIAN_POINT('Ctrl Pts',(150.728595939184,16.2730602364247,2.78052815248715));
#27863=CARTESIAN_POINT('Ctrl Pts',(150.846289765667,13.0193263629189,10.1509064902335));
#27864=CARTESIAN_POINT('Ctrl Pts',(150.96398359215,6.6648980778637,15.103739391559));
#27865=CARTESIAN_POINT('Ctrl Pts',(151.081677418633,-1.27684971008452,16.4594483067999));
#27866=CARTESIAN_POINT('Ctrl Pts',(151.199371245116,-8.9145013535939,13.8951596028249));
#27867=CARTESIAN_POINT('Ctrl Pts',(151.3170650716,-14.429066575644,8.02158521091566));
#27868=CARTESIAN_POINT('Ctrl Pts',(151.434758898083,-16.5071907466476,0.237582299656825));
#27869=CARTESIAN_POINT('Ctrl Pts',(151.552452724566,-14.6539458481936,-7.60300357807271));
#27870=CARTESIAN_POINT('Ctrl Pts',(151.670146551049,-9.31070248650847,-13.6328504339994));
#27871=CARTESIAN_POINT('Ctrl Pts',(151.787840377532,-1.75001288928721,-16.41588398425));
#27872=CARTESIAN_POINT('Ctrl Pts',(151.905534204016,6.22746153779737,-15.289294121406));
#27873=CARTESIAN_POINT('Ctrl Pts',(152.023228030499,12.7217974753715,-10.5213906394047));
#27874=CARTESIAN_POINT('Ctrl Pts',(152.140921856982,16.1862973646181,-3.24770220401861));
#27875=CARTESIAN_POINT('Ctrl Pts',(152.258615683465,15.7958524346883,4.79946224469923));
#27876=CARTESIAN_POINT('Ctrl Pts',(152.376309509948,11.6434514425716,11.7035819511739));
#27877=CARTESIAN_POINT('Ctrl Pts',(152.494003336432,4.71803437391177,15.8203648385703));
#27878=CARTESIAN_POINT('Ctrl Pts',(152.611697162915,-3.33103449436932,16.1693537650236));
#27879=CARTESIAN_POINT('Ctrl Pts',(152.729390989398,-10.5867808457656,12.6674331774043));
#27880=CARTESIAN_POINT('Ctrl Pts',(152.847084815881,-15.321168850129,6.14862399617431));
#27881=CARTESIAN_POINT('Ctrl Pts',(152.964778642365,-16.4066519107647,-1.83454764438394));
#27882=CARTESIAN_POINT('Ctrl Pts',(153.082472468847,-13.5847102929711,-9.38080157750341));
#27883=CARTESIAN_POINT('Ctrl Pts',(153.200166295331,-7.52742044345396,-14.6929143959928));
#27884=CARTESIAN_POINT('Ctrl Pts',(153.317860121814,0.322607410479242,-16.5057479818145));
#27885=CARTESIAN_POINT('Ctrl Pts',(153.435553948297,8.09580275988852,-14.3875560695159));
#27886=CARTESIAN_POINT('Ctrl Pts',(153.55324777478,13.9408936021924,-8.84280936992474));
#27887=CARTESIAN_POINT('Ctrl Pts',(153.670941601264,16.4658072385194,-1.19205031957574));
#27888=CARTESIAN_POINT('Ctrl Pts',(153.788635427747,15.0692077042171,6.74260863076332));
#27889=CARTESIAN_POINT('Ctrl Pts',(153.90632925423,10.0837105454609,13.0714411453305));
#27890=CARTESIAN_POINT('Ctrl Pts',(154.024023080713,2.69666676709334,16.2871661232927));
#27891=CARTESIAN_POINT('Ctrl Pts',(154.141716907196,-5.33261787385496,15.6239232778429));
#27892=CARTESIAN_POINT('Ctrl Pts',(154.25941073368,-12.0918808922171,11.239671190427));
#27893=CARTESIAN_POINT('Ctrl Pts',(154.377104560163,-15.9713294265628,4.17856773652037));
#27894=CARTESIAN_POINT('Ctrl Pts',(154.494798386646,-16.047030122041,-3.87770760150731));
#27895=CARTESIAN_POINT('Ctrl Pts',(154.612492213129,-12.3009540250728,-11.0104642069953));
#27896=CARTESIAN_POINT('Ctrl Pts',(154.730186039612,-5.62527037702249,-15.52095761111));
#27897=CARTESIAN_POINT('Ctrl Pts',(154.847879866096,2.39013330736106,-16.3349641797441));
#27898=CARTESIAN_POINT('Ctrl Pts',(154.965573692578,9.83630044545192,-13.2586192918901));
#27899=CARTESIAN_POINT('Ctrl Pts',(155.083267519062,14.9398444015544,-7.02458833226706));
#27900=CARTESIAN_POINT('Ctrl Pts',(155.200961345545,16.4853000271441,0.88242563172352));
#27901=CARTESIAN_POINT('Ctrl Pts',(155.318655172028,14.1046000600101,8.5792802220024));
#27902=CARTESIAN_POINT('Ctrl Pts',(155.436348998511,8.36473439267312,14.2328848277681));
#27903=CARTESIAN_POINT('Ctrl Pts',(155.554042824995,0.632715190771028,16.4967713043446));
#27904=CARTESIAN_POINT('Ctrl Pts',(155.671736651478,-7.24999209571292,14.8317701773112));
#27905=CARTESIAN_POINT('Ctrl Pts',(155.789430477961,-13.4060339913992,9.63441978543227));
#27906=CARTESIAN_POINT('Ctrl Pts',(155.907124304444,-16.369281382593,2.14252631208443));
#27907=CARTESIAN_POINT('Ctrl Pts',(156.024818130927,-15.4340042978408,-5.85963337715855));
#27908=CARTESIAN_POINT('Ctrl Pts',(156.142511957411,-10.8229492659289,-12.46625690284));
#27909=CARTESIAN_POINT('Ctrl Pts',(156.260205783894,-3.63428977912547,-16.1039041782365));
#27910=CARTESIAN_POINT('Ctrl Pts',(156.377899610377,4.41991580743947,-15.9062294789062));
#27911=CARTESIAN_POINT('Ctrl Pts',(156.49559343686,11.4214698111898,-11.9203112095514));
#27912=CARTESIAN_POINT('Ctrl Pts',(156.613287263343,15.702875106546,-5.0954396639247));
#27913=CARTESIAN_POINT('Ctrl Pts',(156.730981089826,16.2444679132066,2.94296690387111));
#27914=CARTESIAN_POINT('Ctrl Pts',(156.84867491631,12.9172619450047,10.2804735214198));
#27915=CARTESIAN_POINT('Ctrl Pts',(156.966368742793,6.5136679132218,15.1695722516076));
#27916=CARTESIAN_POINT('Ctrl Pts',(157.084062569276,-1.44122780336697,16.4458704360481));
#27917=CARTESIAN_POINT('Ctrl Pts',(157.201756395759,-9.0528792604481,13.8054036187367));
#27918=CARTESIAN_POINT('Ctrl Pts',(157.319450222242,-14.5084879108993,7.87702802583353));
#27919=CARTESIAN_POINT('Ctrl Pts',(157.437144048726,-16.5087405253944,0.0726515359649123));
#27920=CARTESIAN_POINT('Ctrl Pts',(157.554837875209,-14.5772549345868,-7.74902771659407));
#27921=CARTESIAN_POINT('Ctrl Pts',(157.672531701692,-9.17403568447366,-13.7251907542476));
#27922=CARTESIAN_POINT('Ctrl Pts',(157.790225528175,-1.58591889223899,-16.4325485925865));
#27923=CARTESIAN_POINT('Ctrl Pts',(157.907919354658,6.37990193438496,-15.226314172777));
#27924=CARTESIAN_POINT('Ctrl Pts',(158.025613181142,12.8262789159184,-10.3937654943502));
#27925=CARTESIAN_POINT('Ctrl Pts',(158.143307007625,16.2179364433534,-3.08582719863357));
#27926=CARTESIAN_POINT('Ctrl Pts',(158.261000834108,15.7471139574029,4.95703479845001));
#27927=CARTESIAN_POINT('Ctrl Pts',(158.378694660591,11.5259430136559,11.8193244149755));
#27928=CARTESIAN_POINT('Ctrl Pts',(158.496388487074,4.55974191880648,15.8667118715365));
#27929=CARTESIAN_POINT('Ctrl Pts',(158.614082313558,-3.492411885816,16.1352673110888));
#27930=CARTESIAN_POINT('Ctrl Pts',(158.731776140041,-10.7128093720813,12.5610313007303));
#27931=CARTESIAN_POINT('Ctrl Pts',(158.849469966524,-15.3818334310674,5.99524747440632));
#27932=CARTESIAN_POINT('Ctrl Pts',(158.967163793007,-16.387504608863,-1.99837050492948));
#27933=CARTESIAN_POINT('Ctrl Pts',(159.08485761949,-13.4903112488624,-9.51605456002099));
#27934=CARTESIAN_POINT('Ctrl Pts',(159.202551445973,-7.3802518281838,-14.7673855144731));
#27935=CARTESIAN_POINT('Ctrl Pts',(159.320245272457,0.487495771855852,-16.5017011199725));
#27936=CARTESIAN_POINT('Ctrl Pts',(159.43793909894,8.23914088980841,-14.3059550320265));
#27937=CARTESIAN_POINT('Ctrl Pts',(159.555632925423,14.0285439478352,-8.70308834174033));
#27938=CARTESIAN_POINT('Ctrl Pts',(159.673326751906,16.4768949056349,-1.02748540093825));
#27939=CARTESIAN_POINT('Ctrl Pts',(159.791020578389,15.0010920428818,6.89282449373751));
#27940=CARTESIAN_POINT('Ctrl Pts',(159.908714404872,9.95261404991291,13.1715323920171));
#27941=CARTESIAN_POINT('Ctrl Pts',(160.026408231356,2.53381151022997,16.3132949219679));
#27942=CARTESIAN_POINT('Ctrl Pts',(160.144102057839,-5.4884461206807,15.5698667676016));
#27943=CARTESIAN_POINT('Ctrl Pts',(160.261795884322,-12.2035699174123,11.1183035239783));
#27944=CARTESIAN_POINT('Ctrl Pts',(160.379489710805,-16.0122792598392,4.01879395906327));
#27945=CARTESIAN_POINT('Ctrl Pts',(160.497183537288,-16.007488110024,-4.03783560684653));
#27946=CARTESIAN_POINT('Ctrl Pts',(160.614877363772,-12.1903375330135,-11.1328101938226));
#27947=CARTESIAN_POINT('Ctrl Pts',(160.732571190255,-5.4699239396416,-15.5763835364636));
#27948=CARTESIAN_POINT('Ctrl Pts',(160.850265016738,2.55321222669146,-16.3102697496379));
#27949=CARTESIAN_POINT('Ctrl Pts',(160.967958843221,9.96827280770127,-13.1596857565719));
#27950=CARTESIAN_POINT('Ctrl Pts',(161.085652669704,15.0092795365331,-6.8749778017596));
#27951=CARTESIAN_POINT('Ctrl Pts',(161.203346496188,16.4756611934474,1.04708176338345));
#27952=CARTESIAN_POINT('Ctrl Pts',(161.321040322671,14.0181828519411,8.71976728531359));
#27953=CARTESIAN_POINT('Ctrl Pts',(161.438734149154,8.22212001920016,14.3157442827939));
#27954=CARTESIAN_POINT('Ctrl Pts',(161.556427975637,0.467868834153206,16.5022692601504));
#27955=CARTESIAN_POINT('Ctrl Pts',(161.67412180212,-7.39781046180786,14.7585972352269));
#27956=CARTESIAN_POINT('Ctrl Pts',(161.791815628604,-13.5016197966082,9.50000288675245));
#27957=CARTESIAN_POINT('Ctrl Pts',(161.909509455087,-16.3898698156561,1.97887832024774));
#27958=CARTESIAN_POINT('Ctrl Pts',(162.02720328157,-15.3746919968823,-6.01353789224345));
#27959=CARTESIAN_POINT('Ctrl Pts',(162.144897108053,-10.6978621080534,-12.5737638874599));
#27960=CARTESIAN_POINT('Ctrl Pts',(162.262590934536,-3.47321864733025,-16.1394096610853));
#27961=CARTESIAN_POINT('Ctrl Pts',(162.380284761019,4.57861005079439,-15.861277438562));
#27962=CARTESIAN_POINT('Ctrl Pts',(162.497978587503,11.5399923859502,-11.8056074690535));
#27963=CARTESIAN_POINT('Ctrl Pts',(162.615672413986,15.7529985573068,-4.93830218115272));
#27964=CARTESIAN_POINT('Ctrl Pts',(162.733366240469,16.2142547888485,3.10511410831708));
#27965=CARTESIAN_POINT('Ctrl Pts',(162.851060066952,12.8139078331282,10.4090133067854));
#27966=CARTESIAN_POINT('Ctrl Pts',(162.968753893435,6.36178773363243,15.233891453402));
#27967=CARTESIAN_POINT('Ctrl Pts',(163.086447719919,-1.60546211644266,16.4306507291704));
#27968=CARTESIAN_POINT('Ctrl Pts',(163.204141546402,-9.19035349473336,13.7142697427697));
#27969=CARTESIAN_POINT('Ctrl Pts',(163.321835372885,-14.5864610720469,7.73168451831101));
#27970=CARTESIAN_POINT('Ctrl Pts',(163.439529199368,-16.5086424323394,-0.0922864520782876));
#27971=CARTESIAN_POINT('Ctrl Pts',(163.557223025851,-14.4991089795936,-7.89427837917087));
#27972=CARTESIAN_POINT('Ctrl Pts',(163.674916852335,-9.03645312437413,-13.8161610668922));
#27973=CARTESIAN_POINT('Ctrl Pts',(163.792610678818,-1.42166665518031,-16.4475729352965));
#27974=CARTESIAN_POINT('Ctrl Pts',(163.910304505301,6.5317056326209,-15.1618144131892));
#27975=CARTESIAN_POINT('Ctrl Pts',(164.027998331784,12.929479817265,-10.2651027954568));
#27976=CARTESIAN_POINT('Ctrl Pts',(164.145692158267,16.2479572192145,-2.92364433524647));
#27977=CARTESIAN_POINT('Ctrl Pts',(164.263385984751,15.6968025698744,5.1141128849533));
#27978=CARTESIAN_POINT('Ctrl Pts',(164.381079811234,11.4072863090007,11.9338864302274));
#27979=CARTESIAN_POINT('Ctrl Pts',(164.498773637717,4.40098978716235,15.9114765234129));
#27980=CARTESIAN_POINT('Ctrl Pts',(164.6164674642,-3.65343136949515,16.0995674308211));
#27981=CARTESIAN_POINT('Ctrl Pts',(164.734161290683,-10.8377876645193,12.4533814633825));
#27982=CARTESIAN_POINT('Ctrl Pts',(164.851855117167,-15.4409234832775,5.8412605319531));
#27983=CARTESIAN_POINT('Ctrl Pts',(164.96954894365,-16.3668018890651,-2.16196928388703));
#27984=CARTESIAN_POINT('Ctrl Pts',(165.087242770133,-13.3944008250271,-9.65040813125861));
#27985=CARTESIAN_POINT('Ctrl Pts',(165.204936596616,-7.23268723116105,-14.8402762372271));
#27986=CARTESIAN_POINT('Ctrl Pts',(165.322630423099,0.6530358372013,-16.4962133373671));
#27987=CARTESIAN_POINT('Ctrl Pts',(165.401092974088,5.80398048830776,-14.9798339628417));
#27988=CARTESIAN_POINT('Ctrl Pts',(165.440324249582,8.04829710023833,-13.6572445638311));
#27989=CARTESIAN_POINT('Ctrl Pts',(149.834675750418,-6.94218356525857,14.5692179326398));
#27990=CARTESIAN_POINT('Ctrl Pts',(149.873907025912,-9.33636620409445,13.4283979212707));
#27991=CARTESIAN_POINT('Ctrl Pts',(149.952369576901,-13.5492960147677,9.9450267124702));
#27992=CARTESIAN_POINT('Ctrl Pts',(150.070063403384,-16.642450412093,2.34726636911127));
#27993=CARTESIAN_POINT('Ctrl Pts',(150.187757229867,-15.7715623732181,-5.80803173104413));
#27994=CARTESIAN_POINT('Ctrl Pts',(150.30545105635,-11.1447227959129,-12.5808087266611));
#27995=CARTESIAN_POINT('Ctrl Pts',(150.423144882834,-3.86353739057469,-16.3569758645323));
#27996=CARTESIAN_POINT('Ctrl Pts',(150.540838709317,4.33773958218958,-16.2377207209922));
#27997=CARTESIAN_POINT('Ctrl Pts',(150.6585325358,11.5059616765565,-12.2511901249246));
#27998=CARTESIAN_POINT('Ctrl Pts',(150.776226362283,15.9338999488442,-5.34694454897571));
#27999=CARTESIAN_POINT('Ctrl Pts',(150.893920188766,16.5670106914817,2.83075456988176));
#28000=CARTESIAN_POINT('Ctrl Pts',(151.011614015249,13.2545025899662,10.3342686568263));
#28001=CARTESIAN_POINT('Ctrl Pts',(151.129307841733,6.78529029631758,15.3765676735605));
#28002=CARTESIAN_POINT('Ctrl Pts',(151.247001668216,-1.29991424422042,16.7567656060342));
#28003=CARTESIAN_POINT('Ctrl Pts',(151.364695494699,-9.07552956165211,14.1461565529374));
#28004=CARTESIAN_POINT('Ctrl Pts',(151.482389321182,-14.6897078210113,8.16648411676187));
#28005=CARTESIAN_POINT('Ctrl Pts',(151.600083147665,-16.8053704474042,0.241873897185706));
#28006=CARTESIAN_POINT('Ctrl Pts',(151.717776974149,-14.9186492283738,-7.74034138233968));
#28007=CARTESIAN_POINT('Ctrl Pts',(151.835470800632,-9.47888752319158,-13.8791091296951));
#28008=CARTESIAN_POINT('Ctrl Pts',(151.953164627115,-1.78162446557883,-16.7124143539056));
#28009=CARTESIAN_POINT('Ctrl Pts',(152.070858453598,6.33995206670156,-15.5654741944342));
#28010=CARTESIAN_POINT('Ctrl Pts',(152.188552280081,12.951599252216,-10.7114450926761));
#28011=CARTESIAN_POINT('Ctrl Pts',(152.306246106565,16.478680567709,-3.30636747821358));
#28012=CARTESIAN_POINT('Ctrl Pts',(152.423939933048,16.0811827870456,4.88615793010572));
#28013=CARTESIAN_POINT('Ctrl Pts',(152.541633759531,11.8537743812354,11.9149910647864));
#28014=CARTESIAN_POINT('Ctrl Pts',(152.659327586014,4.80325917680914,16.1061379737952));
#28015=CARTESIAN_POINT('Ctrl Pts',(152.777021412497,-3.39120505179396,16.4614309052881));
#28016=CARTESIAN_POINT('Ctrl Pts',(152.89471523898,-10.7780164831926,12.8962529379659));
#28017=CARTESIAN_POINT('Ctrl Pts',(153.012409065464,-15.5979246962986,6.25969043330361));
#28018=CARTESIAN_POINT('Ctrl Pts',(153.130102891947,-16.7030155157083,-1.86768622477728));
#28019=CARTESIAN_POINT('Ctrl Pts',(153.24779671843,-13.8300994032196,-9.55025285786763));
#28020=CARTESIAN_POINT('Ctrl Pts',(153.365490544913,-7.66339294233319,-14.9583216894008));
#28021=CARTESIAN_POINT('Ctrl Pts',(153.483184371396,0.328434869711692,-16.8039016210083));
#28022=CARTESIAN_POINT('Ctrl Pts',(153.60087819788,8.24204230369565,-14.6474474846737));
#28023=CARTESIAN_POINT('Ctrl Pts',(153.718572024363,14.1927166741118,-9.00254256088617));
#28024=CARTESIAN_POINT('Ctrl Pts',(153.836265850846,16.7632394031106,-1.21358306933514));
#28025=CARTESIAN_POINT('Ctrl Pts',(153.953959677329,15.3414122187735,6.86440458349061));
#28026=CARTESIAN_POINT('Ctrl Pts',(154.071653503812,10.2658589097167,13.3075587542557));
#28027=CARTESIAN_POINT('Ctrl Pts',(154.189347330296,2.74537834388392,16.5813713817981));
#28028=CARTESIAN_POINT('Ctrl Pts',(154.307041156779,-5.42894428252613,15.9061479664124));
#28029=CARTESIAN_POINT('Ctrl Pts',(154.424734983262,-12.310304092225,11.4427003940996));
#28030=CARTESIAN_POINT('Ctrl Pts',(154.542428809745,-16.2598295294687,4.25404781646794));
#28031=CARTESIAN_POINT('Ctrl Pts',(154.660122636228,-16.33689765391,-3.94775305684763));
#28032=CARTESIAN_POINT('Ctrl Pts',(154.777816462712,-12.5231538437161,-11.2093531017091));
#28033=CARTESIAN_POINT('Ctrl Pts',(154.895510289195,-5.72688315071847,-15.8013223665045));
#28034=CARTESIAN_POINT('Ctrl Pts',(155.013204115678,2.4333077787351,-16.6300328444091));
#28035=CARTESIAN_POINT('Ctrl Pts',(155.130897942161,10.0139796864803,-13.4981180166325));
#28036=CARTESIAN_POINT('Ctrl Pts',(155.248591768644,15.2097121459439,-7.15147786053393));
#28037=CARTESIAN_POINT('Ctrl Pts',(155.366285595127,16.7830843021561,0.898365437281314));
#28038=CARTESIAN_POINT('Ctrl Pts',(155.483979421611,14.3593802639669,8.7342531213022));
#28039=CARTESIAN_POINT('Ctrl Pts',(155.601673248094,8.51583181660166,14.4899823196419));
#28040=CARTESIAN_POINT('Ctrl Pts',(155.719367074577,0.64414432060565,16.7947627922043));
#28041=CARTESIAN_POINT('Ctrl Pts',(155.83706090106,-7.38095323299944,15.0996857094594));
#28042=CARTESIAN_POINT('Ctrl Pts',(155.954754727543,-13.6481955599689,9.80845232995632));
#28043=CARTESIAN_POINT('Ctrl Pts',(156.072448554027,-16.6649699403357,2.18122810358885));
#28044=CARTESIAN_POINT('Ctrl Pts',(156.19014238051,-15.7127983612061,-5.96547959616457));
#28045=CARTESIAN_POINT('Ctrl Pts',(156.307836206993,-11.0184509610961,-12.6914426906518));
#28046=CARTESIAN_POINT('Ctrl Pts',(156.425530033476,-3.69993822624373,-16.3947990617195));
#28047=CARTESIAN_POINT('Ctrl Pts',(156.543223859959,4.49975550839517,-16.1935536407808));
#28048=CARTESIAN_POINT('Ctrl Pts',(156.660917686443,11.6277829569437,-12.1356352391784));
#28049=CARTESIAN_POINT('Ctrl Pts',(156.778611512926,15.9865259513294,-5.18748177439226));
#28050=CARTESIAN_POINT('Ctrl Pts',(156.896305339409,16.5379018872638,2.99612755392965));
#28051=CARTESIAN_POINT('Ctrl Pts',(157.013999165892,13.1505945186976,10.4661761382551));
#28052=CARTESIAN_POINT('Ctrl Pts',(157.131692992375,6.63132836671759,15.443589713695));
#28053=CARTESIAN_POINT('Ctrl Pts',(157.249386818858,-1.4672616017113,16.7429424697191));
#28054=CARTESIAN_POINT('Ctrl Pts',(157.367080645342,-9.21640707510144,14.0547792504258));
#28055=CARTESIAN_POINT('Ctrl Pts',(157.484774471825,-14.7705637934707,8.01931570492096));
#28056=CARTESIAN_POINT('Ctrl Pts',(157.602468298308,-16.8069482207728,0.0739638860544137));
#28057=CARTESIAN_POINT('Ctrl Pts',(157.720162124791,-14.8405729988752,-7.88900324611639));
#28058=CARTESIAN_POINT('Ctrl Pts',(157.837855951274,-9.33975202331718,-13.9731174508455));
#28059=CARTESIAN_POINT('Ctrl Pts',(157.955549777758,-1.61456633612997,-16.7293799854751));
#28060=CARTESIAN_POINT('Ctrl Pts',(158.073243604241,6.49514608942308,-15.5013565996409));
#28061=CARTESIAN_POINT('Ctrl Pts',(158.190937430724,13.0579680063074,-10.5815145748816));
#28062=CARTESIAN_POINT('Ctrl Pts',(158.308631257207,16.5108911628928,-3.14156842346082));
#28063=CARTESIAN_POINT('Ctrl Pts',(158.42632508369,16.0315639161914,5.04657681535204));
#28064=CARTESIAN_POINT('Ctrl Pts',(158.544018910174,11.7341433241446,12.0328242570317));
#28065=CARTESIAN_POINT('Ctrl Pts',(158.661712736657,4.64210738618032,16.1533222021771));
#28066=CARTESIAN_POINT('Ctrl Pts',(158.77940656314,-3.55549750389685,16.4267287264374));
#28067=CARTESIAN_POINT('Ctrl Pts',(158.897100389623,-10.9063215415264,12.7879290577097));
#28068=CARTESIAN_POINT('Ctrl Pts',(159.014794216106,-15.659685099468,6.10354337558762));
#28069=CARTESIAN_POINT('Ctrl Pts',(159.13248804259,-16.6835223441284,-2.03446832001538));
#28070=CARTESIAN_POINT('Ctrl Pts',(159.250181869073,-13.7339951701931,-9.68794899951949));
#28071=CARTESIAN_POINT('Ctrl Pts',(159.367875695556,-7.51356592840906,-15.0341380262265));
#28072=CARTESIAN_POINT('Ctrl Pts',(159.485569522039,0.496301712588155,-16.7997816581723));
#28073=CARTESIAN_POINT('Ctrl Pts',(159.603263348522,8.38796963981923,-14.5643724366568));
#28074=CARTESIAN_POINT('Ctrl Pts',(159.720957175005,14.281950302715,-8.86029766446685));
#28075=CARTESIAN_POINT('Ctrl Pts',(159.838651001489,16.7745273536853,-1.04604551174608));
#28076=CARTESIAN_POINT('Ctrl Pts',(159.956344827972,15.2720661416863,7.01733388945811));
#28077=CARTESIAN_POINT('Ctrl Pts',(160.074038654455,10.1323943362558,13.4094580116719));
#28078=CARTESIAN_POINT('Ctrl Pts',(160.191732480938,2.57958133075788,16.60797216129));
#28079=CARTESIAN_POINT('Ctrl Pts',(160.309426307421,-5.58758735234152,15.8511149996501));
#28080=CARTESIAN_POINT('Ctrl Pts',(160.427120133904,-12.4240106260698,11.3191403876568));
#28081=CARTESIAN_POINT('Ctrl Pts',(160.544813960388,-16.3015190651706,4.0913879454361));
#28082=CARTESIAN_POINT('Ctrl Pts',(160.662507786871,-16.2966413698226,-4.11077355440117));
#28083=CARTESIAN_POINT('Ctrl Pts',(160.780201613354,-12.4105392168435,-11.3339091005428));
#28084=CARTESIAN_POINT('Ctrl Pts',(160.897895439837,-5.56873059357299,-15.85774948498));
#28085=CARTESIAN_POINT('Ctrl Pts',(161.015589266321,2.59933249448306,-16.6048923433819));
#28086=CARTESIAN_POINT('Ctrl Pts',(161.133283092804,10.1483359479702,-13.3973973830485));
#28087=CARTESIAN_POINT('Ctrl Pts',(161.250976919287,15.2804015311513,-6.99916482153175));
#28088=CARTESIAN_POINT('Ctrl Pts',(161.36867074577,16.7732713561836,1.06599585553062));
#28089=CARTESIAN_POINT('Ctrl Pts',(161.486364572253,14.2714020478718,8.87727789021946));
#28090=CARTESIAN_POINT('Ctrl Pts',(161.604058398736,8.37064131058994,14.5743385167775));
#28091=CARTESIAN_POINT('Ctrl Pts',(161.72175222522,0.476320241246173,16.8003600610212));
#28092=CARTESIAN_POINT('Ctrl Pts',(161.839446051703,-7.53144173460349,15.0251909988012));
#28093=CARTESIAN_POINT('Ctrl Pts',(161.957139878186,-13.745507991303,9.67160737484704));
#28094=CARTESIAN_POINT('Ctrl Pts',(162.074833704669,-16.6859302751296,2.01462403582233));
#28095=CARTESIAN_POINT('Ctrl Pts',(162.192527531152,-15.652414665095,-6.12216418467065));
#28096=CARTESIAN_POINT('Ctrl Pts',(162.310221357636,-10.8911042757288,-12.8008916411092));
#28097=CARTESIAN_POINT('Ctrl Pts',(162.427915184119,-3.53595756595174,-16.4309459022901));
#28098=CARTESIAN_POINT('Ctrl Pts',(162.545609010602,4.66131634502582,-16.1477896036442));
#28099=CARTESIAN_POINT('Ctrl Pts',(162.663302837085,11.7484464790292,-12.0188595333448));
#28100=CARTESIAN_POINT('Ctrl Pts',(162.780996663568,16.0375548133002,-5.02750581908371));
#28101=CARTESIAN_POINT('Ctrl Pts',(162.898690490052,16.5071430043621,3.16120372464508));
#28102=CARTESIAN_POINT('Ctrl Pts',(163.016384316535,13.0453734569189,10.5970378180802));
#28103=CARTESIAN_POINT('Ctrl Pts',(163.134078143018,6.47670468054396,15.5090707534204));
#28104=CARTESIAN_POINT('Ctrl Pts',(163.251771969501,-1.63446258180371,16.7274478397662));
#28105=CARTESIAN_POINT('Ctrl Pts',(163.369465795984,-9.35636459237956,13.9619991663135));
#28106=CARTESIAN_POINT('Ctrl Pts',(163.487159622468,-14.8499454325485,7.87134676680609));
#28107=CARTESIAN_POINT('Ctrl Pts',(163.604853448951,-16.8068483558016,-0.0939534799261245));
#28108=CARTESIAN_POINT('Ctrl Pts',(163.722547275434,-14.7610154446685,-8.03687766216926));
#28109=CARTESIAN_POINT('Ctrl Pts',(163.840241101917,-9.19968422346793,-14.065731017089));
#28110=CARTESIAN_POINT('Ctrl Pts',(163.9579349284,-1.44734710828245,-16.7446757222752));
#28111=CARTESIAN_POINT('Ctrl Pts',(164.075628754883,6.64969191271279,-15.4356917405938));
#28112=CARTESIAN_POINT('Ctrl Pts',(164.193322581367,13.1630330900188,-10.4505277612649));
#28113=CARTESIAN_POINT('Ctrl Pts',(164.31101640785,16.5414542227863,-2.97645594967455));
#28114=CARTESIAN_POINT('Ctrl Pts',(164.428710234333,15.9803437226336,5.20649230148));
#28115=CARTESIAN_POINT('Ctrl Pts',(164.546404060816,11.6133432492922,12.1494556775476));
#28116=CARTESIAN_POINT('Ctrl Pts',(164.664097887299,4.48048761558814,16.198895465931));
#28117=CARTESIAN_POINT('Ctrl Pts',(164.781791713783,-3.7194255831206,16.3903839769258));
#28118=CARTESIAN_POINT('Ctrl Pts',(164.899485540266,-11.0335573949518,12.6783346740863));
#28119=CARTESIAN_POINT('Ctrl Pts',(165.017179366749,-15.7198425322127,5.94677487077617));
#28120=CARTESIAN_POINT('Ctrl Pts',(165.134873193232,-16.662445658167,-2.20102228593978));
#28121=CARTESIAN_POINT('Ctrl Pts',(165.252567019715,-13.6363522564438,-9.82472948326341));
#28122=CARTESIAN_POINT('Ctrl Pts',(165.370260846199,-7.3633357798665,-15.1083454196505));
#28123=CARTESIAN_POINT('Ctrl Pts',(165.487954672682,0.664832031569472,-16.7941947463207));
#28124=CARTESIAN_POINT('Ctrl Pts',(165.56641722367,5.90882141440849,-15.2504240636636));
#28125=CARTESIAN_POINT('Ctrl Pts',(165.605648499165,8.19367851963193,-13.9039439059363));
#28126=CARTESIAN_POINT('Ctrl Pts',(150.,-7.06535955977555,14.8277213114857));
#28127=CARTESIAN_POINT('Ctrl Pts',(150.039231275494,-9.50202246794194,13.6666595940101));
#28128=CARTESIAN_POINT('Ctrl Pts',(150.117693826483,-13.7897027968609,10.1214825126218));
#28129=CARTESIAN_POINT('Ctrl Pts',(150.235387652966,-16.9377394031488,2.38891419744853));
#28130=CARTESIAN_POINT('Ctrl Pts',(150.35308147945,-16.0513990934872,-5.91108433372057));
#28131=CARTESIAN_POINT('Ctrl Pts',(150.470775305933,-11.3424649473698,-12.8040315227983));
#28132=CARTESIAN_POINT('Ctrl Pts',(150.588469132416,-3.9320885972612,-16.6471996464972));
#28133=CARTESIAN_POINT('Ctrl Pts',(150.706162958899,4.41470461516072,-16.5258285446613));
#28134=CARTESIAN_POINT('Ctrl Pts',(150.823856785382,11.710113332741,-12.4685644587302));
#28135=CARTESIAN_POINT('Ctrl Pts',(150.941550611866,16.2166170441621,-5.44181602655281));
#28136=CARTESIAN_POINT('Ctrl Pts',(151.059244438349,16.8609611465387,2.88098098727637));
#28137=CARTESIAN_POINT('Ctrl Pts',(151.176938264832,13.4896788170136,10.517630823419));
#28138=CARTESIAN_POINT('Ctrl Pts',(151.294632091315,6.90568251477146,15.6493959555621));
#28139=CARTESIAN_POINT('Ctrl Pts',(151.412325917798,-1.32297877835631,17.0540829052685));
#28140=CARTESIAN_POINT('Ctrl Pts',(151.530019744282,-9.23655776971034,14.39715350305));
#28141=CARTESIAN_POINT('Ctrl Pts',(151.647713570765,-14.9503490663786,8.31138302260808));
#28142=CARTESIAN_POINT('Ctrl Pts',(151.765407397248,-17.1035501481607,0.246165494714576));
#28143=CARTESIAN_POINT('Ctrl Pts',(151.883101223731,-15.183352608554,-7.87767918660661));
#28144=CARTESIAN_POINT('Ctrl Pts',(152.000795050214,-9.64707255987471,-14.1253678253907));
#28145=CARTESIAN_POINT('Ctrl Pts',(152.118488876697,-1.81323604187045,-17.0089447235611));
#28146=CARTESIAN_POINT('Ctrl Pts',(152.236182703181,6.45244259560576,-15.8416542674624));
#28147=CARTESIAN_POINT('Ctrl Pts',(152.353876529664,13.1814010290606,-10.9014995459474));
#28148=CARTESIAN_POINT('Ctrl Pts',(152.471570356147,16.7710637708,-3.36503275240856));
#28149=CARTESIAN_POINT('Ctrl Pts',(152.58926418263,16.3665131394028,4.97285361551223));
#28150=CARTESIAN_POINT('Ctrl Pts',(152.706958009113,12.0640973198993,12.1264001783988));
#28151=CARTESIAN_POINT('Ctrl Pts',(152.824651835597,4.8884839797065,16.39191110902));
#28152=CARTESIAN_POINT('Ctrl Pts',(152.94234566208,-3.45137560921858,16.7535080455525));
#28153=CARTESIAN_POINT('Ctrl Pts',(153.060039488563,-10.9692521206197,13.1250726985274));
#28154=CARTESIAN_POINT('Ctrl Pts',(153.177733315046,-15.8746805424682,6.37075687043291));
#28155=CARTESIAN_POINT('Ctrl Pts',(153.295427141529,-16.9993791206519,-1.90082480517061));
#28156=CARTESIAN_POINT('Ctrl Pts',(153.413120968012,-14.0754885134681,-9.71970413823186));
#28157=CARTESIAN_POINT('Ctrl Pts',(153.530814794496,-7.79936544121243,-15.2237289828089));
#28158=CARTESIAN_POINT('Ctrl Pts',(153.648508620979,0.33426232894414,-17.1020552602022));
#28159=CARTESIAN_POINT('Ctrl Pts',(153.766202447462,8.38828184750279,-14.9073388998315));
#28160=CARTESIAN_POINT('Ctrl Pts',(153.883896273945,14.4445397460312,-9.16227575184762));
#28161=CARTESIAN_POINT('Ctrl Pts',(154.001590100428,17.0606715677019,-1.23511581909452));
#28162=CARTESIAN_POINT('Ctrl Pts',(154.119283926912,15.6136167333299,6.9862005362179));
#28163=CARTESIAN_POINT('Ctrl Pts',(154.236977753395,10.4480072739726,13.5436763631809));
#28164=CARTESIAN_POINT('Ctrl Pts',(154.354671579878,2.79408992067451,16.8755766403035));
#28165=CARTESIAN_POINT('Ctrl Pts',(154.472365406361,-5.52527069119732,16.1883726549819));
#28166=CARTESIAN_POINT('Ctrl Pts',(154.590059232844,-12.528727292233,11.6457295977722));
#28167=CARTESIAN_POINT('Ctrl Pts',(154.707753059327,-16.5483296323747,4.3295278964155));
#28168=CARTESIAN_POINT('Ctrl Pts',(154.825446885811,-16.6267651857789,-4.01779851218795));
#28169=CARTESIAN_POINT('Ctrl Pts',(154.943140712294,-12.7453536623595,-11.408241996423));
#28170=CARTESIAN_POINT('Ctrl Pts',(155.060834538777,-5.82849592441443,-16.0816871218991));
#28171=CARTESIAN_POINT('Ctrl Pts',(155.17852836526,2.47648225010914,-16.9251015090742));
#28172=CARTESIAN_POINT('Ctrl Pts',(155.296222191744,10.1916589275088,-13.7376167413748));
#28173=CARTESIAN_POINT('Ctrl Pts',(155.413916018227,15.4795798903333,-7.2783673888008));
#28174=CARTESIAN_POINT('Ctrl Pts',(155.53160984471,17.0808685771681,0.91430524283911));
#28175=CARTESIAN_POINT('Ctrl Pts',(155.649303671193,14.6141604679237,8.88922602060199));
#28176=CARTESIAN_POINT('Ctrl Pts',(155.766997497676,8.66692924053017,14.7470798115157));
#28177=CARTESIAN_POINT('Ctrl Pts',(155.884691324159,0.655573450440289,17.0927542800641));
#28178=CARTESIAN_POINT('Ctrl Pts',(156.002385150643,-7.51191437028597,15.3676012416077));
#28179=CARTESIAN_POINT('Ctrl Pts',(156.120078977126,-13.8903571285385,9.98248487448037));
#28180=CARTESIAN_POINT('Ctrl Pts',(156.237772803609,-16.9606584980785,2.21992989509328));
#28181=CARTESIAN_POINT('Ctrl Pts',(156.355466630092,-15.9915924245715,-6.07132581517059));
#28182=CARTESIAN_POINT('Ctrl Pts',(156.473160456575,-11.2139526562633,-12.9166284784635));
#28183=CARTESIAN_POINT('Ctrl Pts',(156.590854283059,-3.76558667336199,-16.6856939452026));
#28184=CARTESIAN_POINT('Ctrl Pts',(156.708548109542,4.57959520935088,-16.4808778026554));
#28185=CARTESIAN_POINT('Ctrl Pts',(156.826241936025,11.8340961026976,-12.3509592688053));
#28186=CARTESIAN_POINT('Ctrl Pts',(156.943935762508,16.2701767961127,-5.27952388485984));
#28187=CARTESIAN_POINT('Ctrl Pts',(157.061629588991,16.831335861321,3.04928820398821));
#28188=CARTESIAN_POINT('Ctrl Pts',(157.179323415474,13.3839270923905,10.6518787550904));
#28189=CARTESIAN_POINT('Ctrl Pts',(157.297017241958,6.74898882021338,15.7176071757824));
#28190=CARTESIAN_POINT('Ctrl Pts',(157.414711068441,-1.49329540005564,17.04001450339));
#28191=CARTESIAN_POINT('Ctrl Pts',(157.532404894924,-9.37993488975477,14.3041548821149));
#28192=CARTESIAN_POINT('Ctrl Pts',(157.650098721407,-15.032639676042,8.16160338400838));
#28193=CARTESIAN_POINT('Ctrl Pts',(157.76779254789,-17.1051559161512,0.0752762361439129));
#28194=CARTESIAN_POINT('Ctrl Pts',(157.885486374374,-15.1038910631636,-8.0289787756387));
#28195=CARTESIAN_POINT('Ctrl Pts',(158.003180200857,-9.50546836216071,-14.2210441474433));
#28196=CARTESIAN_POINT('Ctrl Pts',(158.12087402734,-1.64321378002094,-17.0262113783636));
#28197=CARTESIAN_POINT('Ctrl Pts',(158.238567853823,6.61039024446121,-15.7763990265048));
#28198=CARTESIAN_POINT('Ctrl Pts',(158.356261680306,13.2896570966964,-10.7692636554129));
#28199=CARTESIAN_POINT('Ctrl Pts',(158.47395550679,16.8038458824322,-3.19730964828806));
#28200=CARTESIAN_POINT('Ctrl Pts',(158.591649333273,16.3160138749799,5.13611883225406));
#28201=CARTESIAN_POINT('Ctrl Pts',(158.709343159756,11.9423436346333,12.246324099088));
#28202=CARTESIAN_POINT('Ctrl Pts',(158.827036986239,4.72447285355417,16.4399325328178));
#28203=CARTESIAN_POINT('Ctrl Pts',(158.944730812722,-3.61858312197772,16.7181901417859));
#28204=CARTESIAN_POINT('Ctrl Pts',(159.062424639206,-11.0998337109716,13.0148268146891));
#28205=CARTESIAN_POINT('Ctrl Pts',(159.180118465689,-15.9375367678685,6.21183927676893));
#28206=CARTESIAN_POINT('Ctrl Pts',(159.297812292172,-16.9795400793939,-2.07056613510129));
#28207=CARTESIAN_POINT('Ctrl Pts',(159.415506118655,-13.9776790915239,-9.85984343901797));
#28208=CARTESIAN_POINT('Ctrl Pts',(159.533199945138,-7.6468800286343,-15.30089053798));
#28209=CARTESIAN_POINT('Ctrl Pts',(159.650893771621,0.50510765332046,-17.097862196372));
#28210=CARTESIAN_POINT('Ctrl Pts',(159.768587598105,8.53679838983004,-14.8227898412871));
#28211=CARTESIAN_POINT('Ctrl Pts',(159.886281424588,14.5353566575949,-9.01750698719337));
#28212=CARTESIAN_POINT('Ctrl Pts',(160.003975251071,17.0721598017356,-1.06460562255391));
#28213=CARTESIAN_POINT('Ctrl Pts',(160.121669077554,15.5430402404909,7.1418432851787));
#28214=CARTESIAN_POINT('Ctrl Pts',(160.239362904038,10.3121746225986,13.6473836313267));
#28215=CARTESIAN_POINT('Ctrl Pts',(160.35705673052,2.62535115128579,16.9026494006121));
#28216=CARTESIAN_POINT('Ctrl Pts',(160.474750557004,-5.68672858400233,16.1323632316986));
#28217=CARTESIAN_POINT('Ctrl Pts',(160.592444383487,-12.6444513347273,11.5199772513354));
#28218=CARTESIAN_POINT('Ctrl Pts',(160.71013820997,-16.590758870502,4.16398193180893));
#28219=CARTESIAN_POINT('Ctrl Pts',(160.827832036453,-16.5857946296213,-4.1837115019558));
#28220=CARTESIAN_POINT('Ctrl Pts',(160.945525862937,-12.6307409006735,-11.535008007263));
#28221=CARTESIAN_POINT('Ctrl Pts',(161.06321968942,-5.66753724750438,-16.1391154334964));
#28222=CARTESIAN_POINT('Ctrl Pts',(161.180913515903,2.64545276227466,-16.899514937126));
#28223=CARTESIAN_POINT('Ctrl Pts',(161.298607342386,10.3283990882391,-13.6351090095251));
#28224=CARTESIAN_POINT('Ctrl Pts',(161.416301168869,15.5515235257695,-7.1233518413039));
#28225=CARTESIAN_POINT('Ctrl Pts',(161.533994995353,17.0708815189199,1.0849099476778));
#28226=CARTESIAN_POINT('Ctrl Pts',(161.651688821836,14.5246212438026,9.03478849512532));
#28227=CARTESIAN_POINT('Ctrl Pts',(161.769382648319,8.51916260197972,14.8329327507611));
#28228=CARTESIAN_POINT('Ctrl Pts',(161.887076474802,0.484771648339155,17.098450861892));
#28229=CARTESIAN_POINT('Ctrl Pts',(162.004770301285,-7.66507300739915,15.2917847623754));
#28230=CARTESIAN_POINT('Ctrl Pts',(162.122464127769,-13.9893961859976,9.84321186294161));
#28231=CARTESIAN_POINT('Ctrl Pts',(162.240157954252,-16.9819907346032,2.05036975139694));
#28232=CARTESIAN_POINT('Ctrl Pts',(162.357851780735,-15.9301373333076,-6.23079047709786));
#28233=CARTESIAN_POINT('Ctrl Pts',(162.475545607218,-11.0843464434042,-13.0280193947584));
#28234=CARTESIAN_POINT('Ctrl Pts',(162.593239433701,-3.59869648457321,-16.722482143495));
#28235=CARTESIAN_POINT('Ctrl Pts',(162.710933260184,4.74402263925723,-16.4343017687264));
#28236=CARTESIAN_POINT('Ctrl Pts',(162.828627086668,11.9569005721082,-12.232111597636));
#28237=CARTESIAN_POINT('Ctrl Pts',(162.946320913151,16.3221110692936,-5.11670945701468));
#28238=CARTESIAN_POINT('Ctrl Pts',(163.064014739634,16.8000312198758,3.21729334097308));
#28239=CARTESIAN_POINT('Ctrl Pts',(163.181708566117,13.2768390807095,10.785062329375));
#28240=CARTESIAN_POINT('Ctrl Pts',(163.2994023926,6.59162162745551,15.7842500534388));
#28241=CARTESIAN_POINT('Ctrl Pts',(163.417096219084,-1.66346304716478,17.0242449503621));
#28242=CARTESIAN_POINT('Ctrl Pts',(163.534790045567,-9.52237569002574,14.2097285898572));
#28243=CARTESIAN_POINT('Ctrl Pts',(163.65248387205,-15.1134297930502,8.01100901530118));
#28244=CARTESIAN_POINT('Ctrl Pts',(163.770177698533,-17.1050542792638,-0.0956205077739737));
#28245=CARTESIAN_POINT('Ctrl Pts',(163.887871525016,-15.0229219097434,-8.17947694516765));
#28246=CARTESIAN_POINT('Ctrl Pts',(164.0055653515,-9.36291532256174,-14.3153009672858));
#28247=CARTESIAN_POINT('Ctrl Pts',(164.123259177983,-1.47302756138459,-17.0417785092538));
#28248=CARTESIAN_POINT('Ctrl Pts',(164.240953004466,6.76767819280469,-15.7095690679985));
#28249=CARTESIAN_POINT('Ctrl Pts',(164.358646830949,13.3965863627725,-10.635952727073));
#28250=CARTESIAN_POINT('Ctrl Pts',(164.476340657432,16.8349512263582,-3.02926756410262));
#28251=CARTESIAN_POINT('Ctrl Pts',(164.594034483916,16.2638848753927,5.2988717180067));
#28252=CARTESIAN_POINT('Ctrl Pts',(164.711728310399,11.8194001895836,12.3650249248679));
#28253=CARTESIAN_POINT('Ctrl Pts',(164.829422136882,4.55998544401394,16.4863144084491));
#28254=CARTESIAN_POINT('Ctrl Pts',(164.947115963365,-3.78541979674606,16.6812005230305));
#28255=CARTESIAN_POINT('Ctrl Pts',(165.064809789848,-11.2293271253843,12.9032878847901));
#28256=CARTESIAN_POINT('Ctrl Pts',(165.182503616331,-15.998761581148,6.05228920959924));
#28257=CARTESIAN_POINT('Ctrl Pts',(165.300197442814,-16.9580894272689,-2.24007528799254));
#28258=CARTESIAN_POINT('Ctrl Pts',(165.417891269298,-13.8783036878605,-9.99905083526821));
#28259=CARTESIAN_POINT('Ctrl Pts',(165.535585095781,-7.49398432857193,-15.3764146020739));
#28260=CARTESIAN_POINT('Ctrl Pts',(165.653278922264,0.676628225937629,-17.0921761552743));
#28261=CARTESIAN_POINT('Ctrl Pts',(165.731741473253,6.01366234050923,-15.5210141644856));
#28262=CARTESIAN_POINT('Ctrl Pts',(165.770972748747,8.33905993902552,-14.1506432480414));
#28263=CARTESIAN_POINT('Ctrl Pts',(165.268843152848,-16.4247445391107,-0.000389063610209933));
#28264=CARTESIAN_POINT('Ctrl Pts',(165.270895435232,-16.4248785782203,-0.141592307580833));
#28265=CARTESIAN_POINT('Ctrl Pts',(165.272947717616,-16.4231982118296,-0.282792220533225));
#28266=CARTESIAN_POINT('Ctrl Pts',(165.275,-16.4196979759281,-0.423941685645475));
#28267=CARTESIAN_POINT('Ctrl Pts',(150.,-9.03713009573195,-12.6741506013615));
#28268=CARTESIAN_POINT('Ctrl Pts',(150.030832127889,-7.39916843321553,-13.8395576086113));
#28269=CARTESIAN_POINT('Ctrl Pts',(150.100895531273,-3.16192523972154,-15.7683197386922));
#28270=CARTESIAN_POINT('Ctrl Pts',(150.210190210152,4.18380951624729,-15.6615050736542));
#28271=CARTESIAN_POINT('Ctrl Pts',(150.327884036635,11.0976583641875,-11.8164414573133));
#28272=CARTESIAN_POINT('Ctrl Pts',(150.445577863118,15.3684657582085,-5.15720159382155));
#28273=CARTESIAN_POINT('Ctrl Pts',(150.563271689601,15.9791097813677,2.73030173509255));
#28274=CARTESIAN_POINT('Ctrl Pts',(150.680965516085,12.7841501358716,9.96754432364079));
#28275=CARTESIAN_POINT('Ctrl Pts',(150.798659342568,6.54450585940981,14.8309111095575));
#28276=CARTESIAN_POINT('Ctrl Pts',(150.916353169051,-1.25378517594862,16.1621310075655));
#28277=CARTESIAN_POINT('Ctrl Pts',(151.034046995534,-8.75347314553567,13.6441626527123));
#28278=CARTESIAN_POINT('Ctrl Pts',(151.151740822017,-14.1684253302768,7.87668630506945));
#28279=CARTESIAN_POINT('Ctrl Pts',(151.231348624873,-15.5486722830063,2.7067130916238));
#28280=CARTESIAN_POINT('Ctrl Pts',(151.271725152234,-15.5672190915335,0.0747297253538588));
#28281=CARTESIAN_POINT('Ctrl Pts',(151.272870404101,-15.5671986622434,7.50751021387757E-5));
#28282=CARTESIAN_POINT('Origin',(147.227129595899,0.,0.));
#28283=CARTESIAN_POINT('Ctrl Pts',(150.,9.03673727728059,-12.6742328676692));
#28284=CARTESIAN_POINT('Ctrl Pts',(150.039231275494,11.1195140215529,-11.1892115301467));
#28285=CARTESIAN_POINT('Ctrl Pts',(150.117693826483,14.5370057041716,-7.17421629738743));
#28286=CARTESIAN_POINT('Ctrl Pts',(150.235387652966,16.2010328735656,0.560984685021083));
#28287=CARTESIAN_POINT('Ctrl Pts',(150.35308147945,14.0064191663237,8.1610886176298));
#28288=CARTESIAN_POINT('Ctrl Pts',(150.470775305933,8.47610941309655,13.8182656780649));
#28289=CARTESIAN_POINT('Ctrl Pts',(150.588469132416,0.927077910240183,16.1841184068341));
#28290=CARTESIAN_POINT('Ctrl Pts',(150.706162958899,-6.84272643302437,14.6957170013813));
#28291=CARTESIAN_POINT('Ctrl Pts',(150.823856785382,-12.9828704069121,9.70728517421879));
#28292=CARTESIAN_POINT('Ctrl Pts',(150.914178997716,-15.3221047690584,4.10479808015603));
#28293=CARTESIAN_POINT('Ctrl Pts',(150.965269934555,-15.5660958690062,0.773696244953541));
#28294=CARTESIAN_POINT('Ctrl Pts',(150.977129595899,-15.5654260231298,0.000355229555255854));
#28295=CARTESIAN_POINT('Ctrl Pts',(149.504027251253,9.53545461596197,-13.3736954603778));
#28296=CARTESIAN_POINT('Ctrl Pts',(149.543258526747,11.7331751550021,-11.8067191133635));
#28297=CARTESIAN_POINT('Ctrl Pts',(149.621721077736,15.3392705675541,-7.57014526479843));
#28298=CARTESIAN_POINT('Ctrl Pts',(149.739414904219,17.0951316783309,0.591944176325289));
#28299=CARTESIAN_POINT('Ctrl Pts',(149.857108730702,14.7794021442229,8.61148086333111));
#28300=CARTESIAN_POINT('Ctrl Pts',(149.974802557185,8.94388695261846,14.5808648853565));
#28301=CARTESIAN_POINT('Ctrl Pts',(150.092496383669,0.978241268647,17.0772837399741));
#28302=CARTESIAN_POINT('Ctrl Pts',(150.210190210152,-7.2203612155008,15.5067407866328));
#28303=CARTESIAN_POINT('Ctrl Pts',(150.327884036635,-13.6993660157928,10.2430085530626));
#28304=CARTESIAN_POINT('Ctrl Pts',(150.445577863118,-16.9157108038983,2.53983419096766));
#28305=CARTESIAN_POINT('Ctrl Pts',(150.563271689601,-16.1033955003998,-5.76825062376693));
#28306=CARTESIAN_POINT('Ctrl Pts',(150.680965516084,-11.4558781196984,-12.7025528487927));
#28307=CARTESIAN_POINT('Ctrl Pts',(150.798659342568,-4.08001792255419,-16.6116073332124));
#28308=CARTESIAN_POINT('Ctrl Pts',(150.916353169051,4.26754373314548,-16.5644223179528));
#28309=CARTESIAN_POINT('Ctrl Pts',(151.034046995534,11.5987427473219,-12.5722390515179));
#28310=CARTESIAN_POINT('Ctrl Pts',(151.151740822017,16.1675736233743,-5.58583814191949));
#28311=CARTESIAN_POINT('Ctrl Pts',(151.2694346485,16.8859189113636,2.73089130155499));
#28312=CARTESIAN_POINT('Ctrl Pts',(151.387128474984,13.5826968280316,10.3972290703567));
#28313=CARTESIAN_POINT('Ctrl Pts',(151.504822301467,7.04460603362714,15.5873522661647));
#28314=CARTESIAN_POINT('Ctrl Pts',(151.62251612795,-1.17123519699634,17.0651760414828));
#28315=CARTESIAN_POINT('Ctrl Pts',(151.740209954433,-9.10813388004872,14.4787403548484));
#28316=CARTESIAN_POINT('Ctrl Pts',(151.857903780917,-14.8758302598876,8.44403334780864));
#28317=CARTESIAN_POINT('Ctrl Pts',(151.975597607399,-17.1006839818747,0.398286883712695));
#28318=CARTESIAN_POINT('Ctrl Pts',(152.093291433883,-15.2528216508935,-7.74231598233075));
#28319=CARTESIAN_POINT('Ctrl Pts',(152.210985260366,-9.77233201382398,-14.0390011077331));
#28320=CARTESIAN_POINT('Ctrl Pts',(152.328679086849,-1.96445398056304,-16.9921436447781));
#28321=CARTESIAN_POINT('Ctrl Pts',(152.446372913332,6.31128038344754,-15.8984202048656));
#28322=CARTESIAN_POINT('Ctrl Pts',(152.564066739816,13.0839138797936,-11.0183130593643));
#28323=CARTESIAN_POINT('Ctrl Pts',(152.681760566299,16.7404693205759,-3.51407342198624));
#28324=CARTESIAN_POINT('Ctrl Pts',(152.799454392782,16.4100977937248,4.82708146695919));
#28325=CARTESIAN_POINT('Ctrl Pts',(152.917148219265,12.1714809135036,12.0186137911331));
#28326=CARTESIAN_POINT('Ctrl Pts',(153.034842045748,5.03409192834135,16.3477809975931));
#28327=CARTESIAN_POINT('Ctrl Pts',(153.152535872231,-3.30222144073897,16.7835442813653));
#28328=CARTESIAN_POINT('Ctrl Pts',(153.270229698715,-10.8520744386629,13.2221218216275));
#28329=CARTESIAN_POINT('Ctrl Pts',(153.387923525198,-15.8173865013383,6.51170556425243));
#28330=CARTESIAN_POINT('Ctrl Pts',(153.505617351681,-17.0156139266551,-1.74954502292907));
#28331=CARTESIAN_POINT('Ctrl Pts',(153.623311178164,-14.1613856689232,-9.59412221228455));
#28332=CARTESIAN_POINT('Ctrl Pts',(153.741005004647,-7.93446759340149,-15.1537536306189));
#28333=CARTESIAN_POINT('Ctrl Pts',(153.858698831131,0.182131244121732,-17.1043518818501));
#28334=CARTESIAN_POINT('Ctrl Pts',(153.976392657614,8.25535352182861,-14.9813605296003));
#28335=CARTESIAN_POINT('Ctrl Pts',(154.094086484097,14.362472522903,-9.29039332413286));
#28336=CARTESIAN_POINT('Ctrl Pts',(154.21178031058,17.0490106593108,-1.38681672435119));
#28337=CARTESIAN_POINT('Ctrl Pts',(154.329474137064,15.6751393133167,6.84704553777379));
#28338=CARTESIAN_POINT('Ctrl Pts',(154.447167963546,10.5680610629674,13.4502085655809));
#28339=CARTESIAN_POINT('Ctrl Pts',(154.56486179003,2.9440827878509,16.850056427992));
#28340=CARTESIAN_POINT('Ctrl Pts',(154.682555616513,-5.38106119756087,16.2368779473254));
#28341=CARTESIAN_POINT('Ctrl Pts',(154.800249442996,-12.4246462498137,11.7567083256848));
#28342=CARTESIAN_POINT('Ctrl Pts',(154.917943269479,-16.5091650866505,4.47654925472243));
#28343=CARTESIAN_POINT('Ctrl Pts',(155.035637095962,-16.6618446042499,-3.86974927767475));
#28344=CARTESIAN_POINT('Ctrl Pts',(155.153330922446,-12.8463224955304,-11.2944244399201));
#28345=CARTESIAN_POINT('Ctrl Pts',(155.271024748929,-5.97130733368415,-16.0292081468463));
#28346=CARTESIAN_POINT('Ctrl Pts',(155.388718575412,2.32584037324249,-16.9464595608177));
#28347=CARTESIAN_POINT('Ctrl Pts',(155.506412401895,10.0690636035655,-13.8277251648847));
#28348=CARTESIAN_POINT('Ctrl Pts',(155.624106228379,15.414228544653,-7.41576587153617));
#28349=CARTESIAN_POINT('Ctrl Pts',(155.741800054862,17.0883253517992,0.762339661366479));
#28350=CARTESIAN_POINT('Ctrl Pts',(155.859493881345,14.6926494499394,8.75888561572939));
#28351=CARTESIAN_POINT('Ctrl Pts',(155.977187707828,8.79775741523248,14.6694065848267));
#28352=CARTESIAN_POINT('Ctrl Pts',(156.094881534311,0.807582648493649,17.0862469651497));
#28353=CARTESIAN_POINT('Ctrl Pts',(156.212575360794,-7.37492681198748,15.4338096271162));
#28354=CARTESIAN_POINT('Ctrl Pts',(156.330269187278,-13.8010163043069,10.1056407048979));
#28355=CARTESIAN_POINT('Ctrl Pts',(156.447963013761,-16.9402419082406,2.37070225429615));
#28356=CARTESIAN_POINT('Ctrl Pts',(156.565656840244,-16.0449625046453,-5.92884502350692));
#28357=CARTESIAN_POINT('Ctrl Pts',(156.683350666727,-11.3283987344367,-12.8163726226201));
#28358=CARTESIAN_POINT('Ctrl Pts',(156.80104449321,-3.91385215684362,-16.651540060385));
#28359=CARTESIAN_POINT('Ctrl Pts',(156.918738319694,4.43282137684879,-16.5209600123355));
#28360=CARTESIAN_POINT('Ctrl Pts',(157.036432146177,11.7237697243691,-12.4557315537146));
#28361=CARTESIAN_POINT('Ctrl Pts',(157.15412597266,16.2225733129014,-5.42403357251556));
#28362=CARTESIAN_POINT('Ctrl Pts',(157.271819799143,16.8577925665448,2.89945768577206));
#28363=CARTESIAN_POINT('Ctrl Pts',(157.389513625626,13.4781430305917,10.5324111928441));
#28364=CARTESIAN_POINT('Ctrl Pts',(157.50720745211,6.8885254290314,15.6569550839818));
#28365=CARTESIAN_POINT('Ctrl Pts',(157.624901278593,-1.34167029936179,17.0526228450654));
#28366=CARTESIAN_POINT('Ctrl Pts',(157.742595105076,-9.25233248327858,14.3870208419639));
#28367=CARTESIAN_POINT('Ctrl Pts',(157.860288931559,-14.9594498809222,8.29499152190118));
#28368=CARTESIAN_POINT('Ctrl Pts',(157.977982758042,-17.1038096874183,0.227418699343366));
#28369=CARTESIAN_POINT('Ctrl Pts',(158.095676584525,-15.1747090200033,-7.89431638879937));
#28370=CARTESIAN_POINT('Ctrl Pts',(158.213370411009,-9.63158442892658,-14.1359331661088));
#28371=CARTESIAN_POINT('Ctrl Pts',(158.331064237492,-1.79459202773081,-17.010921919233));
#28372=CARTESIAN_POINT('Ctrl Pts',(158.448758063975,6.46980221114646,-15.8345724425031));
#28373=CARTESIAN_POINT('Ctrl Pts',(158.566451890458,13.1933418648307,-10.8870453074258));
#28374=CARTESIAN_POINT('Ctrl Pts',(158.684145716941,16.7747419842613,-3.346648539912));
#28375=CARTESIAN_POINT('Ctrl Pts',(158.801839543425,16.3610527240895,4.99078940126682));
#28376=CARTESIAN_POINT('Ctrl Pts',(158.919533369908,12.0507987335361,12.1396159318177));
#28377=CARTESIAN_POINT('Ctrl Pts',(159.037227196391,4.87051442709172,16.3972593534324));
#28378=CARTESIAN_POINT('Ctrl Pts',(159.154921022874,-3.46973648146967,16.7497150374982));
#28379=CARTESIAN_POINT('Ctrl Pts',(159.272614849357,-10.9836314687213,13.11304178471));
#28380=CARTESIAN_POINT('Ctrl Pts',(159.390308675841,-15.8816537664659,6.35335334530791));
#28381=CARTESIAN_POINT('Ctrl Pts',(159.508002502324,-16.9972854705154,-1.91945610057624));
#28382=CARTESIAN_POINT('Ctrl Pts',(159.625696328807,-14.0648266150179,-9.73512595592479));
#28383=CARTESIAN_POINT('Ctrl Pts',(159.74339015529,-7.78267454287779,-15.2322684472103));
#28384=CARTESIAN_POINT('Ctrl Pts',(159.861083981773,0.353007106070388,-17.1016786039061));
#28385=CARTESIAN_POINT('Ctrl Pts',(159.978777808256,8.40461622849572,-14.898135827678));
#28386=CARTESIAN_POINT('Ctrl Pts',(160.09647163474,14.4545735183265,-9.146438076734));
#28387=CARTESIAN_POINT('Ctrl Pts',(160.214165461223,17.0620150780238,-1.21641545761408));
#28388=CARTESIAN_POINT('Ctrl Pts',(160.331859287706,15.6059500099123,7.00330988721436));
#28389=CARTESIAN_POINT('Ctrl Pts',(160.449553114189,10.4331562313559,13.5551199234958));
#28390=CARTESIAN_POINT('Ctrl Pts',(160.567246940672,2.77559149806718,16.8786290001319));
#28391=CARTESIAN_POINT('Ctrl Pts',(160.684940767155,-5.54301089090938,16.182306861245));
#28392=CARTESIAN_POINT('Ctrl Pts',(160.802634593639,-12.5414842452891,11.6319902859914));
#28393=CARTESIAN_POINT('Ctrl Pts',(160.920328420122,-16.5530651300371,4.31138723486822));
#28394=CARTESIAN_POINT('Ctrl Pts',(161.038022246605,-16.6223514171736,-4.03602012534875));
#28395=CARTESIAN_POINT('Ctrl Pts',(161.155716073088,-12.7328418150455,-11.4222048835269));
#28396=CARTESIAN_POINT('Ctrl Pts',(161.273409899572,-5.8108658325,-16.0880658677455));
#28397=CARTESIAN_POINT('Ctrl Pts',(161.391103726055,2.49503178624673,-16.9223769451532));
#28398=CARTESIAN_POINT('Ctrl Pts',(161.508797552538,10.2067101317342,-13.7264377525632));
#28399=CARTESIAN_POINT('Ctrl Pts',(161.626491379021,15.4875481527481,-7.26139637428879));
#28400=CARTESIAN_POINT('Ctrl Pts',(161.744185205504,17.079856168403,0.933026449209681));
#28401=CARTESIAN_POINT('Ctrl Pts',(161.861879031988,14.604408504263,8.90523875754094));
#28402=CARTESIAN_POINT('Ctrl Pts',(161.979572858471,8.65076025942847,14.7565704695287));
#28403=CARTESIAN_POINT('Ctrl Pts',(162.097266684954,0.636838272645602,17.0934625545191));
#28404=CARTESIAN_POINT('Ctrl Pts',(162.214960511437,-7.52875375600992,15.3593584491469));
#28405=CARTESIAN_POINT('Ctrl Pts',(162.33265433792,-13.901290237245,9.96725412683175));
#28406=CARTESIAN_POINT('Ctrl Pts',(162.450348164403,-16.9630814895256,2.2013385623837));
#28407=CARTESIAN_POINT('Ctrl Pts',(162.568041990887,-15.984928236899,-6.08885000246564));
#28408=CARTESIAN_POINT('Ctrl Pts',(162.68573581737,-11.1997884386548,-12.9289119423714));
#28409=CARTESIAN_POINT('Ctrl Pts',(162.803429643853,-3.74729579099151,-16.6898112435252));
#28410=CARTESIAN_POINT('Ctrl Pts',(162.921123470336,4.59765658343188,-16.4758483557211));
#28411=CARTESIAN_POINT('Ctrl Pts',(163.038817296819,11.8476264497369,-12.3379808942753));
#28412=CARTESIAN_POINT('Ctrl Pts',(163.156511123302,16.275953722843,-5.26168752638849));
#28413=CARTESIAN_POINT('Ctrl Pts',(163.274204949786,16.8279835131639,3.06773462333517));
#28414=CARTESIAN_POINT('Ctrl Pts',(163.391898776269,13.3722439005881,10.6665420135521));
#28415=CARTESIAN_POINT('Ctrl Pts',(163.509592602752,6.73175719848808,15.7249950652666));
#28416=CARTESIAN_POINT('Ctrl Pts',(163.627286429235,-1.51197141403623,17.0383674997955));
#28417=CARTESIAN_POINT('Ctrl Pts',(163.744980255719,-9.39560767951175,14.2938652721985));
#28418=CARTESIAN_POINT('Ctrl Pts',(163.862674082202,-15.0415760162977,8.14512168035195));
#28419=CARTESIAN_POINT('Ctrl Pts',(163.980367908685,-17.1052287046836,0.0565278839563854));
#28420=CARTESIAN_POINT('Ctrl Pts',(164.098061735168,-15.0950805326928,-8.04552894975068));
#28421=CARTESIAN_POINT('Ctrl Pts',(164.215755561651,-9.48987782598886,-14.2314539225157));
#28422=CARTESIAN_POINT('Ctrl Pts',(164.333449388134,-1.62454606293885,-17.0280028132521));
#28423=CARTESIAN_POINT('Ctrl Pts',(164.451143214618,6.62766822942697,-15.7691428839178));
#28424=CARTESIAN_POINT('Ctrl Pts',(164.568837041101,13.3014734656906,-10.754693373019));
#28425=CARTESIAN_POINT('Ctrl Pts',(164.686530867584,16.8072981115472,-3.17888441199923));
#28426=CARTESIAN_POINT('Ctrl Pts',(164.804224694067,16.3104609706914,5.15398850889241));
#28427=CARTESIAN_POINT('Ctrl Pts',(164.92191852055,11.9287363733997,12.2594281650536));
#28428=CARTESIAN_POINT('Ctrl Pts',(165.039612347034,4.70681762497127,16.4450537503718));
#28429=CARTESIAN_POINT('Ctrl Pts',(165.157306173517,-3.63765716981974,16.714298405546));
#28430=CARTESIAN_POINT('Ctrl Pts',(165.235768724506,-8.620294072214,14.2392607093337));
#28431=CARTESIAN_POINT('Ctrl Pts',(165.275,-10.6720568218315,12.4855047231419));
#28432=CARTESIAN_POINT('Ctrl Pts',(149.669351500835,9.36921550306818,-13.1405412628083));
#28433=CARTESIAN_POINT('Ctrl Pts',(149.708582776329,11.5286214438524,-11.6008832522912));
#28434=CARTESIAN_POINT('Ctrl Pts',(149.787045327318,15.0718489464266,-7.43816894232811));
#28435=CARTESIAN_POINT('Ctrl Pts',(149.904739153801,16.7970987434091,0.581624345890556));
#28436=CARTESIAN_POINT('Ctrl Pts',(150.022432980285,14.5217411515898,8.46135011476401));
#28437=CARTESIAN_POINT('Ctrl Pts',(150.140126806768,8.78796110611117,14.3266651495927));
#28438=CARTESIAN_POINT('Ctrl Pts',(150.257820633251,0.96118681584472,16.7795619622608));
#28439=CARTESIAN_POINT('Ctrl Pts',(150.375514459734,-7.09448295467532,15.2363995248823));
#28440=CARTESIAN_POINT('Ctrl Pts',(150.493208286218,-13.4605341461659,10.064434093448));
#28441=CARTESIAN_POINT('Ctrl Pts',(150.610902112701,-16.6208058548148,2.49555525516348));
#28442=CARTESIAN_POINT('Ctrl Pts',(150.728595939184,-15.8226522856942,-5.66768815398822));
#28443=CARTESIAN_POINT('Ctrl Pts',(150.846289765667,-11.2561587468171,-12.481099210543));
#28444=CARTESIAN_POINT('Ctrl Pts',(150.96398359215,-4.00888774708244,-16.3220040601612));
#28445=CARTESIAN_POINT('Ctrl Pts',(151.081677418633,4.19314427208089,-16.2756416585466));
#28446=CARTESIAN_POINT('Ctrl Pts',(151.199371245117,11.3965327025307,-12.353057276638));
#28447=CARTESIAN_POINT('Ctrl Pts',(151.3170650716,15.8857115407531,-5.48845581303432));
#28448=CARTESIAN_POINT('Ctrl Pts',(151.434758898083,16.5915333478769,2.68328151621556));
#28449=CARTESIAN_POINT('Ctrl Pts',(151.552452724566,13.3458989445182,10.215965962637));
#28450=CARTESIAN_POINT('Ctrl Pts',(151.670146551049,6.92179185172581,15.3156056408121));
#28451=CARTESIAN_POINT('Ctrl Pts',(151.787840377533,-1.15081612858479,16.7676653468417));
#28452=CARTESIAN_POINT('Ctrl Pts',(151.905534204016,-8.94934458710798,14.2263210366986));
#28453=CARTESIAN_POINT('Ctrl Pts',(152.023228030499,-14.6164881597404,8.2968218440555));
#28454=CARTESIAN_POINT('Ctrl Pts',(152.140921856982,-16.8025542492592,0.391343233840468));
#28455=CARTESIAN_POINT('Ctrl Pts',(152.258615683465,-14.9869071620209,-7.6073380717347));
#28456=CARTESIAN_POINT('Ctrl Pts',(152.376309509948,-9.60196323013091,-13.7942481112521));
#28457=CARTESIAN_POINT('Ctrl Pts',(152.494003336432,-1.93020610249092,-16.6959061816011));
#28458=CARTESIAN_POINT('Ctrl Pts',(152.611697162915,6.20125084689959,-15.6212504864081));
#28459=CARTESIAN_POINT('Ctrl Pts',(152.729390989398,12.8558116734326,-10.8262221038362));
#28460=CARTESIAN_POINT('Ctrl Pts',(152.847084815881,16.4486194947039,-3.45280980406319));
#28461=CARTESIAN_POINT('Ctrl Pts',(152.964778642364,16.1240075956589,4.74292714257176));
#28462=CARTESIAN_POINT('Ctrl Pts',(153.082472468848,11.9592858718244,11.8090838027562));
#28463=CARTESIAN_POINT('Ctrl Pts',(153.200166295331,4.94632862705181,16.0627772174616));
#28464=CARTESIAN_POINT('Ctrl Pts',(153.317860121814,-3.24465120575843,16.4909434956746));
#28465=CARTESIAN_POINT('Ctrl Pts',(153.435553948297,-10.6628816523304,12.9916101270386));
#28466=CARTESIAN_POINT('Ctrl Pts',(153.55324777478,-15.5416295074474,6.39818185720075));
#28467=CARTESIAN_POINT('Ctrl Pts',(153.670941601263,-16.7189672875137,-1.71904382248367));
#28468=CARTESIAN_POINT('Ctrl Pts',(153.788635427747,-13.9144990457088,-9.42686030083935));
#28469=CARTESIAN_POINT('Ctrl Pts',(153.90632925423,-7.79613975197862,-14.8895662728029));
#28470=CARTESIAN_POINT('Ctrl Pts',(154.024023080713,0.178956006267607,-16.8061582038369));
#28471=CARTESIAN_POINT('Ctrl Pts',(154.141716907196,8.11143142253025,-14.7201786368971));
#28472=CARTESIAN_POINT('Ctrl Pts',(154.25941073368,14.1120801937138,-9.12842655832674));
#28473=CARTESIAN_POINT('Ctrl Pts',(154.377104560162,16.7517817885471,-1.36263925287367));
#28474=CARTESIAN_POINT('Ctrl Pts',(154.494798386646,15.4018622270234,6.72767558406047));
#28475=CARTESIAN_POINT('Ctrl Pts',(154.612492213129,10.383819706171,13.2157204546066));
#28476=CARTESIAN_POINT('Ctrl Pts',(154.730186039612,2.89275626691932,16.5562960835077));
#28477=CARTESIAN_POINT('Ctrl Pts',(154.847879866095,-5.28724890691117,15.9538076276774));
#28478=CARTESIAN_POINT('Ctrl Pts',(154.965573692579,-12.2080375768375,11.5517443421804));
#28479=CARTESIAN_POINT('Ctrl Pts',(155.083267519062,-16.2213477702083,4.39850603529533));
#28480=CARTESIAN_POINT('Ctrl Pts',(155.200961345545,-16.3713655051676,-3.80228488159183));
#28481=CARTESIAN_POINT('Ctrl Pts',(155.318655172028,-12.6223624074577,-11.0975198165794));
#28482=CARTESIAN_POINT('Ctrl Pts',(155.436348998512,-5.86720481587589,-15.7497582988799));
#28483=CARTESIAN_POINT('Ctrl Pts',(155.554042824994,2.28529216070807,-16.6510185443647));
#28484=CARTESIAN_POINT('Ctrl Pts',(155.671736651478,9.89352166366411,-13.5866555088138));
#28485=CARTESIAN_POINT('Ctrl Pts',(155.789430477961,15.1455001218973,-7.28648096698123));
#28486=CARTESIAN_POINT('Ctrl Pts',(155.907124304444,16.7904110769446,0.74904919183636));
#28487=CARTESIAN_POINT('Ctrl Pts',(156.024818130927,14.4365008855564,8.60618504367071));
#28488=CARTESIAN_POINT('Ctrl Pts',(156.142511957411,8.64437916038609,14.413663231672));
#28489=CARTESIAN_POINT('Ctrl Pts',(156.260205783894,0.793503422229031,16.7883689244513));
#28490=CARTESIAN_POINT('Ctrl Pts',(156.377899610377,-7.24635388701869,15.1647398318818));
#28491=CARTESIAN_POINT('Ctrl Pts',(156.49559343686,-13.5604122849012,9.92946108749472));
#28492=CARTESIAN_POINT('Ctrl Pts',(156.613287263343,-16.6449092890366,2.32937192915047));
#28493=CARTESIAN_POINT('Ctrl Pts',(156.730981089826,-15.765237998514,-5.8254827846953));
#28494=CARTESIAN_POINT('Ctrl Pts',(156.84867491631,-11.1309018103816,-12.5929346743409));
#28495=CARTESIAN_POINT('Ctrl Pts',(156.966368742793,-3.84561888042886,-16.361240608556));
#28496=CARTESIAN_POINT('Ctrl Pts',(157.084062569276,4.35554050005972,-16.2329370656364));
#28497=CARTESIAN_POINT('Ctrl Pts',(157.201756395759,11.5193799855214,-12.2385809460795));
#28498=CARTESIAN_POINT('Ctrl Pts',(157.319450222242,15.9397523772454,-5.32947211050702));
#28499=CARTESIAN_POINT('Ctrl Pts',(157.437144048726,16.5638973518458,2.84890914949683));
#28500=CARTESIAN_POINT('Ctrl Pts',(157.554837875209,13.2431679160219,10.3487913483953));
#28501=CARTESIAN_POINT('Ctrl Pts',(157.672531701692,6.76843232360655,15.3839950177231));
#28502=CARTESIAN_POINT('Ctrl Pts',(157.790225528175,-1.31827990117477,16.755331000214));
#28503=CARTESIAN_POINT('Ctrl Pts',(157.907919354658,-9.0910292621774,14.1362005425364));
#28504=CARTESIAN_POINT('Ctrl Pts',(158.025613181142,-14.6986499738657,8.15037838203533));
#28505=CARTESIAN_POINT('Ctrl Pts',(158.143307007625,-16.8056254619089,0.223453929507307));
#28506=CARTESIAN_POINT('Ctrl Pts',(158.261000834108,-14.9101563303303,-7.75668853504396));
#28507=CARTESIAN_POINT('Ctrl Pts',(158.378694660591,-9.46366940906519,-13.8894902764823));
#28508=CARTESIAN_POINT('Ctrl Pts',(158.496388487074,-1.76330548726561,-16.7143570795634));
#28509=CARTESIAN_POINT('Ctrl Pts',(158.614082313557,6.35700903835122,-15.5585158325238));
#28510=CARTESIAN_POINT('Ctrl Pts',(158.731776140041,12.9633319139634,-10.6972428463128));
#28511=CARTESIAN_POINT('Ctrl Pts',(158.849469966524,16.4822946559695,-3.28830377221617));
#28512=CARTESIAN_POINT('Ctrl Pts',(158.967163793007,16.0758175674659,4.90378102713882));
#28513=CARTESIAN_POINT('Ctrl Pts',(159.08485761949,11.8407076396336,11.927976417536));
#28514=CARTESIAN_POINT('Ctrl Pts',(159.202551445973,4.78560290160023,16.1113929780379));
#28515=CARTESIAN_POINT('Ctrl Pts',(159.320245272457,-3.40924582445485,16.4577040237394));
#28516=CARTESIAN_POINT('Ctrl Pts',(159.43793909894,-10.7921451447597,12.8844317685729));
#28517=CARTESIAN_POINT('Ctrl Pts',(159.555632925423,-15.6047763505738,6.2425903175801));
#28518=CARTESIAN_POINT('Ctrl Pts',(159.673326751906,-16.7009583658286,-1.88599270609223));
#28519=CARTESIAN_POINT('Ctrl Pts',(159.791020578389,-13.8196233820674,-9.56540581483018));
#28520=CARTESIAN_POINT('Ctrl Pts',(159.908714404873,-7.64699302961428,-14.9667122785735));
#28521=CARTESIAN_POINT('Ctrl Pts',(160.026408231356,0.346852854330788,-16.803531531259));
#28522=CARTESIAN_POINT('Ctrl Pts',(160.144102057839,8.25809191452131,-14.638404856947));
#28523=CARTESIAN_POINT('Ctrl Pts',(160.261795884322,14.2025755197285,-8.98698099647384));
#28524=CARTESIAN_POINT('Ctrl Pts',(160.379489710805,16.7645594909558,-1.19520872602881));
#28525=CARTESIAN_POINT('Ctrl Pts',(160.497183537289,15.3338791554016,6.88121565365554));
#28526=CARTESIAN_POINT('Ctrl Pts',(160.614877363772,10.2512667770577,13.3188028099438));
#28527=CARTESIAN_POINT('Ctrl Pts',(160.732571190255,2.72720241889082,16.5843705274264));
#28528=CARTESIAN_POINT('Ctrl Pts',(160.850265016738,-5.44637520332267,15.9001879224494));
#28529=CARTESIAN_POINT('Ctrl Pts',(160.967958843221,-12.3228386432412,11.4292006105945));
#28530=CARTESIAN_POINT('Ctrl Pts',(161.085652669705,-16.2644824694596,4.23622341540371));
#28531=CARTESIAN_POINT('Ctrl Pts',(161.203346496188,-16.3325608340194,-3.96565699823196));
#28532=CARTESIAN_POINT('Ctrl Pts',(161.321040322671,-12.5108601253202,-11.223072562772));
#28533=CARTESIAN_POINT('Ctrl Pts',(161.438734149154,-5.70956041812335,-15.8075899066357));
#28534=CARTESIAN_POINT('Ctrl Pts',(161.556427975637,2.45153392615592,-16.6273557799633));
#28535=CARTESIAN_POINT('Ctrl Pts',(161.674121802121,10.0287684911728,-13.4871339199638));
#28536=CARTESIAN_POINT('Ctrl Pts',(161.791815628603,15.2175414913454,-7.13480271512424));
#28537=CARTESIAN_POINT('Ctrl Pts',(161.909509455087,16.7820895435127,0.916760262072329));
#28538=CARTESIAN_POINT('Ctrl Pts',(162.02720328157,14.3497983139923,8.74998669554875));
#28539=CARTESIAN_POINT('Ctrl Pts',(162.144897108053,8.49994472212025,14.4993075195166));
#28540=CARTESIAN_POINT('Ctrl Pts',(162.262590934536,0.625735767965398,16.7954587187512));
#28541=CARTESIAN_POINT('Ctrl Pts',(162.38028476102,-7.39749904440972,15.0915866201111));
#28542=CARTESIAN_POINT('Ctrl Pts',(162.497978587503,-13.6589380631546,9.79348711196305));
#28543=CARTESIAN_POINT('Ctrl Pts',(162.615672413986,-16.6673506898589,2.16296088826871));
#28544=CARTESIAN_POINT('Ctrl Pts',(162.733366240469,-15.7062503555818,-5.9826982704592));
#28545=CARTESIAN_POINT('Ctrl Pts',(162.851060066952,-11.0045336794823,-12.70351200723));
#28546=CARTESIAN_POINT('Ctrl Pts',(162.968753893435,-3.68196622327458,-16.3988445799281));
#28547=CARTESIAN_POINT('Ctrl Pts',(163.086447719919,4.51750200427417,-16.1886118761679));
#28548=CARTESIAN_POINT('Ctrl Pts',(163.204141546402,11.6410774187547,-12.1228831269039));
#28549=CARTESIAN_POINT('Ctrl Pts',(163.321835372885,15.9922021643325,-5.16995637124805));
#28550=CARTESIAN_POINT('Ctrl Pts',(163.439529199368,16.5346079832404,3.0142523822763));
#28551=CARTESIAN_POINT('Ctrl Pts',(163.557223025851,13.1391150092071,10.4805837605487));
#28552=CARTESIAN_POINT('Ctrl Pts',(163.674916852335,6.61439715746602,15.4508488042657));
#28553=CARTESIAN_POINT('Ctrl Pts',(163.792610678818,-1.48561202198696,16.7413241796393));
#28554=CARTESIAN_POINT('Ctrl Pts',(163.910304505301,-9.2318066287338,14.0446690274074));
#28555=CARTESIAN_POINT('Ctrl Pts',(164.027998331784,-14.7793443394474,8.00312133982417));
#28556=CARTESIAN_POINT('Ctrl Pts',(164.145692158267,-16.8070197403253,0.0555423887009042));
#28557=CARTESIAN_POINT('Ctrl Pts',(164.26338598475,-14.831916069342,-7.90526488796918));
#28558=CARTESIAN_POINT('Ctrl Pts',(164.381079811234,-9.32443328927823,-13.9833457440858));
#28559=CARTESIAN_POINT('Ctrl Pts',(164.498773637717,-1.59622406810641,-16.7311401888639));
#28560=CARTESIAN_POINT('Ctrl Pts',(164.6164674642,6.51212285362811,-15.4942269591197));
#28561=CARTESIAN_POINT('Ctrl Pts',(164.734161290683,13.0695783712066,-10.5671983077305));
#28562=CARTESIAN_POINT('Ctrl Pts',(164.851855117166,16.5142832065705,-3.1234644088713));
#28563=CARTESIAN_POINT('Ctrl Pts',(164.96954894365,16.0261078200699,5.06413495580132));
#28564=CARTESIAN_POINT('Ctrl Pts',(165.087242770133,11.7207732890452,12.0456998694637));
#28565=CARTESIAN_POINT('Ctrl Pts',(165.204936596616,4.62475995514413,16.1583541375));
#28566=CARTESIAN_POINT('Ctrl Pts',(165.322630423099,-3.57423901879522,16.4229048379096));
#28567=CARTESIAN_POINT('Ctrl Pts',(165.401092974088,-8.47000967601441,13.9910164290221));
#28568=CARTESIAN_POINT('Ctrl Pts',(165.440324249582,-10.486002424819,12.2678350563248));
#28569=CARTESIAN_POINT('Ctrl Pts',(149.834675750418,9.20297639017438,-12.9073870652388));
#28570=CARTESIAN_POINT('Ctrl Pts',(149.873907025912,11.3240677327026,-11.395047391219));
#28571=CARTESIAN_POINT('Ctrl Pts',(149.952369576901,14.8044273252991,-7.30619261985777));
#28572=CARTESIAN_POINT('Ctrl Pts',(150.070063403384,16.4990658084874,0.571304515455822));
#28573=CARTESIAN_POINT('Ctrl Pts',(150.187757229867,14.2640801589567,8.3112193661969));
#28574=CARTESIAN_POINT('Ctrl Pts',(150.30545105635,8.63203525960385,14.0724654138288));
#28575=CARTESIAN_POINT('Ctrl Pts',(150.423144882833,0.944132363042452,16.4818401845475));
#28576=CARTESIAN_POINT('Ctrl Pts',(150.540838709317,-6.96860469384984,14.9660582631318));
#28577=CARTESIAN_POINT('Ctrl Pts',(150.6585325358,-13.221702276539,9.88585963383337));
#28578=CARTESIAN_POINT('Ctrl Pts',(150.776226362283,-16.3259009057313,2.45127631935929));
#28579=CARTESIAN_POINT('Ctrl Pts',(150.893920188766,-15.5419090709886,-5.5671256842095));
#28580=CARTESIAN_POINT('Ctrl Pts',(151.011614015249,-11.0564393739357,-12.2596455722933));
#28581=CARTESIAN_POINT('Ctrl Pts',(151.129307841733,-3.93775757161068,-16.03240078711));
#28582=CARTESIAN_POINT('Ctrl Pts',(151.247001668216,4.11874481101629,-15.9868609991405));
#28583=CARTESIAN_POINT('Ctrl Pts',(151.364695494699,11.1943226577395,-12.1338755017581));
#28584=CARTESIAN_POINT('Ctrl Pts',(151.482389321182,15.6038494581319,-5.39107348414916));
#28585=CARTESIAN_POINT('Ctrl Pts',(151.600083147665,16.2971477843902,2.63567173087615));
#28586=CARTESIAN_POINT('Ctrl Pts',(151.717776974149,13.1091010610049,10.0347028549172));
#28587=CARTESIAN_POINT('Ctrl Pts',(151.835470800632,6.79897766982448,15.0438590154596));
#28588=CARTESIAN_POINT('Ctrl Pts',(151.953164627115,-1.13039706017324,16.4701546522007));
#28589=CARTESIAN_POINT('Ctrl Pts',(152.070858453598,-8.79055529416723,13.9739017185488));
#28590=CARTESIAN_POINT('Ctrl Pts',(152.188552280082,-14.3571460595931,8.14961034030235));
#28591=CARTESIAN_POINT('Ctrl Pts',(152.306246106564,-16.5044245166437,0.384399583968249));
#28592=CARTESIAN_POINT('Ctrl Pts',(152.423939933048,-14.7209926731482,-7.47236016113865));
#28593=CARTESIAN_POINT('Ctrl Pts',(152.541633759531,-9.43159444643784,-13.5494951147712));
#28594=CARTESIAN_POINT('Ctrl Pts',(152.659327586014,-1.89595822441881,-16.3996687184241));
#28595=CARTESIAN_POINT('Ctrl Pts',(152.777021412497,6.09122131035165,-15.3440807679507));
#28596=CARTESIAN_POINT('Ctrl Pts',(152.89471523898,12.6277094670717,-10.6341311483081));
#28597=CARTESIAN_POINT('Ctrl Pts',(153.012409065464,16.156769668832,-3.39154618614015));
#28598=CARTESIAN_POINT('Ctrl Pts',(153.130102891947,15.8379173975929,4.65877281818433));
#28599=CARTESIAN_POINT('Ctrl Pts',(153.24779671843,11.7470908301451,11.5995538143793));
#28600=CARTESIAN_POINT('Ctrl Pts',(153.365490544913,4.85856532576227,15.77777343733));
#28601=CARTESIAN_POINT('Ctrl Pts',(153.483184371396,-3.18708097077789,16.1983427099839));
#28602=CARTESIAN_POINT('Ctrl Pts',(153.60087819788,-10.4736888659979,12.7610984324496));
#28603=CARTESIAN_POINT('Ctrl Pts',(153.718572024363,-15.2658725135565,6.28465815014907));
#28604=CARTESIAN_POINT('Ctrl Pts',(153.836265850846,-16.4223206483723,-1.6885426220383));
#28605=CARTESIAN_POINT('Ctrl Pts',(153.953959677329,-13.6676124224945,-9.25959838939414));
#28606=CARTESIAN_POINT('Ctrl Pts',(154.071653503812,-7.65781191055575,-14.6253789149869));
#28607=CARTESIAN_POINT('Ctrl Pts',(154.189347330296,0.175780768413483,-16.5079645258236));
#28608=CARTESIAN_POINT('Ctrl Pts',(154.307041156779,7.9675093232319,-14.4589967441938));
#28609=CARTESIAN_POINT('Ctrl Pts',(154.424734983262,13.8616878645245,-8.96645979252062));
#28610=CARTESIAN_POINT('Ctrl Pts',(154.542428809745,16.4545529177835,-1.33846178139616));
#28611=CARTESIAN_POINT('Ctrl Pts',(154.660122636228,15.12858514073,6.60830563034714));
#28612=CARTESIAN_POINT('Ctrl Pts',(154.777816462711,10.1995783493746,12.9812323436322));
#28613=CARTESIAN_POINT('Ctrl Pts',(154.895510289195,2.84142974598773,16.2625357390233));
#28614=CARTESIAN_POINT('Ctrl Pts',(155.013204115678,-5.19343661626147,15.6707373080295));
#28615=CARTESIAN_POINT('Ctrl Pts',(155.130897942161,-11.9914289038613,11.3467803586759));
#28616=CARTESIAN_POINT('Ctrl Pts',(155.248591768644,-15.9335304537662,4.32046281586825));
#28617=CARTESIAN_POINT('Ctrl Pts',(155.366285595128,-16.0808864060852,-3.73482048550892));
#28618=CARTESIAN_POINT('Ctrl Pts',(155.483979421611,-12.3984023193849,-10.9006151932387));
#28619=CARTESIAN_POINT('Ctrl Pts',(155.601673248094,-5.76310229806762,-15.4703084509134));
#28620=CARTESIAN_POINT('Ctrl Pts',(155.719367074577,2.24474394817366,-16.3555775279118));
#28621=CARTESIAN_POINT('Ctrl Pts',(155.83706090106,9.71797972376269,-13.3455858527429));
#28622=CARTESIAN_POINT('Ctrl Pts',(155.954754727543,14.8767716991417,-7.15719606242632));
#28623=CARTESIAN_POINT('Ctrl Pts',(156.072448554027,16.4924968020899,0.735758722306252));
#28624=CARTESIAN_POINT('Ctrl Pts',(156.19014238051,14.1803523211734,8.45348447161203));
#28625=CARTESIAN_POINT('Ctrl Pts',(156.307836206993,8.49100090553969,14.1579198785174));
#28626=CARTESIAN_POINT('Ctrl Pts',(156.425530033476,0.77942419596441,16.490490883753));
#28627=CARTESIAN_POINT('Ctrl Pts',(156.543223859959,-7.1177809620499,14.8956700366474));
#28628=CARTESIAN_POINT('Ctrl Pts',(156.660917686442,-13.3198082654956,9.75328147009152));
#28629=CARTESIAN_POINT('Ctrl Pts',(156.778611512926,-16.3495766698327,2.28804160400477));
#28630=CARTESIAN_POINT('Ctrl Pts',(156.896305339409,-15.4855134923828,-5.72212054588366));
#28631=CARTESIAN_POINT('Ctrl Pts',(157.013999165892,-10.9334048863264,-12.3694967260616));
#28632=CARTESIAN_POINT('Ctrl Pts',(157.131692992375,-3.7773856040141,-16.070941156727));
#28633=CARTESIAN_POINT('Ctrl Pts',(157.249386818858,4.27825962327065,-15.9449141189373));
#28634=CARTESIAN_POINT('Ctrl Pts',(157.367080645342,11.3149902466737,-12.0214303384444));
#28635=CARTESIAN_POINT('Ctrl Pts',(157.484774471825,15.6569314415894,-5.23491064849851));
#28636=CARTESIAN_POINT('Ctrl Pts',(157.602468298308,16.2700021371469,2.79836061322161));
#28637=CARTESIAN_POINT('Ctrl Pts',(157.720162124791,13.008192801452,10.1651715039466));
#28638=CARTESIAN_POINT('Ctrl Pts',(157.837855951274,6.64833921818169,15.1110349514645));
#28639=CARTESIAN_POINT('Ctrl Pts',(157.955549777758,-1.29488950298773,16.4580391553625));
#28640=CARTESIAN_POINT('Ctrl Pts',(158.073243604241,-8.92972604107625,13.8853802431089));
#28641=CARTESIAN_POINT('Ctrl Pts',(158.190937430724,-14.4378500668093,8.00576524216949));
#28642=CARTESIAN_POINT('Ctrl Pts',(158.308631257207,-16.5074412363995,0.219489159671254));
#28643=CARTESIAN_POINT('Ctrl Pts',(158.426325083691,-14.6456036406574,-7.61906068128856));
#28644=CARTESIAN_POINT('Ctrl Pts',(158.544018910173,-9.29575438920379,-13.6430473868558));
#28645=CARTESIAN_POINT('Ctrl Pts',(158.661712736657,-1.73201894680041,-16.4177922398939));
#28646=CARTESIAN_POINT('Ctrl Pts',(158.77940656314,6.24421586555601,-15.2824592225444));
#28647=CARTESIAN_POINT('Ctrl Pts',(158.897100389623,12.7333219630962,-10.5074403851997));
#28648=CARTESIAN_POINT('Ctrl Pts',(159.014794216106,16.1898473276777,-3.22995900452034));
#28649=CARTESIAN_POINT('Ctrl Pts',(159.13248804259,15.7905824108423,4.81677265301081));
#28650=CARTESIAN_POINT('Ctrl Pts',(159.250181869073,11.6306165457311,11.7163369032544));
#28651=CARTESIAN_POINT('Ctrl Pts',(159.367875695556,4.70069137610872,15.8255266026433));
#28652=CARTESIAN_POINT('Ctrl Pts',(159.485569522039,-3.34875516744001,16.1656930099807));
#28653=CARTESIAN_POINT('Ctrl Pts',(159.603263348522,-10.6006588207982,12.6558217524358));
#28654=CARTESIAN_POINT('Ctrl Pts',(159.720957175005,-15.3278989346817,6.13182728985231));
#28655=CARTESIAN_POINT('Ctrl Pts',(159.838651001489,-16.4046312611417,-1.85252931160823));
#28656=CARTESIAN_POINT('Ctrl Pts',(159.956344827972,-13.574420149117,-9.39568567373559));
#28657=CARTESIAN_POINT('Ctrl Pts',(160.074038654455,-7.51131151635076,-14.7011561099368));
#28658=CARTESIAN_POINT('Ctrl Pts',(160.191732480938,0.34069860259118,-16.5053844586119));
#28659=CARTESIAN_POINT('Ctrl Pts',(160.309426307421,8.11156760054691,-14.3786738862161));
#28660=CARTESIAN_POINT('Ctrl Pts',(160.427120133905,13.9505775211304,-8.8275239162137));
#28661=CARTESIAN_POINT('Ctrl Pts',(160.544813960388,16.4671039038878,-1.17400199444354));
#28662=CARTESIAN_POINT('Ctrl Pts',(160.662507786871,15.0618083008908,6.75912142009672));
#28663=CARTESIAN_POINT('Ctrl Pts',(160.780201613354,10.0693773227594,13.0824856963917));
#28664=CARTESIAN_POINT('Ctrl Pts',(160.897895439837,2.67881333971445,16.2901120547209));
#28665=CARTESIAN_POINT('Ctrl Pts',(161.01558926632,-5.34973951573596,15.6180689836538));
#28666=CARTESIAN_POINT('Ctrl Pts',(161.133283092804,-12.1041930411931,11.2264109351977));
#28667=CARTESIAN_POINT('Ctrl Pts',(161.250976919287,-15.975899808882,4.16105959593918));
#28668=CARTESIAN_POINT('Ctrl Pts',(161.36867074577,-16.0427702508652,-3.89529387111515));
#28669=CARTESIAN_POINT('Ctrl Pts',(161.486364572253,-12.2888784355949,-11.0239402420172));
#28670=CARTESIAN_POINT('Ctrl Pts',(161.604058398736,-5.60825500374669,-15.5271139455259));
#28671=CARTESIAN_POINT('Ctrl Pts',(161.72175222522,2.40803606606511,-16.3323346147733));
#28672=CARTESIAN_POINT('Ctrl Pts',(161.839446051703,9.85082685061131,-13.2478300873643));
#28673=CARTESIAN_POINT('Ctrl Pts',(161.957139878186,14.9475348299427,-7.00820905595969));
#28674=CARTESIAN_POINT('Ctrl Pts',(162.074833704669,16.4843229186225,0.900494074934982));
#28675=CARTESIAN_POINT('Ctrl Pts',(162.192527531152,14.0951881237216,8.59473463355657));
#28676=CARTESIAN_POINT('Ctrl Pts',(162.310221357636,8.34912918481203,14.2420445695044));
#28677=CARTESIAN_POINT('Ctrl Pts',(162.427915184119,0.614633263285196,16.4974548829834));
#28678=CARTESIAN_POINT('Ctrl Pts',(162.545609010602,-7.26624433280952,14.8238147910752));
#28679=CARTESIAN_POINT('Ctrl Pts',(162.663302837085,-13.4165858890642,9.61972009709434));
#28680=CARTESIAN_POINT('Ctrl Pts',(162.780996663568,-16.3716198901922,2.12458321415372));
#28681=CARTESIAN_POINT('Ctrl Pts',(162.898690490051,-15.4275724742645,-5.87654653845276));
#28682=CARTESIAN_POINT('Ctrl Pts',(163.016384316535,-10.8092789203097,-12.4781120720886));
#28683=CARTESIAN_POINT('Ctrl Pts',(163.134078143018,-3.61663665555766,-16.1078779163309));
#28684=CARTESIAN_POINT('Ctrl Pts',(163.251771969501,4.43734742511645,-15.9013753966148));
#28685=CARTESIAN_POINT('Ctrl Pts',(163.369465795984,11.4345283877725,-11.9077853595324));
#28686=CARTESIAN_POINT('Ctrl Pts',(163.487159622467,15.7084506058219,-5.07822521610762));
#28687=CARTESIAN_POINT('Ctrl Pts',(163.604853448951,16.2412324533168,2.96077014121744));
#28688=CARTESIAN_POINT('Ctrl Pts',(163.722547275434,12.9059861178261,10.2946255075453));
#28689=CARTESIAN_POINT('Ctrl Pts',(163.840241101917,6.49703711644397,15.1767025432649));
#28690=CARTESIAN_POINT('Ctrl Pts',(163.9579349284,-1.45925262993771,16.444280859483));
#28691=CARTESIAN_POINT('Ctrl Pts',(164.075628754883,-9.06800557795583,13.7954727826163));
#28692=CARTESIAN_POINT('Ctrl Pts',(164.193322581366,-14.517112662597,7.86112099929637));
#28693=CARTESIAN_POINT('Ctrl Pts',(164.31101640785,-16.5088107759669,0.0545568934454388));
#28694=CARTESIAN_POINT('Ctrl Pts',(164.428710234333,-14.5687516059912,-7.7650008261877));
#28695=CARTESIAN_POINT('Ctrl Pts',(164.546404060816,-9.15898875256761,-13.7352375656558));
#28696=CARTESIAN_POINT('Ctrl Pts',(164.664097887299,-1.56790207327398,-16.4342775644758));
#28697=CARTESIAN_POINT('Ctrl Pts',(164.781791713783,6.39657747782926,-15.2193110343215));
#28698=CARTESIAN_POINT('Ctrl Pts',(164.899485540266,12.8376832767225,-10.379703242442));
#28699=CARTESIAN_POINT('Ctrl Pts',(165.017179366749,16.2212683015939,-3.06804440574336));
#28700=CARTESIAN_POINT('Ctrl Pts',(165.134873193232,15.7417546694485,4.97428140271022));
#28701=CARTESIAN_POINT('Ctrl Pts',(165.252567019715,11.5128102046906,11.8319715738739));
#28702=CARTESIAN_POINT('Ctrl Pts',(165.370260846199,4.542702285317,15.8716545246283));
#28703=CARTESIAN_POINT('Ctrl Pts',(165.487954672682,-3.51082086777072,16.1315112702732));
#28704=CARTESIAN_POINT('Ctrl Pts',(165.56641722367,-8.31972527981482,13.7427721487105));
#28705=CARTESIAN_POINT('Ctrl Pts',(165.605648499165,-10.2999480278064,12.0501653895076));
#28706=CARTESIAN_POINT('Ctrl Pts',(150.,9.03673727728059,-12.6742328676692));
#28707=CARTESIAN_POINT('Ctrl Pts',(150.039231275494,11.1195140215529,-11.1892115301467));
#28708=CARTESIAN_POINT('Ctrl Pts',(150.117693826483,14.5370057041716,-7.17421629738743));
#28709=CARTESIAN_POINT('Ctrl Pts',(150.235387652966,16.2010328735656,0.560984685021083));
#28710=CARTESIAN_POINT('Ctrl Pts',(150.35308147945,14.0064191663237,8.1610886176298));
#28711=CARTESIAN_POINT('Ctrl Pts',(150.470775305933,8.47610941309655,13.8182656780649));
#28712=CARTESIAN_POINT('Ctrl Pts',(150.588469132416,0.927077910240183,16.1841184068341));
#28713=CARTESIAN_POINT('Ctrl Pts',(150.706162958899,-6.84272643302437,14.6957170013813));
#28714=CARTESIAN_POINT('Ctrl Pts',(150.823856785382,-12.9828704069121,9.70728517421879));
#28715=CARTESIAN_POINT('Ctrl Pts',(150.941550611866,-16.0309959566478,2.40699738355509));
#28716=CARTESIAN_POINT('Ctrl Pts',(151.059244438349,-15.261165856283,-5.46656321443077));
#28717=CARTESIAN_POINT('Ctrl Pts',(151.176938264832,-10.8567200010544,-12.0381919340435));
#28718=CARTESIAN_POINT('Ctrl Pts',(151.294632091315,-3.86662739613892,-15.7427975140589));
#28719=CARTESIAN_POINT('Ctrl Pts',(151.412325917798,4.04434534995169,-15.6980803397344));
#28720=CARTESIAN_POINT('Ctrl Pts',(151.530019744281,10.9921126129483,-11.9146937268782));
#28721=CARTESIAN_POINT('Ctrl Pts',(151.647713570765,15.3219873755107,-5.293691155264));
#28722=CARTESIAN_POINT('Ctrl Pts',(151.765407397248,16.0027622209035,2.58806194553672));
#28723=CARTESIAN_POINT('Ctrl Pts',(151.883101223731,12.8723031774915,9.8534397471975));
#28724=CARTESIAN_POINT('Ctrl Pts',(152.000795050214,6.67616348792316,14.772112390107));
#28725=CARTESIAN_POINT('Ctrl Pts',(152.118488876698,-1.1099779917617,16.1726439575597));
#28726=CARTESIAN_POINT('Ctrl Pts',(152.23618270318,-8.63176600122648,13.7214824003989));
#28727=CARTESIAN_POINT('Ctrl Pts',(152.353876529664,-14.0978039594459,8.00239883654923));
#28728=CARTESIAN_POINT('Ctrl Pts',(152.471570356147,-16.2062947840282,0.377455934096013));
#28729=CARTESIAN_POINT('Ctrl Pts',(152.58926418263,-14.4550781842755,-7.33738225054259));
#28730=CARTESIAN_POINT('Ctrl Pts',(152.706958009113,-9.26122566274478,-13.3047421182903));
#28731=CARTESIAN_POINT('Ctrl Pts',(152.824651835596,-1.8617103463467,-16.1034312552471));
#28732=CARTESIAN_POINT('Ctrl Pts',(152.94234566208,5.98119177380371,-15.0669110494933));
#28733=CARTESIAN_POINT('Ctrl Pts',(153.060039488563,12.3996072607107,-10.44204019278));
#28734=CARTESIAN_POINT('Ctrl Pts',(153.177733315046,15.86491984296,-3.3302825682171));
#28735=CARTESIAN_POINT('Ctrl Pts',(153.295427141529,15.551827199527,4.5746184937969));
#28736=CARTESIAN_POINT('Ctrl Pts',(153.413120968012,11.5348957884658,11.3900238260024));
#28737=CARTESIAN_POINT('Ctrl Pts',(153.530814794496,4.77080202447272,15.4927696571985));
#28738=CARTESIAN_POINT('Ctrl Pts',(153.648508620979,-3.12951073579735,15.9057419242933));
#28739=CARTESIAN_POINT('Ctrl Pts',(153.766202447462,-10.2844960796655,12.5305867378607));
#28740=CARTESIAN_POINT('Ctrl Pts',(153.883896273945,-14.9901155196656,6.17113444309738));
#28741=CARTESIAN_POINT('Ctrl Pts',(154.001590100428,-16.1256740092309,-1.6580414215929));
#28742=CARTESIAN_POINT('Ctrl Pts',(154.119283926912,-13.4207257992801,-9.09233647794895));
#28743=CARTESIAN_POINT('Ctrl Pts',(154.236977753395,-7.51948406913288,-14.3611915571709));
#28744=CARTESIAN_POINT('Ctrl Pts',(154.354671579878,0.172605530559356,-16.2097708478104));
#28745=CARTESIAN_POINT('Ctrl Pts',(154.472365406361,7.82358722393355,-14.1978148514905));
#28746=CARTESIAN_POINT('Ctrl Pts',(154.590059232844,13.6112955353353,-8.80449302671448));
#28747=CARTESIAN_POINT('Ctrl Pts',(154.707753059327,16.1573240470198,-1.31428430991864));
#28748=CARTESIAN_POINT('Ctrl Pts',(154.825446885811,14.8553080544366,6.48893567663383));
#28749=CARTESIAN_POINT('Ctrl Pts',(154.943140712294,10.0153369925782,12.7467442326578));
#28750=CARTESIAN_POINT('Ctrl Pts',(155.060834538777,2.79010322505614,15.968775394539));
#28751=CARTESIAN_POINT('Ctrl Pts',(155.17852836526,-5.09962432561176,15.3876669883817));
#28752=CARTESIAN_POINT('Ctrl Pts',(155.296222191744,-11.7748202308851,11.1418163751715));
#28753=CARTESIAN_POINT('Ctrl Pts',(155.413916018227,-15.645713137324,4.24241959644116));
#28754=CARTESIAN_POINT('Ctrl Pts',(155.53160984471,-15.7904073070029,-3.66735608942599));
#28755=CARTESIAN_POINT('Ctrl Pts',(155.649303671193,-12.1744422313121,-10.703710569898));
#28756=CARTESIAN_POINT('Ctrl Pts',(155.766997497676,-5.65899978025936,-15.1908586029469));
#28757=CARTESIAN_POINT('Ctrl Pts',(155.884691324159,2.20419573563924,-16.0601365114588));
#28758=CARTESIAN_POINT('Ctrl Pts',(156.002385150643,9.54243778386128,-13.104516196672));
#28759=CARTESIAN_POINT('Ctrl Pts',(156.120078977126,14.6080432763861,-7.02791115787139));
#28760=CARTESIAN_POINT('Ctrl Pts',(156.237772803609,16.1945825272352,0.72246825277614));
#28761=CARTESIAN_POINT('Ctrl Pts',(156.355466630092,13.9242037567905,8.30078389955334));
#28762=CARTESIAN_POINT('Ctrl Pts',(156.473160456575,8.3376226506933,13.9021765253628));
#28763=CARTESIAN_POINT('Ctrl Pts',(156.590854283059,0.765344969699789,16.1926128430546));
#28764=CARTESIAN_POINT('Ctrl Pts',(156.708548109542,-6.9892080370811,14.626600241413));
#28765=CARTESIAN_POINT('Ctrl Pts',(156.826241936025,-13.0792042460899,9.5771018526883));
#28766=CARTESIAN_POINT('Ctrl Pts',(156.943935762508,-16.0542440506288,2.24671127885909));
#28767=CARTESIAN_POINT('Ctrl Pts',(157.061629588991,-15.2057889862516,-5.61875830707204));
#28768=CARTESIAN_POINT('Ctrl Pts',(157.179323415475,-10.7359079622712,-12.1460587777823));
#28769=CARTESIAN_POINT('Ctrl Pts',(157.297017241958,-3.70915232759935,-15.780641704898));
#28770=CARTESIAN_POINT('Ctrl Pts',(157.414711068441,4.20097874648159,-15.6568911722382));
#28771=CARTESIAN_POINT('Ctrl Pts',(157.532404894924,11.1106005078261,-11.8042797308094));
#28772=CARTESIAN_POINT('Ctrl Pts',(157.650098721407,15.3741105059335,-5.14034918648998));
#28773=CARTESIAN_POINT('Ctrl Pts',(157.76779254789,15.976106922448,2.74781207694638));
#28774=CARTESIAN_POINT('Ctrl Pts',(157.885486374374,12.7732176868821,9.98155165949782));
#28775=CARTESIAN_POINT('Ctrl Pts',(158.003180200857,6.52824611275682,14.8380748852059));
#28776=CARTESIAN_POINT('Ctrl Pts',(158.12087402734,-1.27149910480069,16.1607473105111));
#28777=CARTESIAN_POINT('Ctrl Pts',(158.238567853823,-8.76842281997508,13.6345599436814));
#28778=CARTESIAN_POINT('Ctrl Pts',(158.356261680306,-14.1770501597529,7.86115210230364));
#28779=CARTESIAN_POINT('Ctrl Pts',(158.47395550679,-16.20925701089,0.215524389835196));
#28780=CARTESIAN_POINT('Ctrl Pts',(158.591649333273,-14.3810509509845,-7.48143282753315));
#28781=CARTESIAN_POINT('Ctrl Pts',(158.709343159756,-9.12783936934241,-13.3966044972293));
#28782=CARTESIAN_POINT('Ctrl Pts',(158.827036986239,-1.70073240633521,-16.1212274002243));
#28783=CARTESIAN_POINT('Ctrl Pts',(158.944730812722,6.13142269276078,-15.0064026125651));
#28784=CARTESIAN_POINT('Ctrl Pts',(159.062424639206,12.503312012229,-10.3176379240867));
#28785=CARTESIAN_POINT('Ctrl Pts',(159.180118465689,15.8973999993859,-3.17161423682451));
#28786=CARTESIAN_POINT('Ctrl Pts',(159.297812292172,15.5053472542187,4.7297642788828));
#28787=CARTESIAN_POINT('Ctrl Pts',(159.415506118655,11.4205254518286,11.5046973889728));
#28788=CARTESIAN_POINT('Ctrl Pts',(159.533199945138,4.61577985061722,15.5396602272488));
#28789=CARTESIAN_POINT('Ctrl Pts',(159.650893771622,-3.28826451042518,15.8736819962219));
#28790=CARTESIAN_POINT('Ctrl Pts',(159.768587598105,-10.4091724968367,12.4272117362987));
#28791=CARTESIAN_POINT('Ctrl Pts',(159.886281424588,-15.0510215187897,6.02106426212451));
#28792=CARTESIAN_POINT('Ctrl Pts',(160.003975251071,-16.1083041564548,-1.81906591712422));
#28793=CARTESIAN_POINT('Ctrl Pts',(160.121669077554,-13.3292169161666,-9.22596553264098));
#28794=CARTESIAN_POINT('Ctrl Pts',(160.239362904037,-7.37563000308724,-14.4355999413));
#28795=CARTESIAN_POINT('Ctrl Pts',(160.357056730521,0.334544350851575,-16.2072373859648));
#28796=CARTESIAN_POINT('Ctrl Pts',(160.474750557004,7.96504328657251,-14.1189429154851));
#28797=CARTESIAN_POINT('Ctrl Pts',(160.592444383487,13.6985795225324,-8.66806683595355));
#28798=CARTESIAN_POINT('Ctrl Pts',(160.71013820997,16.1696483168198,-1.15279526285827));
#28799=CARTESIAN_POINT('Ctrl Pts',(160.827832036453,14.7897374463801,6.6370271865379));
#28800=CARTESIAN_POINT('Ctrl Pts',(160.945525862937,9.88748786846115,12.8461685828396));
#28801=CARTESIAN_POINT('Ctrl Pts',(161.06321968942,2.63042426053809,15.9958535820154));
#28802=CARTESIAN_POINT('Ctrl Pts',(161.180913515903,-5.25310382814925,15.3359500448582));
#28803=CARTESIAN_POINT('Ctrl Pts',(161.298607342386,-11.8855474391451,11.0236212598008));
#28804=CARTESIAN_POINT('Ctrl Pts',(161.416301168869,-15.6873171483045,4.08589577647466));
#28805=CARTESIAN_POINT('Ctrl Pts',(161.533994995353,-15.752979667711,-3.82493074399836));
#28806=CARTESIAN_POINT('Ctrl Pts',(161.651688821836,-12.0668967458695,-10.8248079212624));
#28807=CARTESIAN_POINT('Ctrl Pts',(161.769382648319,-5.50694958937003,-15.2466379844161));
#28808=CARTESIAN_POINT('Ctrl Pts',(161.887076474802,2.3645382059743,-16.0373134495834));
#28809=CARTESIAN_POINT('Ctrl Pts',(162.004770301285,9.67288521004985,-13.0085262547648));
#28810=CARTESIAN_POINT('Ctrl Pts',(162.122464127768,14.67752816854,-6.88161539679513));
#28811=CARTESIAN_POINT('Ctrl Pts',(162.240157954252,16.1865562937323,0.884227887797634));
#28812=CARTESIAN_POINT('Ctrl Pts',(162.357851780735,13.840577933451,8.43948257156437));
#28813=CARTESIAN_POINT('Ctrl Pts',(162.475545607218,8.19831364750381,13.9847816194923));
#28814=CARTESIAN_POINT('Ctrl Pts',(162.593239433701,0.603530758605001,16.1994510472156));
#28815=CARTESIAN_POINT('Ctrl Pts',(162.710933260184,-7.13498962120933,14.5560429620394));
#28816=CARTESIAN_POINT('Ctrl Pts',(162.828627086668,-13.1742337149738,9.44595308222564));
#28817=CARTESIAN_POINT('Ctrl Pts',(162.946320913151,-16.0758890905255,2.08620554003872));
#28818=CARTESIAN_POINT('Ctrl Pts',(163.064014739634,-15.1488945929473,-5.77039480644631));
#28819=CARTESIAN_POINT('Ctrl Pts',(163.181708566117,-10.6140241611372,-12.2527121369471));
#28820=CARTESIAN_POINT('Ctrl Pts',(163.2994023926,-3.55130708784071,-15.8169112527338));
#28821=CARTESIAN_POINT('Ctrl Pts',(163.417096219084,4.35719284595873,-15.6141389170616));
#28822=CARTESIAN_POINT('Ctrl Pts',(163.534790045567,11.2279793567904,-11.692687592161));
#28823=CARTESIAN_POINT('Ctrl Pts',(163.65248387205,15.4246990473113,-4.9864940609672));
#28824=CARTESIAN_POINT('Ctrl Pts',(163.770177698533,15.9478569233932,2.90728790015858));
#28825=CARTESIAN_POINT('Ctrl Pts',(163.887871525016,12.672857226445,10.108667254542));
#28826=CARTESIAN_POINT('Ctrl Pts',(164.005565351499,6.37967707542191,14.902556282264));
#28827=CARTESIAN_POINT('Ctrl Pts',(164.123259177983,-1.43289323788845,16.1472375393268));
#28828=CARTESIAN_POINT('Ctrl Pts',(164.240953004466,-8.90420452717788,13.5462765378252));
#28829=CARTESIAN_POINT('Ctrl Pts',(164.358646830949,-14.2548809857467,7.71912065876858));
#28830=CARTESIAN_POINT('Ctrl Pts',(164.476340657432,-16.2106018116086,0.0535713981899616));
#28831=CARTESIAN_POINT('Ctrl Pts',(164.594034483915,-14.3055871426404,-7.62473676440622));
#28832=CARTESIAN_POINT('Ctrl Pts',(164.711728310399,-8.99354421585697,-13.4871293872258));
#28833=CARTESIAN_POINT('Ctrl Pts',(164.829422136882,-1.53958007844154,-16.1374149400877));
#28834=CARTESIAN_POINT('Ctrl Pts',(164.947115963365,6.2810321020304,-14.9443951095233));
#28835=CARTESIAN_POINT('Ctrl Pts',(165.064809789848,12.6057881822385,-10.1922081771534));
#28836=CARTESIAN_POINT('Ctrl Pts',(165.182503616331,15.9282533966172,-3.01262440261544));
#28837=CARTESIAN_POINT('Ctrl Pts',(165.300197442815,15.457401518827,4.88442784961914));
#28838=CARTESIAN_POINT('Ctrl Pts',(165.417891269298,11.3048471203361,11.6182432782841));
#28839=CARTESIAN_POINT('Ctrl Pts',(165.535585095781,4.46064461548986,15.5849549117565));
#28840=CARTESIAN_POINT('Ctrl Pts',(165.653278922264,-3.4474027167462,15.8401177026368));
#28841=CARTESIAN_POINT('Ctrl Pts',(165.731741473253,-8.16944088361523,13.4945278683989));
#28842=CARTESIAN_POINT('Ctrl Pts',(165.770972748747,-10.1138936307938,11.8324957226905));
#28843=CARTESIAN_POINT('Origin',(157.6,0.,0.));
#28844=CARTESIAN_POINT('Origin',(165.275,0.,0.));
#28845=CARTESIAN_POINT('Ctrl Pts',(68.2290272512527,-8.6315465241079,18.1146005753553));
#28846=CARTESIAN_POINT('Ctrl Pts',(68.2686455391672,-11.6377133328369,16.682172156035));
#28847=CARTESIAN_POINT('Ctrl Pts',(68.3478821149964,-16.920167839264,12.2933105870388));
#28848=CARTESIAN_POINT('Ctrl Pts',(68.4667369787402,-20.7364191237466,2.71910129728484));
#28849=CARTESIAN_POINT('Ctrl Pts',(68.5855918424838,-19.5178285413225,-7.51269261680735));
#28850=CARTESIAN_POINT('Ctrl Pts',(68.7044467062276,-13.560781282725,-15.9217739264575));
#28851=CARTESIAN_POINT('Ctrl Pts',(68.8233015699713,-4.3112850075781,-20.4646502512393));
#28852=CARTESIAN_POINT('Ctrl Pts',(68.9421564337151,5.98487983261901,-20.039336396671));
#28853=CARTESIAN_POINT('Ctrl Pts',(69.0610112974588,14.8280289192567,-14.7486055907437));
#28854=CARTESIAN_POINT('Ctrl Pts',(69.1798661612025,20.0711408256307,-5.87721609629587));
#28855=CARTESIAN_POINT('Ctrl Pts',(69.2987210249463,20.4412844203846,4.42111651613181));
#28856=CARTESIAN_POINT('Ctrl Pts',(69.4175758886899,15.8485849447886,13.6460461909995));
#28857=CARTESIAN_POINT('Ctrl Pts',(69.5364307524338,7.40808631971404,19.5579297437878));
#28858=CARTESIAN_POINT('Ctrl Pts',(69.6552856161775,-2.83098632764961,20.7214331897253));
#28859=CARTESIAN_POINT('Ctrl Pts',(69.7741404799212,-12.3827371735606,16.8540836193131));
#28860=CARTESIAN_POINT('Ctrl Pts',(69.892995343665,-18.928143773215,8.89481171599467));
#28861=CARTESIAN_POINT('Ctrl Pts',(70.0118502074086,-20.8780784123747,-1.22398747391038));
#28862=CARTESIAN_POINT('Ctrl Pts',(70.1307050711525,-17.7591261183169,-11.0456210793205));
#28863=CARTESIAN_POINT('Ctrl Pts',(70.2495599348961,-10.3285220474192,-18.1855419414053));
#28864=CARTESIAN_POINT('Ctrl Pts',(70.36841479864,-0.390306419466782,-20.9102837301104));
#28865=CARTESIAN_POINT('Ctrl Pts',(70.4872696623836,9.64266981062011,-18.5583195092622));
#28866=CARTESIAN_POINT('Ctrl Pts',(70.6061245261274,17.3345491904711,-11.7006712929421));
#28867=CARTESIAN_POINT('Ctrl Pts',(70.724979389871,20.8178577880174,-2.00227405925465));
#28868=CARTESIAN_POINT('Ctrl Pts',(70.843834253615,19.2469000686554,8.18224553636222));
#28869=CARTESIAN_POINT('Ctrl Pts',(70.9626891173585,13.0030812084345,16.3802375864514));
#28870=CARTESIAN_POINT('Ctrl Pts',(71.0815439811024,3.602307582272,20.6013515178363));
#28871=CARTESIAN_POINT('Ctrl Pts',(71.200398844846,-6.67305275956469,19.8207636371352));
#28872=CARTESIAN_POINT('Ctrl Pts',(71.3192537085899,-15.3282951176304,14.2279890734018));
#28873=CARTESIAN_POINT('Ctrl Pts',(71.4381085723335,-20.2620553480119,5.1808703285721));
#28874=CARTESIAN_POINT('Ctrl Pts',(71.5569634360773,-20.2764898302783,-5.12408669424093));
#28875=CARTESIAN_POINT('Ctrl Pts',(71.6758182998211,-15.3680940867467,-14.1849916611866));
#28876=CARTESIAN_POINT('Ctrl Pts',(71.7946731635647,-6.72855361766429,-19.8019915791725));
#28877=CARTESIAN_POINT('Ctrl Pts',(71.9135280273086,3.54457961832131,-20.6113623910834));
#28878=CARTESIAN_POINT('Ctrl Pts',(72.0323828910522,12.9571416297572,-16.416600898898));
#28879=CARTESIAN_POINT('Ctrl Pts',(72.151237754796,19.2239023220937,-8.2361328181285));
#28880=CARTESIAN_POINT('Ctrl Pts',(72.2700926185397,20.8233853839836,1.94394584218601));
#28881=CARTESIAN_POINT('Ctrl Pts',(72.3889474822834,17.3672601118087,11.6520633578796));
#28882=CARTESIAN_POINT('Ctrl Pts',(72.5078023460272,9.69462233016103,18.5312331527829));
#28883=CARTESIAN_POINT('Ctrl Pts',(72.6266572097709,-0.331725597276454,
20.9112950917769));
#28884=CARTESIAN_POINT('Ctrl Pts',(72.7455120735146,-10.2775354823501,18.2144055268431));
#28885=CARTESIAN_POINT('Ctrl Pts',(72.8643669372584,-17.7281125760169,11.0953291424513));
#28886=CARTESIAN_POINT('Ctrl Pts',(72.9832218010021,-20.8745675476636,1.28247182631354));
#28887=CARTESIAN_POINT('Ctrl Pts',(73.1020766647459,-18.9529879169663,-8.84175057930195));
#28888=CARTESIAN_POINT('Ctrl Pts',(73.2209315284896,-12.429904644976,-16.8193274183025));
#28889=CARTESIAN_POINT('Ctrl Pts',(73.3397863922333,-2.88902535394313,-20.7134216582276));
#28890=CARTESIAN_POINT('Ctrl Pts',(73.4586412559771,7.35326633413225,-19.5786051215753));
#28891=CARTESIAN_POINT('Ctrl Pts',(73.5774961197208,15.8102942970291,-13.6903943890812));
#28892=CARTESIAN_POINT('Ctrl Pts',(73.6963509834645,20.4288178986918,-4.47835947076039));
#28893=CARTESIAN_POINT('Ctrl Pts',(73.8152058472083,20.0875282846243,5.82095453526969));
#28894=CARTESIAN_POINT('Ctrl Pts',(73.934060710952,14.8692854982535,14.7070273358924));
#28895=CARTESIAN_POINT('Ctrl Pts',(74.0529155746958,6.04100129448752,20.0224525882135));
#28896=CARTESIAN_POINT('Ctrl Pts',(74.1717704384394,-4.25394819579815,20.4767240796648));
#28897=CARTESIAN_POINT('Ctrl Pts',(74.2906253021834,-13.5161023190106,15.9595514469955));
#28898=CARTESIAN_POINT('Ctrl Pts',(74.4094801659269,-19.4967477793413,7.56763703648682));
#28899=CARTESIAN_POINT('Ctrl Pts',(74.5283350296708,-20.7438727893319,-2.66158711810738));
#28900=CARTESIAN_POINT('Ctrl Pts',(74.6471898934143,-16.9546939409116,-12.2446174973853));
#28901=CARTESIAN_POINT('Ctrl Pts',(74.7660447571583,-9.04916751458383,-18.8548368218943));
#28902=CARTESIAN_POINT('Ctrl Pts',(74.8848996209018,1.05336222602103,-20.8873821315178));
#28903=CARTESIAN_POINT('Ctrl Pts',(75.0037544846458,10.9001512813116,-17.8487816483865));
#28904=CARTESIAN_POINT('Ctrl Pts',(75.1226093483893,18.1005456873079,-10.4767623867747));
#28905=CARTESIAN_POINT('Ctrl Pts',(75.2414642121331,20.9063967498254,-0.561141003802912));
#28906=CARTESIAN_POINT('Ctrl Pts',(75.3603190758769,18.6364855530042,9.4907170709027));
#28907=CARTESIAN_POINT('Ctrl Pts',(75.4791739396206,11.8419127825698,17.2383701647594));
#28908=CARTESIAN_POINT('Ctrl Pts',(75.5980288033644,2.1722996740317,20.8008033117344));
#28909=CARTESIAN_POINT('Ctrl Pts',(75.7168836671081,-8.02471549395103,19.3131107159981));
#28910=CARTESIAN_POINT('Ctrl Pts',(75.8357385308518,-16.2734490649882,13.1364820182761));
#28911=CARTESIAN_POINT('Ctrl Pts',(75.9545933945955,-20.5712311840959,3.77051082185677));
#28912=CARTESIAN_POINT('Ctrl Pts',(76.0734482583393,-19.8746242594179,-6.51088433580387));
#28913=CARTESIAN_POINT('Ctrl Pts',(76.192303122083,-14.352754093941,-15.2115335915258));
#28914=CARTESIAN_POINT('Ctrl Pts',(76.3111579858267,-5.34624865537712,-20.2190486819271));
#28915=CARTESIAN_POINT('Ctrl Pts',(76.4300128495705,4.95824645968282,-20.3176794032267));
#28916=CARTESIAN_POINT('Ctrl Pts',(76.5488677133142,14.0589530618911,-15.4834796829007));
#28917=CARTESIAN_POINT('Ctrl Pts',(76.667722577058,19.7463549128656,-6.8901213300209));
#28918=CARTESIAN_POINT('Ctrl Pts',(76.7865774408017,20.6396354130593,3.3760560278593));
#28919=CARTESIAN_POINT('Ctrl Pts',(76.9054323045454,16.5219193398244,12.8225771830625));
#28920=CARTESIAN_POINT('Ctrl Pts',(77.0242871682892,8.39292692660435,19.1559672658923));
#28921=CARTESIAN_POINT('Ctrl Pts',(77.1431420320329,-1.77374334422174,20.8385733397488));
#28922=CARTESIAN_POINT('Ctrl Pts',(77.2619968957766,-11.5097751060743,17.4618836697204));
#28923=CARTESIAN_POINT('Ctrl Pts',(77.3808517595204,-18.451404618894,9.84570829738103));
#28924=CARTESIAN_POINT('Ctrl Pts',(77.4997066232641,-20.9133074568072,-0.160858646988668));
#28925=CARTESIAN_POINT('Ctrl Pts',(77.6185614870079,-18.2977702184867,-10.1283715037868));
#28926=CARTESIAN_POINT('Ctrl Pts',(77.7374163507516,-11.2398064531836,-17.636866365152));
#28927=CARTESIAN_POINT('Ctrl Pts',(77.8562712144954,-1.45298481342087,-20.8633923276927));
#28928=CARTESIAN_POINT('Ctrl Pts',(77.975126078239,8.68659993361501,-19.0245968651264));
#28929=CARTESIAN_POINT('Ctrl Pts',(78.0939809419828,16.7172073837676,-12.5669121734563));
#28930=CARTESIAN_POINT('Ctrl Pts',(78.2128358057265,20.6891254607372,-3.05816807208725));
#28931=CARTESIAN_POINT('Ctrl Pts',(78.3316906694703,19.6380315166033,7.19305376319089));
#28932=CARTESIAN_POINT('Ctrl Pts',(78.450545533214,13.8191155315665,15.6979091032047));
#28933=CARTESIAN_POINT('Ctrl Pts',(78.5694003969578,4.6451237813503,20.3915455359125));
#28934=CARTESIAN_POINT('Ctrl Pts',(78.6882552607015,-5.65663495145375,20.1344179283447));
#28935=CARTESIAN_POINT('Ctrl Pts',(78.8071101244452,-14.5850468304206,14.9889530402125));
#28936=CARTESIAN_POINT('Ctrl Pts',(78.925964988189,-19.9724262140028,6.20439323491602));
#28937=CARTESIAN_POINT('Ctrl Pts',(79.0448198519327,-20.5107974964971,-4.08650099044958));
#28938=CARTESIAN_POINT('Ctrl Pts',(79.1636747156764,-16.0694521359249,-13.3852535403135));
#28939=CARTESIAN_POINT('Ctrl Pts',(79.2825295794202,-7.72668274442983,-19.4342655650835));
#28940=CARTESIAN_POINT('Ctrl Pts',(79.401384443164,2.49201032407988,-20.7649268920441));
#28941=CARTESIAN_POINT('Ctrl Pts',(79.5202393069076,12.1056803413097,-17.0541727375234));
#28942=CARTESIAN_POINT('Ctrl Pts',(79.6390941706514,18.7802711793142,-9.20291903249607));
#28943=CARTESIAN_POINT('Ctrl Pts',(79.7579490343951,20.8952914316842,0.882666569120876));
#28944=CARTESIAN_POINT('Ctrl Pts',(79.8768038981389,17.9372456308276,10.7539538527284));
#28945=CARTESIAN_POINT('Ctrl Pts',(79.9956587618826,10.6243033119855,18.014341048792));
#28946=CARTESIAN_POINT('Ctrl Pts',(80.1145136256262,0.731938129029032,20.9011141057727));
#28947=CARTESIAN_POINT('Ctrl Pts',(80.2333684893701,-9.33813074796676,18.7134074508395));
#28948=CARTESIAN_POINT('Ctrl Pts',(80.3522233531138,-17.1410403344121,11.982363729303));
#28949=CARTESIAN_POINT('Ctrl Pts',(80.4710782168576,-20.7823602095201,2.34218026825721));
#28950=CARTESIAN_POINT('Ctrl Pts',(80.5899330806012,-19.3780320528914,-7.86664973444038));
#28951=CARTESIAN_POINT('Ctrl Pts',(80.708787944345,-13.2690058590392,-16.1655741562136));
#28952=CARTESIAN_POINT('Ctrl Pts',(80.8276428080888,-3.93846234853991,-20.5397375498421));
#28953=CARTESIAN_POINT('Ctrl Pts',(80.9464976718324,6.34828125649317,-19.9271580857812));
#28954=CARTESIAN_POINT('Ctrl Pts',(81.0653525355762,15.0937565693877,-14.4765609490419));
#28955=CARTESIAN_POINT('Ctrl Pts',(81.1842073993199,20.1746922266295,-5.51127007576585));
#28956=CARTESIAN_POINT('Ctrl Pts',(81.3030622630637,20.3575126025494,4.7920752210601));
#28957=CARTESIAN_POINT('Ctrl Pts',(81.4219171268074,15.5978316283554,13.9319759108582));
#28958=CARTESIAN_POINT('Ctrl Pts',(81.5407719905512,7.05122906962834,19.6894000135831));
#28959=CARTESIAN_POINT('Ctrl Pts',(81.6596268542949,-3.20730705765452,20.6665305681718));
#28960=CARTESIAN_POINT('Ctrl Pts',(81.7784817180386,-12.6871567229822,16.6261348055928));
#28961=CARTESIAN_POINT('Ctrl Pts',(81.8973365817824,-19.0867533899846,8.54916073759119));
#28962=CARTESIAN_POINT('Ctrl Pts',(82.0161914455261,-20.8523701478954,-1.60342243417667));
#28963=CARTESIAN_POINT('Ctrl Pts',(82.1350463092699,-17.5553415020576,-11.3667184813117));
#28964=CARTESIAN_POINT('Ctrl Pts',(82.2539011730136,-9.99613698190578,-18.3703443006992));
#28965=CARTESIAN_POINT('Ctrl Pts',(82.3727560367574,-0.0100190419482207,
-20.9139236850969));
#28966=CARTESIAN_POINT('Ctrl Pts',(82.4916109005011,9.9785313724145,-18.3799133821952));
#28967=CARTESIAN_POINT('Ctrl Pts',(82.6104657642448,17.544442747166,-11.3835334136054));
#28968=CARTESIAN_POINT('Ctrl Pts',(82.7293206279886,20.8508243032301,-1.62340080174));
#28969=CARTESIAN_POINT('Ctrl Pts',(82.8481754917323,19.0949357636439,8.53086938533054));
#28970=CARTESIAN_POINT('Ctrl Pts',(82.9670303554759,12.7030807563111,16.6139713369771));
#28971=CARTESIAN_POINT('Ctrl Pts',(83.0858852192198,3.22710663214606,20.6634480925139));
#28972=CARTESIAN_POINT('Ctrl Pts',(83.2047400829634,-7.03236099624711,19.6961469101375));
#28973=CARTESIAN_POINT('Ctrl Pts',(83.3235949467073,-15.5844759437393,13.9469141334658));
#28974=CARTESIAN_POINT('Ctrl Pts',(83.4424498104509,-20.3529118683285,4.81157799139837));
#28975=CARTESIAN_POINT('Ctrl Pts',(83.5613046741947,-20.1799634326612,-5.49193774033512));
#28976=CARTESIAN_POINT('Ctrl Pts',(83.6801595379384,-15.1076199452285,-14.4620926520955));
#28977=CARTESIAN_POINT('Ctrl Pts',(83.7990144016822,-6.36737098063297,-19.9210665146787));
#28978=CARTESIAN_POINT('Ctrl Pts',(83.9178692654259,3.91878097726412,-20.5435016474673));
#28979=CARTESIAN_POINT('Ctrl Pts',(84.0367241291697,13.2535111849172,-16.1782800556342));
#28980=CARTESIAN_POINT('Ctrl Pts',(84.1555789929134,19.3704859523993,-7.88521263220971));
#28981=CARTESIAN_POINT('Ctrl Pts',(84.2744338566571,20.7845947636492,2.32226716769303));
#28982=CARTESIAN_POINT('Ctrl Pts',(84.3932887204008,17.152513026647,11.9659350306595));
#28983=CARTESIAN_POINT('Ctrl Pts',(84.5121435841446,9.3560561792281,18.7044517978578));
#28984=CARTESIAN_POINT('Ctrl Pts',(84.6309984478883,-0.711911986905901,
20.901805797829));
#28985=CARTESIAN_POINT('Ctrl Pts',(84.7498533116321,-10.6070385085257,18.0245121533403));
#28986=CARTESIAN_POINT('Ctrl Pts',(84.8687081753758,-17.9269338035892,10.7711349768254));
#28987=CARTESIAN_POINT('Ctrl Pts',(84.9875630391195,-20.8944361389867,0.902686391313687));
#28988=CARTESIAN_POINT('Ctrl Pts',(85.1064179028633,-18.7890800735068,-9.18492102734728));
#28989=CARTESIAN_POINT('Ctrl Pts',(85.225272766607,-12.122014753868,-17.0425661974441));
#28990=CARTESIAN_POINT('Ctrl Pts',(85.3441276303508,-2.51190450252216,-20.7625297123801));
#28991=CARTESIAN_POINT('Ctrl Pts',(85.4629824940945,7.70805881080918,-19.4416597454118));
#28992=CARTESIAN_POINT('Ctrl Pts',(85.5818373578382,16.0566200612769,-13.4006438835997));
#28993=CARTESIAN_POINT('Ctrl Pts',(85.700692221582,20.5068727177375,-4.10615095019311));
#28994=CARTESIAN_POINT('Ctrl Pts',(85.8195470853257,19.9783616090541,6.18525437675218));
#28995=CARTESIAN_POINT('Ctrl Pts',(85.9384019490693,14.5994013736218,14.9749719138016));
#28996=CARTESIAN_POINT('Ctrl Pts',(86.0572568128132,5.67592357316316,20.1289889432845));
#28997=CARTESIAN_POINT('Ctrl Pts',(86.1761116765568,-4.62558407166802,20.3959867690482));
#28998=CARTESIAN_POINT('Ctrl Pts',(86.2949665403008,-13.8040686848729,15.7111422891708));
#28999=CARTESIAN_POINT('Ctrl Pts',(86.4138214040442,-19.6311306835337,7.21186608120808));
#29000=CARTESIAN_POINT('Ctrl Pts',(86.5326762677881,-20.6920460609478,-3.03834397310024));
#29001=CARTESIAN_POINT('Ctrl Pts',(86.6515311315318,-16.7292403389556,-12.5508892899555));
#29002=CARTESIAN_POINT('Ctrl Pts',(86.7703859952756,-8.70482382118687,-19.0162653149707));
#29003=CARTESIAN_POINT('Ctrl Pts',(86.8892408590193,1.432994482384,-20.8647748873721));
#29004=CARTESIAN_POINT('Ctrl Pts',(87.0080957227631,11.2229030338076,-17.6476273697347));
#29005=CARTESIAN_POINT('Ctrl Pts',(87.1269505865067,18.2880576096475,-10.1458983413729));
#29006=CARTESIAN_POINT('Ctrl Pts',(87.2458054502506,20.9131437355076,-0.180896062030789));
#29007=CARTESIAN_POINT('Ctrl Pts',(87.3646603139942,18.460829534231,9.82802509130509));
#29008=CARTESIAN_POINT('Ctrl Pts',(87.4835151777381,11.5265004287498,17.4508478921023));
#29009=CARTESIAN_POINT('Ctrl Pts',(87.6023700414816,1.79370841459017,20.8368643132955));
#29010=CARTESIAN_POINT('Ctrl Pts',(87.7212249052256,-8.37456933075415,19.1639999168141));
#29011=CARTESIAN_POINT('Ctrl Pts',(87.8400797689691,-16.5096261697931,12.8384013031585));
#29012=CARTESIAN_POINT('Ctrl Pts',(87.958934632713,-20.636391267735,3.39582975606967));
#29013=CARTESIAN_POINT('Ctrl Pts',(88.0777894964567,-19.7529474224935,-6.87119876087563));
#29014=CARTESIAN_POINT('Ctrl Pts',(88.1966443602004,-14.0737816631622,-15.4700023912384));
#29015=CARTESIAN_POINT('Ctrl Pts',(88.3154992239441,-4.97771098870528,-20.312919475056));
#29016=CARTESIAN_POINT('Ctrl Pts',(88.4343540876879,5.32687389681903,-20.2241617570368));
#29017=CARTESIAN_POINT('Ctrl Pts',(88.5532089514316,14.3381730091277,-15.2252782912942));
#29018=CARTESIAN_POINT('Ctrl Pts',(88.6720638151754,19.868376918928,-6.52992365153576));
#29019=CARTESIAN_POINT('Ctrl Pts',(88.790918678919,20.5748343493,3.75079935297009));
#29020=CARTESIAN_POINT('Ctrl Pts',(88.9097735426629,16.2860279409612,13.1208840476639));
#29021=CARTESIAN_POINT('Ctrl Pts',(89.0286284064065,8.04321611663378,19.3054131992102));
#29022=CARTESIAN_POINT('Ctrl Pts',(89.1474832701505,-2.15236898069497,20.8028750909506));
#29023=CARTESIAN_POINT('Ctrl Pts',(89.2663381338938,-11.8253908946233,17.2497082436515));
#29024=CARTESIAN_POINT('Ctrl Pts',(89.3851929976379,-18.6273837390381,9.50856873082095));
#29025=CARTESIAN_POINT('Ctrl Pts',(89.5040478613814,-20.9069247951813,-0.541109877118889));
#29026=CARTESIAN_POINT('Ctrl Pts',(89.6229027251253,-18.1105753899303,-10.4594150595525));
#29027=CARTESIAN_POINT('Ctrl Pts',(89.7417575888689,-10.9172475795155,-17.8383297808979));
#29028=CARTESIAN_POINT('Ctrl Pts',(89.8606124526128,-1.07337439090547,-20.886363306994));
#29029=CARTESIAN_POINT('Ctrl Pts',(89.9794673163564,9.03109813531615,-18.8634983461956));
#29030=CARTESIAN_POINT('Ctrl Pts',(90.0983221801003,16.9429543312567,-12.2608565786884));
#29031=CARTESIAN_POINT('Ctrl Pts',(90.2171770438438,20.7413131374097,-2.68146095729082));
#29032=CARTESIAN_POINT('Ctrl Pts',(90.3360319075878,19.5039895591631,7.5489531352732));
#29033=CARTESIAN_POINT('Ctrl Pts',(90.4548867713314,13.531387277919,15.9465943979035));
#29034=CARTESIAN_POINT('Ctrl Pts',(90.5737416350752,4.2735654835411,20.4726382052112));
#29035=CARTESIAN_POINT('Ctrl Pts',(90.6925964988188,-6.021814680891,20.0282327411152));
#29036=CARTESIAN_POINT('Ctrl Pts',(90.8114513625627,-14.8551873562319,14.7212645520118));
#29037=CARTESIAN_POINT('Ctrl Pts',(90.9303062263063,-20.0819422730131,5.84020329677328));
#29038=CARTESIAN_POINT('Ctrl Pts',(91.0491610900501,-20.4330985674198,-4.45879423375491));
#29039=CARTESIAN_POINT('Ctrl Pts',(91.1680159537938,-15.8234056085072,-13.6752200512566));
#29040=CARTESIAN_POINT('Ctrl Pts',(91.2868708175377,-7.37201867707368,-19.5715898806077));
#29041=CARTESIAN_POINT('Ctrl Pts',(91.4057256812812,2.86917222790772,-20.7161033751214));
#29042=CARTESIAN_POINT('Ctrl Pts',(91.5245805450251,12.4137954244847,-16.8313801312361));
#29043=CARTESIAN_POINT('Ctrl Pts',(91.6434354087687,18.9444853649975,-8.85960809395612));
#29044=CARTESIAN_POINT('Ctrl Pts',(91.7622902725126,20.8758294198323,1.26187795552705));
#29045=CARTESIAN_POINT('Ctrl Pts',(91.8811451362562,17.7386656817295,11.0795895560304));
#29046=CARTESIAN_POINT('Ctrl Pts',(91.9603817120854,12.7761628790883,15.8272202722995));
#29047=CARTESIAN_POINT('Ctrl Pts',(92.,9.87756200380534,17.4664283201656));
#29048=CARTESIAN_POINT('Ctrl Pts',(68.3943515008351,-8.75472251862488,18.3731039542012));
#29049=CARTESIAN_POINT('Ctrl Pts',(68.4339697887497,-11.8037886600882,16.9202341464656));
#29050=CARTESIAN_POINT('Ctrl Pts',(68.5132063645789,-17.1616261335772,12.4687415776771));
#29051=CARTESIAN_POINT('Ctrl Pts',(68.6320612283225,-21.0323370153035,2.75790407793953));
#29052=CARTESIAN_POINT('Ctrl Pts',(68.7509160920664,-19.7963566051723,-7.61990207017598));
#29053=CARTESIAN_POINT('Ctrl Pts',(68.86977095581,-13.7542996419509,-16.1489846971332));
#29054=CARTESIAN_POINT('Ctrl Pts',(68.9886258195538,-4.37280895545597,-20.7566898805338));
#29055=CARTESIAN_POINT('Ctrl Pts',(69.1074806832975,6.07028672041002,-20.325306608756));
#29056=CARTESIAN_POINT('Ctrl Pts',(69.2263355470413,15.0396314639171,-14.9590747293047));
#29057=CARTESIAN_POINT('Ctrl Pts',(69.345190410785,20.3575649010131,-5.96108657485157));
#29058=CARTESIAN_POINT('Ctrl Pts',(69.4640452745288,20.7329906089168,4.48420780831553));
#29059=CARTESIAN_POINT('Ctrl Pts',(69.5829001382724,16.0747512762576,13.840781318257));
#29060=CARTESIAN_POINT('Ctrl Pts',(69.7017550020163,7.51380299486025,19.8370300695702));
#29061=CARTESIAN_POINT('Ctrl Pts',(69.8206098657599,-2.8713857572765,21.0171372253617));
#29062=CARTESIAN_POINT('Ctrl Pts',(69.9394647295037,-12.5594443212236,17.0945988625182));
#29063=CARTESIAN_POINT('Ctrl Pts',(70.0583195932474,-19.1982567740677,9.02174462148259));
#29064=CARTESIAN_POINT('Ctrl Pts',(70.1771744569911,-21.1760178447656,-1.24145431765083));
#29065=CARTESIAN_POINT('Ctrl Pts',(70.2960293207349,-18.0125567191098,-11.2032469876909));
#29066=CARTESIAN_POINT('Ctrl Pts',(70.4148841844786,-10.4759146347763,-18.4450576849868));
#29067=CARTESIAN_POINT('Ctrl Pts',(70.5337390482224,-0.395876265061667,
-21.2086827466592));
#29068=CARTESIAN_POINT('Ctrl Pts',(70.6525939119661,9.78027498257911,-18.8231549539572));
#29069=CARTESIAN_POINT('Ctrl Pts',(70.7714487757098,17.5819208903253,-11.867645058188));
#29070=CARTESIAN_POINT('Ctrl Pts',(70.8903036394535,21.1149378454081,-2.03084739751513));
#29071=CARTESIAN_POINT('Ctrl Pts',(71.0091585031973,19.5215618631211,8.29900980664779));
#29072=CARTESIAN_POINT('Ctrl Pts',(71.128013366941,13.1886409404201,16.6139908367525));
#29073=CARTESIAN_POINT('Ctrl Pts',(71.2468682306848,3.65371410806238,20.895341934793));
#29074=CARTESIAN_POINT('Ctrl Pts',(71.3657230944285,-6.76828018003073,20.1036147190673));
#29075=CARTESIAN_POINT('Ctrl Pts',(71.4845779581723,-15.5470366826663,14.4310287835161));
#29076=CARTESIAN_POINT('Ctrl Pts',(71.603432821916,-20.5512038582445,5.25480364439256));
#29077=CARTESIAN_POINT('Ctrl Pts',(71.7222876856597,-20.5658443269705,-5.19720968243216));
#29078=CARTESIAN_POINT('Ctrl Pts',(71.8411425494035,-15.5874036007114,-14.3874177791715));
#29079=CARTESIAN_POINT('Ctrl Pts',(71.9599974131472,-6.82457305997421,-20.0845747755174));
#29080=CARTESIAN_POINT('Ctrl Pts',(72.078852276891,3.59516234048029,-20.9054956676383));
#29081=CARTESIAN_POINT('Ctrl Pts',(72.1977071406347,13.1420457835939,-16.6508730697845));
#29082=CARTESIAN_POINT('Ctrl Pts',(72.3165620043785,19.4982359285231,-8.35366608380849));
#29083=CARTESIAN_POINT('Ctrl Pts',(72.4354168681221,21.1205443226187,1.97168681093702));
#29084=CARTESIAN_POINT('Ctrl Pts',(72.5542717318659,17.6150986110084,11.8183434663484));
#29085=CARTESIAN_POINT('Ctrl Pts',(72.6731265956096,9.83296888759997,18.7956820631658));
#29086=CARTESIAN_POINT('Ctrl Pts',(72.7919814593534,-0.336459468574833,
21.2097085409049));
#29087=CARTESIAN_POINT('Ctrl Pts',(72.9108363230971,-10.4242004688258,18.4743331665816));
#29088=CARTESIAN_POINT('Ctrl Pts',(73.0296911868409,-17.9811005998156,11.2536644069138));
#29089=CARTESIAN_POINT('Ctrl Pts',(73.1485460505845,-21.172456878459,1.30077326768389));
#29090=CARTESIAN_POINT('Ctrl Pts',(73.2674009143283,-19.2234554547616,-8.96792627885183));
#29091=CARTESIAN_POINT('Ctrl Pts',(73.386255778072,-12.6072848933614,-17.0593466751147));
#29092=CARTESIAN_POINT('Ctrl Pts',(73.5051106418158,-2.93025302619897,-21.0090113657587));
#29093=CARTESIAN_POINT('Ctrl Pts',(73.6239655055595,7.45820070378722,-19.8580004941624));
#29094=CARTESIAN_POINT('Ctrl Pts',(73.7428203693033,16.0359142039836,-13.8857623847811));
#29095=CARTESIAN_POINT('Ctrl Pts',(73.8616752330469,20.720346184434,-4.54226764527755));
#29096=CARTESIAN_POINT('Ctrl Pts',(73.9805300967909,20.3741862163097,5.90402213641362));
#29097=CARTESIAN_POINT('Ctrl Pts',(74.0993849605344,15.0814767925817,14.9169031343287));
#29098=CARTESIAN_POINT('Ctrl Pts',(74.2182398242783,6.12720906041322,20.3081818608687));
#29099=CARTESIAN_POINT('Ctrl Pts',(74.3370946880219,-4.31465392195945,20.7689360078422));
#29100=CARTESIAN_POINT('Ctrl Pts',(74.4559495517657,-13.7089830896219,16.1873013196328));
#29101=CARTESIAN_POINT('Ctrl Pts',(74.5748044155094,-19.7749750113744,7.67563057107641));
#29102=CARTESIAN_POINT('Ctrl Pts',(74.6936592792532,-21.0398970480001,-2.69956914593409));
#29103=CARTESIAN_POINT('Ctrl Pts',(74.8125141429968,-17.1966449379978,-12.4193536160528));
#29104=CARTESIAN_POINT('Ctrl Pts',(74.9313690067407,-9.17830314573018,-19.123903700061));
#29105=CARTESIAN_POINT('Ctrl Pts',(75.0502238704843,1.06839417185068,-21.1854543321044));
#29106=CARTESIAN_POINT('Ctrl Pts',(75.1690787342282,11.0557012711902,-18.10349167333));
#29107=CARTESIAN_POINT('Ctrl Pts',(75.2879335979718,18.358848496672,-10.6262704294766));
#29108=CARTESIAN_POINT('Ctrl Pts',(75.4067884617156,21.2047402974427,-0.569148734632473));
#29109=CARTESIAN_POINT('Ctrl Pts',(75.5256433254594,18.9024364617877,9.62615380991842));
#29110=CARTESIAN_POINT('Ctrl Pts',(75.644498189203,12.0109021264727,17.484369347289));
#29111=CARTESIAN_POINT('Ctrl Pts',(75.7633530529468,2.2032993531727,21.0976399941897));
#29112=CARTESIAN_POINT('Ctrl Pts',(75.8822079166905,-8.13923174071195,19.5887173657469));
#29113=CARTESIAN_POINT('Ctrl Pts',(76.0010627804342,-16.505678395758,13.3239454389432));
#29114=CARTESIAN_POINT('Ctrl Pts',(76.119917644178,-20.8647917705404,3.824317682426));
#29115=CARTESIAN_POINT('Ctrl Pts',(76.2387725079218,-20.1582439563016,-6.60379754098762));
#29116=CARTESIAN_POINT('Ctrl Pts',(76.3576273716655,-14.557574256196,-15.4286089178339));
#29117=CARTESIAN_POINT('Ctrl Pts',(76.4764822354091,-5.42254199321897,-20.5075834679736));
#29118=CARTESIAN_POINT('Ctrl Pts',(76.595337099153,5.02900283422426,-20.6076216933806));
#29119=CARTESIAN_POINT('Ctrl Pts',(76.7141919628966,14.2595805532021,-15.704435800463));
#29120=CARTESIAN_POINT('Ctrl Pts',(76.8330468266405,20.0281441493233,-6.98844641519513));
#29121=CARTESIAN_POINT('Ctrl Pts',(76.9519016903841,20.9341721581688,3.42423384369045));
#29122=CARTESIAN_POINT('Ctrl Pts',(77.0707565541279,16.7576944515415,13.0055610426041));
#29123=CARTESIAN_POINT('Ctrl Pts',(77.1896114178716,8.51269771370555,19.42933140896));
#29124=CARTESIAN_POINT('Ctrl Pts',(77.3084662816154,-1.79905544789076,21.1359490172441));
#29125=CARTESIAN_POINT('Ctrl Pts',(77.427321145359,-11.6740246981257,17.71107248903));
#29126=CARTESIAN_POINT('Ctrl Pts',(77.5461760091029,-18.7147143407172,9.98621091853553));
#29127=CARTESIAN_POINT('Ctrl Pts',(77.6650308728465,-21.2117496232761,-0.163154171175886));
#29128=CARTESIAN_POINT('Ctrl Pts',(77.7838857365904,-18.5588875093233,-10.2729078541768));
#29129=CARTESIAN_POINT('Ctrl Pts',(77.902740600334,-11.4002034729046,-17.88855226508));
#29130=CARTESIAN_POINT('Ctrl Pts',(78.0215954640778,-1.47371955069089,-21.1611221831461));
#29131=CARTESIAN_POINT('Ctrl Pts',(78.1404503278215,8.81056156468606,-19.29608629435));
#29132=CARTESIAN_POINT('Ctrl Pts',(78.2593051915654,16.955769342426,-12.7462475799967));
#29133=CARTESIAN_POINT('Ctrl Pts',(78.3781600553089,20.9843684507617,-3.10180948589734));
#29134=CARTESIAN_POINT('Ctrl Pts',(78.4970149190528,19.918274930186,7.29570182845017));
#29135=CARTESIAN_POINT('Ctrl Pts',(78.6158697827964,14.0163204350206,15.9219252236326));
#29136=CARTESIAN_POINT('Ctrl Pts',(78.7347246465403,4.71141175649178,20.6825419285183));
#29137=CARTESIAN_POINT('Ctrl Pts',(78.8535795102839,-5.73735763930797,20.4217449960281));
#29138=CARTESIAN_POINT('Ctrl Pts',(78.9724343740277,-14.7931819129804,15.2028520434027));
#29139=CARTESIAN_POINT('Ctrl Pts',(79.0912892377714,-20.2574415881256,6.29293267624914));
#29140=CARTESIAN_POINT('Ctrl Pts',(79.2101441015152,-20.8034956674346,-4.14481717077568));
#29141=CARTESIAN_POINT('Ctrl Pts',(79.3289989652588,-16.2987703401028,-13.5762670408589));
#29142=CARTESIAN_POINT('Ctrl Pts',(79.4478538290027,-7.83694593176299,-19.7116011482261));
#29143=CARTESIAN_POINT('Ctrl Pts',(79.5667086927464,2.5275724158971,-21.0612516020896));
#29144=CARTESIAN_POINT('Ctrl Pts',(79.6855635564901,12.2784337651812,-17.2975433411275));
#29145=CARTESIAN_POINT('Ctrl Pts',(79.8044184202338,19.0482739727128,-9.33424876594779));
#29146=CARTESIAN_POINT('Ctrl Pts',(79.9232732839776,21.1934765014896,0.895262612271957));
#29147=CARTESIAN_POINT('Ctrl Pts',(80.0421281477213,18.193218076009,10.9074175405044));
#29148=CARTESIAN_POINT('Ctrl Pts',(80.1609830114651,10.7759168290822,18.2714136797575));
#29149=CARTESIAN_POINT('Ctrl Pts',(80.2798378752087,0.742383210535154,21.1993822677181));
#29150=CARTESIAN_POINT('Ctrl Pts',(80.3986927389525,-9.47139001252587,18.9804560691979));
#29151=CARTESIAN_POINT('Ctrl Pts',(80.5175476026963,-17.3856505771247,12.1533573704655));
#29152=CARTESIAN_POINT('Ctrl Pts',(80.63640246644,-21.0789337007326,2.37560421877118));
#29153=CARTESIAN_POINT('Ctrl Pts',(80.7552573301837,-19.6545651588917,-7.9789103127562));
#29154=CARTESIAN_POINT('Ctrl Pts',(80.8741121939275,-13.4583604536502,-16.3962640642236));
#29155=CARTESIAN_POINT('Ctrl Pts',(80.9929670576711,-3.99466595183329,-20.8328487081673));
#29156=CARTESIAN_POINT('Ctrl Pts',(81.111821921415,6.43887404366729,-20.2115274636509));
#29157=CARTESIAN_POINT('Ctrl Pts',(81.2306767851586,15.3091511653896,-14.683147889992));
#29158=CARTESIAN_POINT('Ctrl Pts',(81.3495316489025,20.4625940263995,-5.58991834241638));
#29159=CARTESIAN_POINT('Ctrl Pts',(81.4683865126461,20.6480233301123,4.86046025837706));
#29160=CARTESIAN_POINT('Ctrl Pts',(81.5872413763899,15.8204195988616,14.130791381946));
#29161=CARTESIAN_POINT('Ctrl Pts',(81.7060962401336,7.15185323365191,19.9703764783849));
#29162=CARTESIAN_POINT('Ctrl Pts',(81.8249511038774,-3.25307675088904,20.961451119065));
#29163=CARTESIAN_POINT('Ctrl Pts',(81.943805967621,-12.8682080725383,16.8633971181961));
#29164=CARTESIAN_POINT('Ctrl Pts',(82.0626608313649,-19.3591298203665,8.67116105042012));
#29165=CARTESIAN_POINT('Ctrl Pts',(82.1815156951086,-21.1499427119579,-1.62630398297084));
#29166=CARTESIAN_POINT('Ctrl Pts',(82.3003705588523,-17.8058640060564,-11.5289265919231));
#29167=CARTESIAN_POINT('Ctrl Pts',(82.4192254225961,-10.1387862870605,-18.6324972558549));
#29168=CARTESIAN_POINT('Ctrl Pts',(82.5380802863397,-0.010162018117406,
-21.2123746454166));
#29169=CARTESIAN_POINT('Ctrl Pts',(82.6569351500835,10.1209294377187,-18.6422028923849));
#29170=CARTESIAN_POINT('Ctrl Pts',(82.7757900138273,17.794809721102,-11.5459814807533));
#29171=CARTESIAN_POINT('Ctrl Pts',(82.8946448775709,21.148374807404,-1.64656745069401));
#29172=CARTESIAN_POINT('Ctrl Pts',(83.0134997413148,19.3674289601245,8.6526086724557));
#29173=CARTESIAN_POINT('Ctrl Pts',(83.1323546050585,12.8843593488806,16.8510600714922));
#29174=CARTESIAN_POINT('Ctrl Pts',(83.2512094688022,3.27315887408406,20.9583246551133));
#29175=CARTESIAN_POINT('Ctrl Pts',(83.370064332546,-7.13271590450091,19.9772196561435));
#29176=CARTESIAN_POINT('Ctrl Pts',(83.4889191962896,-15.8068733227066,14.1459427796111));
#29177=CARTESIAN_POINT('Ctrl Pts',(83.6077740600334,-20.643356941375,4.880241341892));
#29178=CARTESIAN_POINT('Ctrl Pts',(83.7266289237771,-20.4679404548775,-5.57031012599066));
#29179=CARTESIAN_POINT('Ctrl Pts',(83.8454837875209,-15.323212377748,-14.6684731240356));
#29180=CARTESIAN_POINT('Ctrl Pts',(83.9643386512646,-6.45823618663142,-20.2053489631288));
#29181=CARTESIAN_POINT('Ctrl Pts',(84.0831935150084,3.9747037186663,-20.836666521134));
#29182=CARTESIAN_POINT('Ctrl Pts',(84.202048378752,13.4426446636611,-16.4091512824603));
#29183=CARTESIAN_POINT('Ctrl Pts',(84.3209032424958,19.646911372201,-7.99773811130408));
#29184=CARTESIAN_POINT('Ctrl Pts',(84.4397581062396,21.0812001429395,2.35540694943616));
#29185=CARTESIAN_POINT('Ctrl Pts',(84.5586129699833,17.3972869897626,12.136694227011));
#29186=CARTESIAN_POINT('Ctrl Pts',(84.677467833727,9.48957124763614,18.9713726150788));
#29187=CARTESIAN_POINT('Ctrl Pts',(84.7963226974708,-0.722071286488033,
21.2000838305266));
#29188=CARTESIAN_POINT('Ctrl Pts',(84.9151775612145,-10.7584056492251,18.2817299304756));
#29189=CARTESIAN_POINT('Ctrl Pts',(85.0340324249582,-18.1827590944255,10.9248438468571));
#29190=CARTESIAN_POINT('Ctrl Pts',(85.1528872887019,-21.1926090033863,0.91556812620056));
#29191=CARTESIAN_POINT('Ctrl Pts',(85.2717421524458,-19.0572085737298,-9.31599392128854));
#29192=CARTESIAN_POINT('Ctrl Pts',(85.3905970161894,-12.2950012770463,-17.2857711705771));
#29193=CARTESIAN_POINT('Ctrl Pts',(85.5094518799332,-2.54775049308316,-21.0588202136093));
#29194=CARTESIAN_POINT('Ctrl Pts',(85.6283067436769,7.81805622635515,-19.7191008467849));
#29195=CARTESIAN_POINT('Ctrl Pts',(85.7471616074207,16.2857551460622,-13.591877011165));
#29196=CARTESIAN_POINT('Ctrl Pts',(85.8660164711643,20.7995148803425,-4.16474754415393));
#29197=CARTESIAN_POINT('Ctrl Pts',(85.9848713349081,20.2634616838949,6.27352069809667));
#29198=CARTESIAN_POINT('Ctrl Pts',(86.1037261986518,14.8077413018752,15.1886714001213));
#29199=CARTESIAN_POINT('Ctrl Pts',(86.2225810623957,5.75692151819817,20.4162385369449));
#29200=CARTESIAN_POINT('Ctrl Pts',(86.3414359261392,-4.691593206492,20.6870465400193));
#29201=CARTESIAN_POINT('Ctrl Pts',(86.4602907898831,-14.0010588631557,15.9353472530277));
#29202=CARTESIAN_POINT('Ctrl Pts',(86.5791456536268,-19.9112756191699,7.31478260658337));
#29203=CARTESIAN_POINT('Ctrl Pts',(86.6980005173706,-20.9873307292317,-3.08170248823144));
#29204=CARTESIAN_POINT('Ctrl Pts',(86.8168553811143,-16.9679740132177,-12.7299960428468));
#29205=CARTESIAN_POINT('Ctrl Pts',(86.9357102448579,-8.8290455152107,-19.2876358492809));
#29206=CARTESIAN_POINT('Ctrl Pts',(87.0545651086018,1.45344394877011,-21.1625244725649));
#29207=CARTESIAN_POINT('Ctrl Pts',(87.1734199723454,11.3830588342422,-17.8994668339676));
#29208=CARTESIAN_POINT('Ctrl Pts',(87.2922748360893,18.5490362972512,-10.2906848075035));
#29209=CARTESIAN_POINT('Ctrl Pts',(87.4111296998329,21.211583565601,-0.183477529011579));
#29210=CARTESIAN_POINT('Ctrl Pts',(87.5299845635768,18.7242737537734,9.96827536527145));
#29211=CARTESIAN_POINT('Ctrl Pts',(87.6488394273203,11.6909886985687,17.699879225974));
#29212=CARTESIAN_POINT('Ctrl Pts',(87.7676942910643,1.81930542866218,21.1342156022259));
#29213=CARTESIAN_POINT('Ctrl Pts',(87.8865491548078,-8.49407814682619,19.4374786893705));
#29214=CARTESIAN_POINT('Ctrl Pts',(88.0054040185517,-16.7452258525253,13.0216109799074));
#29215=CARTESIAN_POINT('Ctrl Pts',(88.1242588822953,-20.9308817174528,3.44428975176641));
#29216=CARTESIAN_POINT('Ctrl Pts',(88.2431137460392,-20.0348307369856,-6.96925381260139));
#29217=CARTESIAN_POINT('Ctrl Pts',(88.3619686097828,-14.2746207651856,-15.6907661818753));
#29218=CARTESIAN_POINT('Ctrl Pts',(88.4808234735266,-5.04874513070288,-20.6027938389252));
#29219=CARTESIAN_POINT('Ctrl Pts',(88.5996783372703,5.40289074826908,-20.5127695089313));
#29220=CARTESIAN_POINT('Ctrl Pts',(88.7185332010141,14.5427850928398,-15.44254976056));
#29221=CARTESIAN_POINT('Ctrl Pts',(88.8373880647577,20.151907463494,-6.62310855619352));
#29222=CARTESIAN_POINT('Ctrl Pts',(88.9562429285016,20.8684463545089,3.80432492214186));
#29223=CARTESIAN_POINT('Ctrl Pts',(89.0750977922453,16.5184367778662,13.3081248783771));
#29224=CARTESIAN_POINT('Ctrl Pts',(89.1939526559889,8.15799637548015,19.5809100019827));
#29225=CARTESIAN_POINT('Ctrl Pts',(89.3128075197329,-2.18308424000846,21.0997413386136));
#29226=CARTESIAN_POINT('Ctrl Pts',(89.4316623834764,-11.9941444638625,17.495869225592));
#29227=CARTESIAN_POINT('Ctrl Pts',(89.5505172472203,-18.8932047609022,9.64426022093586));
#29228=CARTESIAN_POINT('Ctrl Pts',(89.6693721109639,-21.2052758782399,-0.548831754892572));
#29229=CARTESIAN_POINT('Ctrl Pts',(89.7882269747077,-18.3690213275962,-10.6086755482063));
#29230=CARTESIAN_POINT('Ctrl Pts',(89.9070818384514,-11.0730415411467,-18.09289065306));
#29231=CARTESIAN_POINT('Ctrl Pts',(90.0259367021953,-1.08869191919774,-21.1844209685031));
#29232=CARTESIAN_POINT('Ctrl Pts',(90.1447915659388,9.15997590841173,-19.132688828153));
#29233=CARTESIAN_POINT('Ctrl Pts',(90.2636464296828,17.1847377989099,-12.4358244362435));
#29234=CARTESIAN_POINT('Ctrl Pts',(90.3825012934262,21.0373008687106,-2.71972659361109));
#29235=CARTESIAN_POINT('Ctrl Pts',(90.5013561571702,19.7823201346039,7.6566800423115));
#29236=CARTESIAN_POINT('Ctrl Pts',(90.6202110209137,13.7244861716685,16.1741593677076));
#29237=CARTESIAN_POINT('Ctrl Pts',(90.7390658846577,4.33455115709318,20.7647918261493));
#29238=CARTESIAN_POINT('Ctrl Pts',(90.8579207484012,-6.10774864533687,20.3140444991141));
#29239=CARTESIAN_POINT('Ctrl Pts',(90.9767756121453,-15.067177463825,14.9313435218322));
#29240=CARTESIAN_POINT('Ctrl Pts',(91.0956304758887,-20.368520489837,5.92354558627522));
#29241=CARTESIAN_POINT('Ctrl Pts',(91.2144853396326,-20.7246879402021,-4.5224232036684));
#29242=CARTESIAN_POINT('Ctrl Pts',(91.3333402033763,-16.0492126196877,-13.8703715024302));
#29243=CARTESIAN_POINT('Ctrl Pts',(91.45219506712,-7.47722065097378,-19.8508851425969));
#29244=CARTESIAN_POINT('Ctrl Pts',(91.5710499308638,2.91011658725582,-21.0117313519411));
#29245=CARTESIAN_POINT('Ctrl Pts',(91.6899047946075,12.5909457871538,-17.0715713856038));
#29246=CARTESIAN_POINT('Ctrl Pts',(91.8087596583513,19.2148315676077,-8.98603862815482));
#29247=CARTESIAN_POINT('Ctrl Pts',(91.9276145220949,21.1737367581028,1.27988551323374));
#29248=CARTESIAN_POINT('Ctrl Pts',(92.0464693858387,17.9918043030239,11.2377002096187));
#29249=CARTESIAN_POINT('Ctrl Pts',(92.1257059616679,12.9584843859408,16.0530817204229));
#29250=CARTESIAN_POINT('Ctrl Pts',(92.1653242495824,10.0185191914685,17.7156819936512));
#29251=CARTESIAN_POINT('Ctrl Pts',(68.5596757504176,-8.87789851314185,18.6316073330471));
#29252=CARTESIAN_POINT('Ctrl Pts',(68.5992940383321,-11.9698639873395,17.1582961368962));
#29253=CARTESIAN_POINT('Ctrl Pts',(68.6785306141613,-17.4030844278904,12.6441725683155));
#29254=CARTESIAN_POINT('Ctrl Pts',(68.797385477905,-21.3282549068603,2.79670685859421));
#29255=CARTESIAN_POINT('Ctrl Pts',(68.9162403416488,-20.0748846690222,-7.72711152354461));
#29256=CARTESIAN_POINT('Ctrl Pts',(69.0350952053924,-13.9478180011767,-16.376195467809));
#29257=CARTESIAN_POINT('Ctrl Pts',(69.1539500691362,-4.43433290333388,-21.0487295098283));
#29258=CARTESIAN_POINT('Ctrl Pts',(69.27280493288,6.15569360820102,-20.611276820841));
#29259=CARTESIAN_POINT('Ctrl Pts',(69.3916597966237,15.2512340085775,-15.1695438678658));
#29260=CARTESIAN_POINT('Ctrl Pts',(69.5105146603674,20.6439889763955,-6.04495705340727));
#29261=CARTESIAN_POINT('Ctrl Pts',(69.6293695241112,21.024696797449,4.54729910049925));
#29262=CARTESIAN_POINT('Ctrl Pts',(69.7482243878549,16.3009176077266,14.0355164455145));
#29263=CARTESIAN_POINT('Ctrl Pts',(69.8670792515987,7.6195196700065,20.1161303953526));
#29264=CARTESIAN_POINT('Ctrl Pts',(69.9859341153423,-2.91178518690343,21.312841260998));
#29265=CARTESIAN_POINT('Ctrl Pts',(70.1047889790862,-12.7361514688866,17.3351141057232));
#29266=CARTESIAN_POINT('Ctrl Pts',(70.2236438428299,-19.4683697749204,9.1486775269705));
#29267=CARTESIAN_POINT('Ctrl Pts',(70.3424987065736,-21.4739572771565,-1.25892116139127));
#29268=CARTESIAN_POINT('Ctrl Pts',(70.4613535703174,-18.2659873199027,-11.3608728960612));
#29269=CARTESIAN_POINT('Ctrl Pts',(70.580208434061,-10.6233072221335,-18.7045734285684));
#29270=CARTESIAN_POINT('Ctrl Pts',(70.6990632978048,-0.401446110656565,
-21.507081763208));
#29271=CARTESIAN_POINT('Ctrl Pts',(70.8179181615486,9.91788015453811,-19.0879903986521));
#29272=CARTESIAN_POINT('Ctrl Pts',(70.9367730252922,17.8292925901796,-12.0346188234338));
#29273=CARTESIAN_POINT('Ctrl Pts',(71.055627889036,21.4120179027988,-2.05942073577562));
#29274=CARTESIAN_POINT('Ctrl Pts',(71.1744827527798,19.7962236575869,8.41577407693337));
#29275=CARTESIAN_POINT('Ctrl Pts',(71.2933376165234,13.3742006724056,16.8477440870536));
#29276=CARTESIAN_POINT('Ctrl Pts',(71.4121924802673,3.70512063385281,21.1893323517497));
#29277=CARTESIAN_POINT('Ctrl Pts',(71.531047344011,-6.86350760049681,20.3864658009993));
#29278=CARTESIAN_POINT('Ctrl Pts',(71.6499022077547,-15.7657782477023,14.6340684936305));
#29279=CARTESIAN_POINT('Ctrl Pts',(71.7687570714985,-20.8403523684772,5.32873696021297));
#29280=CARTESIAN_POINT('Ctrl Pts',(71.8876119352421,-20.8551988236627,-5.27033267062336));
#29281=CARTESIAN_POINT('Ctrl Pts',(72.006466798986,-15.8067131146762,-14.5898438971565));
#29282=CARTESIAN_POINT('Ctrl Pts',(72.1253216627296,-6.92059250228412,-20.3671579718622));
#29283=CARTESIAN_POINT('Ctrl Pts',(72.2441765264734,3.64574506263926,-21.1996289441932));
#29284=CARTESIAN_POINT('Ctrl Pts',(72.3630313902172,13.3269499374307,-16.8851452406709));
#29285=CARTESIAN_POINT('Ctrl Pts',(72.4818862539608,19.7725695349525,-8.47119934948849));
#29286=CARTESIAN_POINT('Ctrl Pts',(72.6007411177046,21.4177032612537,1.99942777968804));
#29287=CARTESIAN_POINT('Ctrl Pts',(72.7195959814483,17.8629371102081,11.9846235748171));
#29288=CARTESIAN_POINT('Ctrl Pts',(72.8384508451921,9.97131544503892,19.0601309735488));
#29289=CARTESIAN_POINT('Ctrl Pts',(72.9573057089358,-0.341193339873213,
21.5081219900329));
#29290=CARTESIAN_POINT('Ctrl Pts',(73.0761605726795,-10.5708654553014,18.7342608063202));
#29291=CARTESIAN_POINT('Ctrl Pts',(73.1950154364233,-18.2340886236142,11.4119996713763));
#29292=CARTESIAN_POINT('Ctrl Pts',(73.313870300167,-21.4703462092543,1.31907470905424));
#29293=CARTESIAN_POINT('Ctrl Pts',(73.4327251639108,-19.4939229925569,-9.0941019784017));
#29294=CARTESIAN_POINT('Ctrl Pts',(73.5515800276545,-12.7846651417468,-17.2993659319269));
#29295=CARTESIAN_POINT('Ctrl Pts',(73.6704348913983,-2.97148069845482,-21.3046010732898));
#29296=CARTESIAN_POINT('Ctrl Pts',(73.7892897551418,7.56313507344221,-20.1373958667494));
#29297=CARTESIAN_POINT('Ctrl Pts',(73.9081446188858,16.2615341109381,-14.081130380481));
#29298=CARTESIAN_POINT('Ctrl Pts',(74.0269994826293,21.0118744701763,-4.60617581979471));
#29299=CARTESIAN_POINT('Ctrl Pts',(74.1458543463733,20.6608441479951,5.98708973755754));
#29300=CARTESIAN_POINT('Ctrl Pts',(74.2647092101168,15.2936680869099,15.1267789327649));
#29301=CARTESIAN_POINT('Ctrl Pts',(74.3835640738608,6.21341682633891,20.5939111335238));
#29302=CARTESIAN_POINT('Ctrl Pts',(74.5024189376042,-4.37535964812074,21.0611479360197));
#29303=CARTESIAN_POINT('Ctrl Pts',(74.6212738013482,-13.9018638602333,16.4150511922701));
#29304=CARTESIAN_POINT('Ctrl Pts',(74.7401286650918,-20.0532022434075,7.78362410566604));
#29305=CARTESIAN_POINT('Ctrl Pts',(74.8589835288356,-21.3359213066685,-2.73755117376083));
#29306=CARTESIAN_POINT('Ctrl Pts',(74.9778383925793,-17.4385959350839,-12.5940897347202));
#29307=CARTESIAN_POINT('Ctrl Pts',(75.0966932563231,-9.30743877687657,-19.3929705782277));
#29308=CARTESIAN_POINT('Ctrl Pts',(75.2155481200667,1.08342611768035,-21.483526532691));
#29309=CARTESIAN_POINT('Ctrl Pts',(75.3344029838106,11.2112512610687,-18.3582016982736));
#29310=CARTESIAN_POINT('Ctrl Pts',(75.4532578475542,18.6171513060362,-10.7757784721784));
#29311=CARTESIAN_POINT('Ctrl Pts',(75.5721127112981,21.5030838450601,-0.577156465462027));
#29312=CARTESIAN_POINT('Ctrl Pts',(75.6909675750417,19.1683873705711,9.76159054893414));
#29313=CARTESIAN_POINT('Ctrl Pts',(75.8098224387856,12.1798914703757,17.7303685298185));
#29314=CARTESIAN_POINT('Ctrl Pts',(75.9286773025292,2.23429903231371,21.3944766766451));
#29315=CARTESIAN_POINT('Ctrl Pts',(76.047532166273,-8.25374798747288,19.8643240154957));
#29316=CARTESIAN_POINT('Ctrl Pts',(76.1663870300167,-16.7379077265277,13.5114088596102));
#29317=CARTESIAN_POINT('Ctrl Pts',(76.2852418937604,-21.1583523569849,3.87812454299523));
#29318=CARTESIAN_POINT('Ctrl Pts',(76.4040967575042,-20.4418636531854,-6.69671074617139));
#29319=CARTESIAN_POINT('Ctrl Pts',(76.5229516212479,-14.762394418451,-15.6456842441421));
#29320=CARTESIAN_POINT('Ctrl Pts',(76.6418064849916,-5.49883533106082,-20.7961182540201));
#29321=CARTESIAN_POINT('Ctrl Pts',(76.7606613487354,5.09975920876569,-20.8975639835345));
#29322=CARTESIAN_POINT('Ctrl Pts',(76.8795162124791,14.4602080445132,-15.9253919180253));
#29323=CARTESIAN_POINT('Ctrl Pts',(76.9983710762229,20.309933385781,-7.08677150036936));
#29324=CARTESIAN_POINT('Ctrl Pts',(77.1172259399665,21.2287089032783,3.4724116595216));
#29325=CARTESIAN_POINT('Ctrl Pts',(77.2360808037104,16.9934695632586,13.1885449021457));
#29326=CARTESIAN_POINT('Ctrl Pts',(77.354935667454,8.63246850080676,19.7026955520276));
#29327=CARTESIAN_POINT('Ctrl Pts',(77.4737905311979,-1.82436755155978,21.4333246947394));
#29328=CARTESIAN_POINT('Ctrl Pts',(77.5926453949414,-11.8382742901771,17.9602613083396));
#29329=CARTESIAN_POINT('Ctrl Pts',(77.7115002586854,-18.9780240625405,10.1267135396901));
#29330=CARTESIAN_POINT('Ctrl Pts',(77.830355122429,-21.510191789745,-0.165449695363124));
#29331=CARTESIAN_POINT('Ctrl Pts',(77.9492099861728,-18.82000480016,-10.4174442045669));
#29332=CARTESIAN_POINT('Ctrl Pts',(78.0680648499164,-11.5606004926255,-18.1402381650081));
#29333=CARTESIAN_POINT('Ctrl Pts',(78.1869197136603,-1.49445428796093,-21.4588520385995));
#29334=CARTESIAN_POINT('Ctrl Pts',(78.3057745774039,8.93452319575713,-19.5675757235736));
#29335=CARTESIAN_POINT('Ctrl Pts',(78.4246294411477,17.1943313010844,-12.9255829865371));
#29336=CARTESIAN_POINT('Ctrl Pts',(78.5434843048914,21.2796114407862,-3.14545089970743));
#29337=CARTESIAN_POINT('Ctrl Pts',(78.6623391686352,20.1985183437687,7.39834989370943));
#29338=CARTESIAN_POINT('Ctrl Pts',(78.7811940323789,14.2135253384747,16.1459413440607));
#29339=CARTESIAN_POINT('Ctrl Pts',(78.9000488961227,4.77769973163326,20.9735383211241));
#29340=CARTESIAN_POINT('Ctrl Pts',(79.0189037598663,-5.8180803271622,20.7090720637115));
#29341=CARTESIAN_POINT('Ctrl Pts',(79.1377586236102,-15.0013169955402,15.416751046593));
#29342=CARTESIAN_POINT('Ctrl Pts',(79.2566134873538,-20.5424569622484,6.38147211758228));
#29343=CARTESIAN_POINT('Ctrl Pts',(79.3754683510977,-21.096193838372,-4.2031333511018));
#29344=CARTESIAN_POINT('Ctrl Pts',(79.4943232148413,-16.5280885442806,-13.7672805414043));
#29345=CARTESIAN_POINT('Ctrl Pts',(79.6131780785851,-7.94720911909616,-19.9889367313688));
#29346=CARTESIAN_POINT('Ctrl Pts',(79.7320329423288,2.56313450771434,-21.357576312135));
#29347=CARTESIAN_POINT('Ctrl Pts',(79.8508878060726,12.4511871890527,-17.5409139447316));
#29348=CARTESIAN_POINT('Ctrl Pts',(79.9697426698162,19.3162767661114,-9.46557849939951));
#29349=CARTESIAN_POINT('Ctrl Pts',(80.08859753356,21.4916615712951,0.907858655423031));
#29350=CARTESIAN_POINT('Ctrl Pts',(80.2074523973037,18.4491905211904,11.0608812282804));
#29351=CARTESIAN_POINT('Ctrl Pts',(80.3263072610476,10.9275303461789,18.528486310723));
#29352=CARTESIAN_POINT('Ctrl Pts',(80.4451621247911,0.752828292041289,21.4976504296635));
#29353=CARTESIAN_POINT('Ctrl Pts',(80.5640169885351,-9.60464927708498,19.2475046875563));
#29354=CARTESIAN_POINT('Ctrl Pts',(80.6828718522786,-17.6302608198373,12.3243510116281));
#29355=CARTESIAN_POINT('Ctrl Pts',(80.8017267160225,-21.3755071919452,2.40902816928516));
#29356=CARTESIAN_POINT('Ctrl Pts',(80.9205815797661,-19.9310982648919,-8.09117089107204));
#29357=CARTESIAN_POINT('Ctrl Pts',(81.03943644351,-13.6477150482613,-16.6269539722335));
#29358=CARTESIAN_POINT('Ctrl Pts',(81.1582913072536,-4.05086955512668,-21.1259598664926));
#29359=CARTESIAN_POINT('Ctrl Pts',(81.2771461709974,6.5294668308414,-20.4958968415206));
#29360=CARTESIAN_POINT('Ctrl Pts',(81.3960010347411,15.5245457613914,-14.8897348309422));
#29361=CARTESIAN_POINT('Ctrl Pts',(81.5148558984849,20.7504958261696,-5.66856660906691));
#29362=CARTESIAN_POINT('Ctrl Pts',(81.6337107622285,20.9385340576752,4.92884529569403));
#29363=CARTESIAN_POINT('Ctrl Pts',(81.7525656259724,16.0430075693679,14.3296068530338));
#29364=CARTESIAN_POINT('Ctrl Pts',(81.8714204897161,7.25247739767545,20.2513529431867));
#29365=CARTESIAN_POINT('Ctrl Pts',(81.9902753534598,-3.29884644412353,21.2563716699582));
#29366=CARTESIAN_POINT('Ctrl Pts',(82.1091302172035,-13.0492594220944,17.1006594307994));
#29367=CARTESIAN_POINT('Ctrl Pts',(82.2279850809474,-19.6315062507484,8.79316136324904));
#29368=CARTESIAN_POINT('Ctrl Pts',(82.3468399446909,-21.4475152760204,-1.64918553176499));
#29369=CARTESIAN_POINT('Ctrl Pts',(82.4656948084348,-18.0563865100551,-11.6911347025345));
#29370=CARTESIAN_POINT('Ctrl Pts',(82.5845496721784,-10.2814355922152,-18.8946502110105));
#29371=CARTESIAN_POINT('Ctrl Pts',(82.7034045359223,-0.0103049942866093,
-21.5108256057363));
#29372=CARTESIAN_POINT('Ctrl Pts',(82.8222593996658,10.2633275030229,-18.9044924025747));
#29373=CARTESIAN_POINT('Ctrl Pts',(82.9411142634098,18.045176695038,-11.7084295479012));
#29374=CARTESIAN_POINT('Ctrl Pts',(83.0599691271533,21.445925311578,-1.66973409964801));
#29375=CARTESIAN_POINT('Ctrl Pts',(83.1788239908973,19.6399221566051,8.77434795958085));
#29376=CARTESIAN_POINT('Ctrl Pts',(83.2976788546409,13.0656379414501,17.0881488060073));
#29377=CARTESIAN_POINT('Ctrl Pts',(83.4165337183847,3.31921111602204,21.2532012177127));
#29378=CARTESIAN_POINT('Ctrl Pts',(83.5353885821283,-7.23307081275469,20.2582924021494));
#29379=CARTESIAN_POINT('Ctrl Pts',(83.6542434458721,-16.029270701674,14.3449714257563));
#29380=CARTESIAN_POINT('Ctrl Pts',(83.7730983096159,-20.9338020144214,4.94890469238559));
#29381=CARTESIAN_POINT('Ctrl Pts',(83.8919531733596,-20.7559174770939,-5.64868251164617));
#29382=CARTESIAN_POINT('Ctrl Pts',(84.0108080371033,-15.5388048102676,-14.8748535959758));
#29383=CARTESIAN_POINT('Ctrl Pts',(84.1296629008471,-6.54910139262988,-20.489631411579));
#29384=CARTESIAN_POINT('Ctrl Pts',(84.2485177645907,4.0306264600685,-21.1298313948007));
#29385=CARTESIAN_POINT('Ctrl Pts',(84.3673726283346,13.6317781424049,-16.6400225092864));
#29386=CARTESIAN_POINT('Ctrl Pts',(84.4862274920783,19.9233367920027,-8.11026359039845));
#29387=CARTESIAN_POINT('Ctrl Pts',(84.6050823558219,21.3778055222299,2.38854673117928));
#29388=CARTESIAN_POINT('Ctrl Pts',(84.7239372195658,17.6420609528783,12.3074534233625));
#29389=CARTESIAN_POINT('Ctrl Pts',(84.8427920833094,9.62308631604418,19.2382934322998));
#29390=CARTESIAN_POINT('Ctrl Pts',(84.9616469470533,-0.732230586070165,
21.4983618632242));
#29391=CARTESIAN_POINT('Ctrl Pts',(85.080501810797,-10.9097727899244,18.538947707611));
#29392=CARTESIAN_POINT('Ctrl Pts',(85.1993566745406,-18.4385843852619,11.0785527168889));
#29393=CARTESIAN_POINT('Ctrl Pts',(85.3182115382845,-21.4907818677859,0.92844986108743));
#29394=CARTESIAN_POINT('Ctrl Pts',(85.4370664020281,-19.3253370739528,-9.44706681522981));
#29395=CARTESIAN_POINT('Ctrl Pts',(85.555921265772,-12.4679878002247,-17.5289761437101));
#29396=CARTESIAN_POINT('Ctrl Pts',(85.6747761295156,-2.58359648364417,-21.3551107148385));
#29397=CARTESIAN_POINT('Ctrl Pts',(85.7936309932594,7.92805364190112,-19.9965419481581));
#29398=CARTESIAN_POINT('Ctrl Pts',(85.9124858570031,16.5148902308474,-13.7831101387303));
#29399=CARTESIAN_POINT('Ctrl Pts',(86.0313407207469,21.0921570429475,-4.22334413811475));
#29400=CARTESIAN_POINT('Ctrl Pts',(86.1501955844906,20.5485617587358,6.36178701944117));
#29401=CARTESIAN_POINT('Ctrl Pts',(86.2690504482343,15.0160812301286,15.402370886441));
#29402=CARTESIAN_POINT('Ctrl Pts',(86.3879053119781,5.83791946323322,20.7034881306052));
#29403=CARTESIAN_POINT('Ctrl Pts',(86.5067601757217,-4.75760234131602,20.9781063109904));
#29404=CARTESIAN_POINT('Ctrl Pts',(86.6256150394656,-14.1980490414384,16.1595522168846));
#29405=CARTESIAN_POINT('Ctrl Pts',(86.7444699032092,-20.1914205548062,7.41769913195866));
#29406=CARTESIAN_POINT('Ctrl Pts',(86.8633247669531,-21.2826153975157,-3.12506100336263));
#29407=CARTESIAN_POINT('Ctrl Pts',(86.9821796306967,-17.2067076874798,-12.9091027957381));
#29408=CARTESIAN_POINT('Ctrl Pts',(87.1010344944405,-8.95326720923453,-19.559006383591));
#29409=CARTESIAN_POINT('Ctrl Pts',(87.2198893581841,1.47389341515622,-21.4602740577577));
#29410=CARTESIAN_POINT('Ctrl Pts',(87.338744221928,11.5432146346768,-18.1513062982005));
#29411=CARTESIAN_POINT('Ctrl Pts',(87.4575990856716,18.810014984855,-10.435471273634));
#29412=CARTESIAN_POINT('Ctrl Pts',(87.5764539494155,21.5100233956944,-0.186058995992359));
#29413=CARTESIAN_POINT('Ctrl Pts',(87.6953088131591,18.9877179733158,10.1085256392378));
#29414=CARTESIAN_POINT('Ctrl Pts',(87.814163676903,11.8554769683876,17.9489105598457));
#29415=CARTESIAN_POINT('Ctrl Pts',(87.9330185406465,1.84490244273418,21.4315668911563));
#29416=CARTESIAN_POINT('Ctrl Pts',(88.0518734043905,-8.61358696289824,19.710957461927));
#29417=CARTESIAN_POINT('Ctrl Pts',(88.1707282681339,-16.9808255352575,13.2048206566564));
#29418=CARTESIAN_POINT('Ctrl Pts',(88.289583131878,-21.2253721671706,3.49274974746314));
#29419=CARTESIAN_POINT('Ctrl Pts',(88.4084379956215,-20.3167140514776,-7.06730886432714));
#29420=CARTESIAN_POINT('Ctrl Pts',(88.5272928593654,-14.475459867209,-15.9115299725123));
#29421=CARTESIAN_POINT('Ctrl Pts',(88.646147723109,-5.11977927270044,-20.8926682027945));
#29422=CARTESIAN_POINT('Ctrl Pts',(88.7650025868529,5.4789075997191,-20.8013772608259));
#29423=CARTESIAN_POINT('Ctrl Pts',(88.8838574505964,14.7473971765519,-15.6598212298257));
#29424=CARTESIAN_POINT('Ctrl Pts',(89.0027123143403,20.4354380080601,-6.71629346085131));
#29425=CARTESIAN_POINT('Ctrl Pts',(89.121567178084,21.1620583597178,3.85785049131365));
#29426=CARTESIAN_POINT('Ctrl Pts',(89.2404220418277,16.7508456147713,13.4953657090902));
#29427=CARTESIAN_POINT('Ctrl Pts',(89.3592769055715,8.27277663432653,19.8564068047553));
#29428=CARTESIAN_POINT('Ctrl Pts',(89.4781317693152,-2.21379949932195,21.3966075862766));
#29429=CARTESIAN_POINT('Ctrl Pts',(89.596986633059,-12.1628980331017,17.7420302075325));
#29430=CARTESIAN_POINT('Ctrl Pts',(89.7158414968027,-19.1590257827662,9.77995171105074));
#29431=CARTESIAN_POINT('Ctrl Pts',(89.8346963605465,-21.5036269612985,-0.556553632666229));
#29432=CARTESIAN_POINT('Ctrl Pts',(89.9535512242901,-18.627467265262,-10.7579360368601));
#29433=CARTESIAN_POINT('Ctrl Pts',(90.072406088034,-11.228835502778,-18.347451525222));
#29434=CARTESIAN_POINT('Ctrl Pts',(90.1912609517776,-1.10400944748999,-21.4824786300121));
#29435=CARTESIAN_POINT('Ctrl Pts',(90.3101158155213,9.28885368150731,-19.4018793101104));
#29436=CARTESIAN_POINT('Ctrl Pts',(90.4289706792652,17.426521266563,-12.6107922937986));
#29437=CARTESIAN_POINT('Ctrl Pts',(90.5478255430088,21.3332886000114,-2.75799222993136));
#29438=CARTESIAN_POINT('Ctrl Pts',(90.6666804067526,20.0606507100447,7.76440694934979));
#29439=CARTESIAN_POINT('Ctrl Pts',(90.7855352704963,13.917585065418,16.4017243375116));
#29440=CARTESIAN_POINT('Ctrl Pts',(90.90439013424,4.39553683064526,21.0569454470874));
#29441=CARTESIAN_POINT('Ctrl Pts',(91.0232449979838,-6.19368260978275,20.5998562571131));
#29442=CARTESIAN_POINT('Ctrl Pts',(91.1420998617275,-15.279167571418,15.1414224916527));
#29443=CARTESIAN_POINT('Ctrl Pts',(91.2609547254712,-20.6550987066608,6.00688787577717));
#29444=CARTESIAN_POINT('Ctrl Pts',(91.3798095892151,-21.0162773129844,-4.58605217358187));
#29445=CARTESIAN_POINT('Ctrl Pts',(91.4986644529586,-16.2750196308681,-14.0655229536038));
#29446=CARTESIAN_POINT('Ctrl Pts',(91.6175193167026,-7.58242262487387,-20.1301804045861));
#29447=CARTESIAN_POINT('Ctrl Pts',(91.7363741804461,2.95106094660392,-21.3073593287609));
#29448=CARTESIAN_POINT('Ctrl Pts',(91.85522904419,12.768096149823,-17.3117626399715));
#29449=CARTESIAN_POINT('Ctrl Pts',(91.9740839079336,19.4851777702179,-9.11246916235354));
#29450=CARTESIAN_POINT('Ctrl Pts',(92.0929387716774,21.4716440963733,1.29789307094044));
#29451=CARTESIAN_POINT('Ctrl Pts',(92.2117936354211,18.2449429243184,11.3958108632069));
#29452=CARTESIAN_POINT('Ctrl Pts',(92.2910302112503,13.1408058927933,16.2789431685464));
#29453=CARTESIAN_POINT('Ctrl Pts',(92.3306484991649,10.1594763791317,17.9649356671368));
#29454=CARTESIAN_POINT('Ctrl Pts',(68.725,-9.00107450765883,18.890110711893));
#29455=CARTESIAN_POINT('Ctrl Pts',(68.7646182879146,-12.1359393145907,17.3963581273268));
#29456=CARTESIAN_POINT('Ctrl Pts',(68.8438548637437,-17.6445427222035,12.8196035589538));
#29457=CARTESIAN_POINT('Ctrl Pts',(68.9627097274875,-21.6241727984171,2.8355096392489));
#29458=CARTESIAN_POINT('Ctrl Pts',(69.0815645912312,-20.353412732872,-7.83432097691324));
#29459=CARTESIAN_POINT('Ctrl Pts',(69.2004194549749,-14.1413363604027,-16.6034062384847));
#29460=CARTESIAN_POINT('Ctrl Pts',(69.3192743187187,-4.49585685121175,-21.3407691391228));
#29461=CARTESIAN_POINT('Ctrl Pts',(69.4381291824624,6.24110049599202,-20.897247032926));
#29462=CARTESIAN_POINT('Ctrl Pts',(69.5569840462062,15.4628365532379,-15.3800130064269));
#29463=CARTESIAN_POINT('Ctrl Pts',(69.6758389099499,20.9304130517779,-6.12882753196297));
#29464=CARTESIAN_POINT('Ctrl Pts',(69.7946937736936,21.3164029859812,4.61039039268297));
#29465=CARTESIAN_POINT('Ctrl Pts',(69.9135486374374,16.5270839391956,14.2302515727719));
#29466=CARTESIAN_POINT('Ctrl Pts',(70.0324035011811,7.72523634515273,20.395230721135));
#29467=CARTESIAN_POINT('Ctrl Pts',(70.1512583649248,-2.95218461653034,21.6085452966344));
#29468=CARTESIAN_POINT('Ctrl Pts',(70.2701132286686,-12.9128586165496,17.5756293489283));
#29469=CARTESIAN_POINT('Ctrl Pts',(70.3889680924123,-19.7384827757731,9.27561043245846));
#29470=CARTESIAN_POINT('Ctrl Pts',(70.507822956156,-21.7718967095473,-1.27638800513175));
#29471=CARTESIAN_POINT('Ctrl Pts',(70.6266778198999,-18.5194179206956,-11.5184988044314));
#29472=CARTESIAN_POINT('Ctrl Pts',(70.7455326836434,-10.7706998094906,-18.96408917215));
#29473=CARTESIAN_POINT('Ctrl Pts',(70.8643875473874,-0.40701595625145,-21.8054807797568));
#29474=CARTESIAN_POINT('Ctrl Pts',(70.9832424111309,10.0554853264971,-19.3528258433471));
#29475=CARTESIAN_POINT('Ctrl Pts',(71.1020972748748,18.0766642900339,-12.2015925886796));
#29476=CARTESIAN_POINT('Ctrl Pts',(71.2209521386185,21.7090979601895,-2.08799407403611));
#29477=CARTESIAN_POINT('Ctrl Pts',(71.3398070023622,20.0708854520526,8.53253834721895));
#29478=CARTESIAN_POINT('Ctrl Pts',(71.458661866106,13.5597604043912,17.0814973373548));
#29479=CARTESIAN_POINT('Ctrl Pts',(71.5775167298496,3.75652715964321,21.4833227687064));
#29480=CARTESIAN_POINT('Ctrl Pts',(71.6963715935935,-6.95873502096286,20.6693168829313));
#29481=CARTESIAN_POINT('Ctrl Pts',(71.8152264573371,-15.9845198127382,14.8371082037448));
#29482=CARTESIAN_POINT('Ctrl Pts',(71.934081321081,-21.1295008787099,5.40267027603342));
#29483=CARTESIAN_POINT('Ctrl Pts',(72.0529361848246,-21.1445533203548,-5.34345565881458));
#29484=CARTESIAN_POINT('Ctrl Pts',(72.1717910485684,-16.0260226286409,-14.7922700151415));
#29485=CARTESIAN_POINT('Ctrl Pts',(72.290645912312,-7.01661194459403,-20.6497411682071));
#29486=CARTESIAN_POINT('Ctrl Pts',(72.4095007760559,3.69632778479824,-21.4937622207481));
#29487=CARTESIAN_POINT('Ctrl Pts',(72.5283556397995,13.5118540912674,-17.1194174115574));
#29488=CARTESIAN_POINT('Ctrl Pts',(72.6472105035433,20.0469031413818,-8.58873261516847));
#29489=CARTESIAN_POINT('Ctrl Pts',(72.766065367287,21.7148621998888,2.02716874843905));
#29490=CARTESIAN_POINT('Ctrl Pts',(72.8849202310308,18.1107756094078,12.1509036832859));
#29491=CARTESIAN_POINT('Ctrl Pts',(73.0037750947745,10.1096620024779,19.3245798839318));
#29492=CARTESIAN_POINT('Ctrl Pts',(73.1226299585183,-0.345927211171586,
21.8065354391609));
#29493=CARTESIAN_POINT('Ctrl Pts',(73.2414848222619,-10.717530441777,18.9941884460587));
#29494=CARTESIAN_POINT('Ctrl Pts',(73.3603396860058,-18.4870766474128,11.5703349358388));
#29495=CARTESIAN_POINT('Ctrl Pts',(73.4791945497494,-21.7682355400497,1.33737615042459));
#29496=CARTESIAN_POINT('Ctrl Pts',(73.5980494134933,-19.7643905303522,-9.22027767795157));
#29497=CARTESIAN_POINT('Ctrl Pts',(73.7169042772369,-12.9620453901322,-17.5393851887391));
#29498=CARTESIAN_POINT('Ctrl Pts',(73.8357591409807,-3.01270837071065,-21.6001907808208));
#29499=CARTESIAN_POINT('Ctrl Pts',(73.9546140047244,7.66806944309719,-20.4167912393365));
#29500=CARTESIAN_POINT('Ctrl Pts',(74.0734688684682,16.4871540178927,-14.2764983761808));
#29501=CARTESIAN_POINT('Ctrl Pts',(74.1923237322118,21.3034027559186,-4.67008399431189));
#29502=CARTESIAN_POINT('Ctrl Pts',(74.3111785959557,20.9475020796805,6.07015733870148));
#29503=CARTESIAN_POINT('Ctrl Pts',(74.4300334596993,15.5058593812382,15.3366547312012));
#29504=CARTESIAN_POINT('Ctrl Pts',(74.5488883234433,6.29962459226462,20.879640406179));
#29505=CARTESIAN_POINT('Ctrl Pts',(74.6677431871866,-4.43606537428203,21.3533598641971));
#29506=CARTESIAN_POINT('Ctrl Pts',(74.7865980509307,-14.0947446308446,16.6428010649075));
#29507=CARTESIAN_POINT('Ctrl Pts',(74.9054529146743,-20.3314294754405,7.89161764025565));
#29508=CARTESIAN_POINT('Ctrl Pts',(75.0243077784181,-21.6319455653368,-2.77553320158754));
#29509=CARTESIAN_POINT('Ctrl Pts',(75.1431626421617,-17.68054693217,-12.7688258533877));
#29510=CARTESIAN_POINT('Ctrl Pts',(75.2620175059056,-9.43657440802294,-19.6620374563944));
#29511=CARTESIAN_POINT('Ctrl Pts',(75.3808723696492,1.09845806351002,-21.7815987332776));
#29512=CARTESIAN_POINT('Ctrl Pts',(75.4997272333931,11.3668012509472,-18.6129117232171));
#29513=CARTESIAN_POINT('Ctrl Pts',(75.6185820971367,18.8754541154003,-10.9252865148803));
#29514=CARTESIAN_POINT('Ctrl Pts',(75.7374369608804,21.8014273926774,-0.585164196291588));
#29515=CARTESIAN_POINT('Ctrl Pts',(75.8562918246243,19.4343382793545,9.89702728794988));
#29516=CARTESIAN_POINT('Ctrl Pts',(75.9751466883679,12.3488808142786,17.976367712348));
#29517=CARTESIAN_POINT('Ctrl Pts',(76.0940015521117,2.26529871145472,21.6913133591005));
#29518=CARTESIAN_POINT('Ctrl Pts',(76.2128564158553,-8.36826423423381,20.1399306652444));
#29519=CARTESIAN_POINT('Ctrl Pts',(76.3317112795992,-16.9701370572975,13.6988722802772));
#29520=CARTESIAN_POINT('Ctrl Pts',(76.4505661433428,-21.4519129434293,3.93193140356445));
#29521=CARTESIAN_POINT('Ctrl Pts',(76.5694210070867,-20.7254833500691,-6.78962395135514));
#29522=CARTESIAN_POINT('Ctrl Pts',(76.6882758708304,-14.967214580706,-15.8627595704502));
#29523=CARTESIAN_POINT('Ctrl Pts',(76.807130734574,-5.57512866890268,-21.0846530400666));
#29524=CARTESIAN_POINT('Ctrl Pts',(76.9259855983179,5.17051558330714,-21.1875062736884));
#29525=CARTESIAN_POINT('Ctrl Pts',(77.0448404620615,14.6608355358242,-16.1463480355876));
#29526=CARTESIAN_POINT('Ctrl Pts',(77.1636953258054,20.5917226222387,-7.1850965855436));
#29527=CARTESIAN_POINT('Ctrl Pts',(77.2825501895489,21.5232456483878,3.52058947535276));
#29528=CARTESIAN_POINT('Ctrl Pts',(77.4014050532929,17.2292446749756,13.3715287616874));
#29529=CARTESIAN_POINT('Ctrl Pts',(77.5202599170364,8.75223928790795,19.9760596950952));
#29530=CARTESIAN_POINT('Ctrl Pts',(77.6391147807804,-1.8496796552288,21.7307003722347));
#29531=CARTESIAN_POINT('Ctrl Pts',(77.7579696445239,-12.0025238822286,18.2094501276491));
#29532=CARTESIAN_POINT('Ctrl Pts',(77.8768245082678,-19.2413337843638,10.2672161608446));
#29533=CARTESIAN_POINT('Ctrl Pts',(77.9956793720115,-21.8086339562139,-0.167745219550351));
#29534=CARTESIAN_POINT('Ctrl Pts',(78.1145342357552,-19.0811220909967,-10.5619805549569));
#29535=CARTESIAN_POINT('Ctrl Pts',(78.2333890994989,-11.7209975123465,-18.3919240649361));
#29536=CARTESIAN_POINT('Ctrl Pts',(78.3522439632427,-1.51518902523096,-21.7565818940529));
#29537=CARTESIAN_POINT('Ctrl Pts',(78.4710988269864,9.05848482682818,-19.8390651527972));
#29538=CARTESIAN_POINT('Ctrl Pts',(78.5899536907302,17.4328932597428,-13.1049183930775));
#29539=CARTESIAN_POINT('Ctrl Pts',(78.7088085544739,21.5748544308107,-3.18909231351752));
#29540=CARTESIAN_POINT('Ctrl Pts',(78.8276634182175,20.4787617573513,7.5009979589687));
#29541=CARTESIAN_POINT('Ctrl Pts',(78.9465182819614,14.4107302419287,16.3699574644887));
#29542=CARTESIAN_POINT('Ctrl Pts',(79.0653731457051,4.84398770677473,21.2645347137299));
#29543=CARTESIAN_POINT('Ctrl Pts',(79.1842280094488,-5.89880301501642,20.9963991313949));
#29544=CARTESIAN_POINT('Ctrl Pts',(79.3030828731926,-15.2094520781,15.6306500497832));
#29545=CARTESIAN_POINT('Ctrl Pts',(79.4219377369363,-20.8274723363712,6.47001155891541));
#29546=CARTESIAN_POINT('Ctrl Pts',(79.54079260068,-21.3888920093095,-4.26144953142791));
#29547=CARTESIAN_POINT('Ctrl Pts',(79.6596474644238,-16.7574067484584,-13.9582940419497));
#29548=CARTESIAN_POINT('Ctrl Pts',(79.7785023281675,-8.05747230642932,-20.2662723145114));
#29549=CARTESIAN_POINT('Ctrl Pts',(79.8973571919112,2.59869659953155,-21.6539010221805));
#29550=CARTESIAN_POINT('Ctrl Pts',(80.0162120556551,12.6239406129242,-17.7842845483357));
#29551=CARTESIAN_POINT('Ctrl Pts',(80.1350669193986,19.58427955951,-9.59690823285125));
#29552=CARTESIAN_POINT('Ctrl Pts',(80.2539217831425,21.7898466411006,0.920454698574115));
#29553=CARTESIAN_POINT('Ctrl Pts',(80.3727766468862,18.7051629663718,11.2143449160563));
#29554=CARTESIAN_POINT('Ctrl Pts',(80.49163151063,11.0791438632757,18.7855589416884));
#29555=CARTESIAN_POINT('Ctrl Pts',(80.6104863743736,0.763273373547416,21.7959185916089));
#29556=CARTESIAN_POINT('Ctrl Pts',(80.7293412381174,-9.73790854164409,19.5145533059146));
#29557=CARTESIAN_POINT('Ctrl Pts',(80.8481961018611,-17.8748710625499,12.4953446527907));
#29558=CARTESIAN_POINT('Ctrl Pts',(80.9670509656049,-21.6720806831577,2.44245211979913));
#29559=CARTESIAN_POINT('Ctrl Pts',(81.0859058293486,-20.2076313708922,-8.20343146938788));
#29560=CARTESIAN_POINT('Ctrl Pts',(81.2047606930923,-13.8370696428724,-16.8576438802434));
#29561=CARTESIAN_POINT('Ctrl Pts',(81.3236155568361,-4.10707315842005,-21.4190710248179));
#29562=CARTESIAN_POINT('Ctrl Pts',(81.4424704205798,6.62005961801551,-20.7802662193902));
#29563=CARTESIAN_POINT('Ctrl Pts',(81.5613252843235,15.7399403573933,-15.0963217718923));
#29564=CARTESIAN_POINT('Ctrl Pts',(81.6801801480674,21.0383976259396,-5.74721487571741));
#29565=CARTESIAN_POINT('Ctrl Pts',(81.799035011811,21.2290447852381,4.99723033301097));
#29566=CARTESIAN_POINT('Ctrl Pts',(81.9178898755548,16.2655955398741,14.5284223241216));
#29567=CARTESIAN_POINT('Ctrl Pts',(82.0367447392985,7.35310156169902,20.5323294079885));
#29568=CARTESIAN_POINT('Ctrl Pts',(82.1555996030423,-3.34461613735804,21.5512922208515));
#29569=CARTESIAN_POINT('Ctrl Pts',(82.274454466786,-13.2303107716506,17.3379217434027));
#29570=CARTESIAN_POINT('Ctrl Pts',(82.3933093305297,-19.9038826811303,8.91516167607796));
#29571=CARTESIAN_POINT('Ctrl Pts',(82.5121641942735,-21.7450878400829,-1.67206708055913));
#29572=CARTESIAN_POINT('Ctrl Pts',(82.6310190580172,-18.3069090140539,-11.853342813146));
#29573=CARTESIAN_POINT('Ctrl Pts',(82.749873921761,-10.4240848973699,-19.1568031661661));
#29574=CARTESIAN_POINT('Ctrl Pts',(82.8687287855046,-0.0104479704558075,
-21.809276566056));
#29575=CARTESIAN_POINT('Ctrl Pts',(82.9875836492484,10.4057255683271,-19.1667819127644));
#29576=CARTESIAN_POINT('Ctrl Pts',(83.1064385129921,18.295543668974,-11.8708776150491));
#29577=CARTESIAN_POINT('Ctrl Pts',(83.225293376736,21.743475815752,-1.69290074860202));
#29578=CARTESIAN_POINT('Ctrl Pts',(83.3441482404795,19.9124153530857,8.89608724670601));
#29579=CARTESIAN_POINT('Ctrl Pts',(83.4630031042234,13.2469165340196,17.3252375405224));
#29580=CARTESIAN_POINT('Ctrl Pts',(83.5818579679671,3.36526335796003,21.5480777803121));
#29581=CARTESIAN_POINT('Ctrl Pts',(83.7007128317108,-7.33342572100848,20.5393651481553));
#29582=CARTESIAN_POINT('Ctrl Pts',(83.8195676954546,-16.2516680806413,14.5440000719016));
#29583=CARTESIAN_POINT('Ctrl Pts',(83.9384225591982,-21.2242470874678,5.0175680428792));
#29584=CARTESIAN_POINT('Ctrl Pts',(84.0572774229421,-21.0438944993103,-5.72705489730169));
#29585=CARTESIAN_POINT('Ctrl Pts',(84.1761322866856,-15.7543972427872,-15.0812340679159));
#29586=CARTESIAN_POINT('Ctrl Pts',(84.2949871504297,-6.63996659862833,-20.7739138600291));
#29587=CARTESIAN_POINT('Ctrl Pts',(84.4138420141732,4.08654920147068,-21.4229962684674));
#29588=CARTESIAN_POINT('Ctrl Pts',(84.532696877917,13.8209116211488,-16.8708937361125));
#29589=CARTESIAN_POINT('Ctrl Pts',(84.6515517416606,20.1997622118043,-8.22278906949283));
#29590=CARTESIAN_POINT('Ctrl Pts',(84.7704066054046,21.6744109015202,2.42168651292241));
#29591=CARTESIAN_POINT('Ctrl Pts',(84.8892614691481,17.8868349159939,12.4782126197139));
#29592=CARTESIAN_POINT('Ctrl Pts',(85.008116332892,9.75660138445222,19.5052142495209));
#29593=CARTESIAN_POINT('Ctrl Pts',(85.1269711966357,-0.742389885652297,
21.7966398959218));
#29594=CARTESIAN_POINT('Ctrl Pts',(85.2458260603794,-11.0611399306238,18.7961654847464));
#29595=CARTESIAN_POINT('Ctrl Pts',(85.3646809241231,-18.6944096760982,11.2322615869207));
#29596=CARTESIAN_POINT('Ctrl Pts',(85.4835357878669,-21.7889547321855,0.9413315959743));
#29597=CARTESIAN_POINT('Ctrl Pts',(85.6023906516106,-19.5934655741757,-9.57813970917106));
#29598=CARTESIAN_POINT('Ctrl Pts',(85.7212455153544,-12.640974323403,-17.7721811168431));
#29599=CARTESIAN_POINT('Ctrl Pts',(85.8401003790981,-2.61944247420519,-21.6514012160677));
#29600=CARTESIAN_POINT('Ctrl Pts',(85.9589552428418,8.03805105744712,-20.2739830495313));
#29601=CARTESIAN_POINT('Ctrl Pts',(86.0778101065855,16.7440253156326,-13.9743432662956));
#29602=CARTESIAN_POINT('Ctrl Pts',(86.1966649703293,21.3847992055526,-4.28194073207559));
#29603=CARTESIAN_POINT('Ctrl Pts',(86.3155198340729,20.8336618335766,6.45005334078568));
#29604=CARTESIAN_POINT('Ctrl Pts',(86.4343746978168,15.2244211583821,15.6160703727607));
#29605=CARTESIAN_POINT('Ctrl Pts',(86.5532295615605,5.91891740826824,20.9907377242656));
#29606=CARTESIAN_POINT('Ctrl Pts',(86.6720844253043,-4.82361147614002,21.2691660819614));
#29607=CARTESIAN_POINT('Ctrl Pts',(86.7909392890479,-14.3950392197212,16.3837571807414));
#29608=CARTESIAN_POINT('Ctrl Pts',(86.9097941527918,-20.4715654904424,7.52061565733396));
#29609=CARTESIAN_POINT('Ctrl Pts',(87.0286490165353,-21.5779000657997,-3.16841951849384));
#29610=CARTESIAN_POINT('Ctrl Pts',(87.1475038802793,-17.445441361742,-13.0882095486293));
#29611=CARTESIAN_POINT('Ctrl Pts',(87.2663587440229,-9.07748890325836,-19.8303769179012));
#29612=CARTESIAN_POINT('Ctrl Pts',(87.3852136077667,1.49434288154233,-21.7580236429505));
#29613=CARTESIAN_POINT('Ctrl Pts',(87.5040684715103,11.7033704351114,-18.4031457624334));
#29614=CARTESIAN_POINT('Ctrl Pts',(87.6229233352542,19.0709936724587,-10.5802577397646));
#29615=CARTESIAN_POINT('Ctrl Pts',(87.7417781989977,21.8084632257878,-0.188640462973126));
#29616=CARTESIAN_POINT('Ctrl Pts',(87.8606330627418,19.2511621928582,10.2487759132041));
#29617=CARTESIAN_POINT('Ctrl Pts',(87.9794879264852,12.0199652382065,18.1979418937174));
#29618=CARTESIAN_POINT('Ctrl Pts',(88.0983427902292,1.87049945680621,21.7289181800866));
#29619=CARTESIAN_POINT('Ctrl Pts',(88.2171976539727,-8.73309577897031,19.9844362344835));
#29620=CARTESIAN_POINT('Ctrl Pts',(88.3360525177166,-17.2164252179897,13.3880303334053));
#29621=CARTESIAN_POINT('Ctrl Pts',(88.4549073814603,-21.5198626168885,3.54120974315988));
#29622=CARTESIAN_POINT('Ctrl Pts',(88.5737622452041,-20.5985973659696,-7.16536391605289));
#29623=CARTESIAN_POINT('Ctrl Pts',(88.6926171089477,-14.6762989692325,-16.1322937631492));
#29624=CARTESIAN_POINT('Ctrl Pts',(88.8114719726916,-5.19081341469801,-21.1825425666637));
#29625=CARTESIAN_POINT('Ctrl Pts',(88.9303268364351,5.55492445116913,-21.0899850127204));
#29626=CARTESIAN_POINT('Ctrl Pts',(89.0491817001791,14.9520092602641,-15.8770926990914));
#29627=CARTESIAN_POINT('Ctrl Pts',(89.1680365639226,20.7189685526261,-6.80947836550907));
#29628=CARTESIAN_POINT('Ctrl Pts',(89.2868914276666,21.4556703649268,3.91137606048543));
#29629=CARTESIAN_POINT('Ctrl Pts',(89.4057462914101,16.9832544516763,13.6826065398033));
#29630=CARTESIAN_POINT('Ctrl Pts',(89.524601155154,8.3875568931729,20.1319036075278));
#29631=CARTESIAN_POINT('Ctrl Pts',(89.6434560188976,-2.24451475863544,21.6934738339396));
#29632=CARTESIAN_POINT('Ctrl Pts',(89.7623108826415,-12.3316516023409,17.9881911894731));
#29633=CARTESIAN_POINT('Ctrl Pts',(89.881165746385,-19.4248468046303,9.91564320116563));
#29634=CARTESIAN_POINT('Ctrl Pts',(90.000020610129,-21.8019780443571,-0.564275510439895));
#29635=CARTESIAN_POINT('Ctrl Pts',(90.1188754738725,-18.8859132029279,-10.9071965255139));
#29636=CARTESIAN_POINT('Ctrl Pts',(90.2377303376164,-11.3846294644092,-18.6020123973841));
#29637=CARTESIAN_POINT('Ctrl Pts',(90.35658520136,-1.11932697578227,-21.7805362915212));
#29638=CARTESIAN_POINT('Ctrl Pts',(90.4754400651038,9.4177314546029,-19.6710697920678));
#29639=CARTESIAN_POINT('Ctrl Pts',(90.5942949288476,17.6683047342162,-12.7857601513537));
#29640=CARTESIAN_POINT('Ctrl Pts',(90.7131497925913,21.6292763313123,-2.79625786625162));
#29641=CARTESIAN_POINT('Ctrl Pts',(90.832004656335,20.3389812854855,7.87213385638809));
#29642=CARTESIAN_POINT('Ctrl Pts',(90.9508595200787,14.1106839591675,16.6292893073156));
#29643=CARTESIAN_POINT('Ctrl Pts',(91.0697143838226,4.45652250419733,21.3490990680254));
#29644=CARTESIAN_POINT('Ctrl Pts',(91.1885692475662,-6.27961657422861,20.885668015112));
#29645=CARTESIAN_POINT('Ctrl Pts',(91.30742411131,-15.4911576790111,15.3515014614732));
#29646=CARTESIAN_POINT('Ctrl Pts',(91.4262789750536,-20.9416769234847,6.0902301652791));
#29647=CARTESIAN_POINT('Ctrl Pts',(91.5451338387976,-21.3078666857667,-4.64968114349535));
#29648=CARTESIAN_POINT('Ctrl Pts',(91.6639887025411,-16.5008266420486,-14.2606744047774));
#29649=CARTESIAN_POINT('Ctrl Pts',(91.7828435662849,-7.68762459877395,-20.4094756665753));
#29650=CARTESIAN_POINT('Ctrl Pts',(91.9016984300287,2.99200530595202,-21.6029873055806));
#29651=CARTESIAN_POINT('Ctrl Pts',(92.0205532937724,12.9452465124921,-17.5519538943392));
#29652=CARTESIAN_POINT('Ctrl Pts',(92.1394081575161,19.7555239728282,-9.23889969655227));
#29653=CARTESIAN_POINT('Ctrl Pts',(92.2582630212599,21.7695514346438,1.31590062864715));
#29654=CARTESIAN_POINT('Ctrl Pts',(92.3771178850036,18.4980815456128,11.5539215167952));
#29655=CARTESIAN_POINT('Ctrl Pts',(92.4563544608328,13.3231273996458,16.5048046166698));
#29656=CARTESIAN_POINT('Ctrl Pts',(92.4959727487473,10.3004335667949,18.2141893406225));
#29657=CARTESIAN_POINT('',(92.,10.9270703901696,-17.8460909879584));
#29658=CARTESIAN_POINT('Ctrl Pts',(92.,10.9270703901696,-17.8460909879584));
#29659=CARTESIAN_POINT('Ctrl Pts',(92.,11.2921794592486,-17.6130173722224));
#29660=CARTESIAN_POINT('Ctrl Pts',(92.,11.6496215836174,-17.368828590994));
#29661=CARTESIAN_POINT('Ctrl Pts',(92.,11.99882582637,-17.1137755643941));
#29662=CARTESIAN_POINT('Ctrl Pts',(92.,12.1338901895175,-17.0151267784142));
#29663=CARTESIAN_POINT('Ctrl Pts',(92.,12.2677219209951,-16.9148522548055));
#29664=CARTESIAN_POINT('Ctrl Pts',(92.,12.4002868707347,-16.81296473787));
#29665=CARTESIAN_POINT('Ctrl Pts',(92.,12.7431657755325,-16.5494329348703));
#29666=CARTESIAN_POINT('Ctrl Pts',(92.,13.0775724354481,-16.2751130739695));
#29667=CARTESIAN_POINT('Ctrl Pts',(92.,13.4031395125407,-15.9905322322926));
#29668=CARTESIAN_POINT('Ctrl Pts',(92.,13.7291901755177,-15.7055286842437));
#29669=CARTESIAN_POINT('Ctrl Pts',(92.,14.0463753218874,-15.4102332180127));
#29670=CARTESIAN_POINT('Ctrl Pts',(92.,14.3542883269116,-15.1051388266276));
#29671=CARTESIAN_POINT('Ctrl Pts',(92.,14.5837985359634,-14.8777295376245));
#29672=CARTESIAN_POINT('Ctrl Pts',(92.,14.8081565673134,-14.6448753583735));
#29673=CARTESIAN_POINT('Ctrl Pts',(92.,15.0271787147356,-14.4067694678288));
#29674=CARTESIAN_POINT('Ctrl Pts',(92.,15.0614652272146,-14.3694955177577));
#29675=CARTESIAN_POINT('Ctrl Pts',(92.,15.0956222772878,-14.3320913486537));
#29676=CARTESIAN_POINT('Ctrl Pts',(92.,15.1296372996932,-14.2945708579953));
#29677=CARTESIAN_POINT('Ctrl Pts',(92.,15.419454141796,-13.9748865142016));
#29678=CARTESIAN_POINT('Ctrl Pts',(92.,15.6991446771822,-13.6465657021793));
#29679=CARTESIAN_POINT('Ctrl Pts',(92.,15.9683573898317,-13.3101384802151));
#29680=CARTESIAN_POINT('Ctrl Pts',(92.,16.24637517215,-12.9627078212336));
#29681=CARTESIAN_POINT('Ctrl Pts',(92.,16.5132191271701,-12.6066315155433));
#29682=CARTESIAN_POINT('Ctrl Pts',(92.,16.7684581893239,-12.2424555046393));
#29683=CARTESIAN_POINT('Ctrl Pts',(92.,17.0147113551117,-11.8911006029549));
#29684=CARTESIAN_POINT('Ctrl Pts',(92.,17.2501624348741,-11.5322056524719));
#29685=CARTESIAN_POINT('Ctrl Pts',(92.,17.4743799650063,-11.1662337083294));
#29686=CARTESIAN_POINT('Ctrl Pts',(92.,17.6967831806401,-10.8032231214182));
#29687=CARTESIAN_POINT('Ctrl Pts',(92.,17.9081341661192,-10.4332491691195));
#29688=CARTESIAN_POINT('Ctrl Pts',(92.,18.1079647220086,-10.0567440255743));
#29689=CARTESIAN_POINT('Ctrl Pts',(92.,18.1292790880992,-10.0165851598352));
#29690=CARTESIAN_POINT('Ctrl Pts',(92.,18.150463115333,-9.97635049241957));
#29691=CARTESIAN_POINT('Ctrl Pts',(92.,18.1715137789144,-9.93604517955553));
#29692=CARTESIAN_POINT('Ctrl Pts',(92.,18.3728227038647,-9.55060273632429));
#29693=CARTESIAN_POINT('Ctrl Pts',(92.,18.5615730281604,-9.15940492952969));
#29694=CARTESIAN_POINT('Ctrl Pts',(92.,18.7374063270933,-8.76297535539794));
#29695=CARTESIAN_POINT('Ctrl Pts',(92.,18.910632580253,-8.37242356466628));
#29696=CARTESIAN_POINT('Ctrl Pts',(92.,19.0713223953422,-7.97679356884877));
#29697=CARTESIAN_POINT('Ctrl Pts',(92.,19.219457689155,-7.57672924718513));
#29698=CARTESIAN_POINT('Ctrl Pts',(92.,19.3682726495474,-7.17482937139957));
#29699=CARTESIAN_POINT('Ctrl Pts',(92.,19.504417731036,-6.7684538540207));
#29700=CARTESIAN_POINT('Ctrl Pts',(92.,19.6278254352608,-6.35823462134573));
#29701=CARTESIAN_POINT('Ctrl Pts',(92.,19.7514283151323,-5.94736660580445));
#29702=CARTESIAN_POINT('Ctrl Pts',(92.,19.8622535912408,-5.53264216214906));
#29703=CARTESIAN_POINT('Ctrl Pts',(92.,19.9601827265672,-5.11468346047855));
#29704=CARTESIAN_POINT('Ctrl Pts',(92.,20.0577509900072,-4.6982649495247));
#29705=CARTESIAN_POINT('Ctrl Pts',(92.,20.1425180399432,-4.2786354299643));
#29706=CARTESIAN_POINT('Ctrl Pts',(92.,20.214315269712,-3.85640572218818));
#29707=CARTESIAN_POINT('Ctrl Pts',(92.,20.2856986963168,-3.4366095343343));
#29708=CARTESIAN_POINT('Ctrl Pts',(92.,20.3442614197365,-3.01424251934551));
#29709=CARTESIAN_POINT('Ctrl Pts',(92.,20.3897861214498,-2.58990850333));
#29710=CARTESIAN_POINT('Ctrl Pts',(92.,20.3963829166491,-2.52842002576895));
#29711=CARTESIAN_POINT('Ctrl Pts',(92.,20.402705853733,-2.46689025967155));
#29712=CARTESIAN_POINT('Ctrl Pts',(92.,20.4087541799555,-2.40532105860444));
#29713=CARTESIAN_POINT('Ctrl Pts',(92.,20.4124617649804,-2.36757953483858));
#29714=CARTESIAN_POINT('Ctrl Pts',(92.,20.416066161468,-2.3298231930452));
#29715=CARTESIAN_POINT('Ctrl Pts',(92.,20.4195671916806,-2.29205246118946));
#29716=CARTESIAN_POINT('Ctrl Pts',(92.,20.4231789043748,-2.25308763557207));
#29717=CARTESIAN_POINT('Ctrl Pts',(92.,20.4266797049764,-2.21411724628959));
#29718=CARTESIAN_POINT('Ctrl Pts',(92.,20.4300694323654,-2.17514335803996));
#29719=CARTESIAN_POINT('Ctrl Pts',(92.,20.4671268176833,-1.74907063051458));
#29720=CARTESIAN_POINT('Ctrl Pts',(92.,20.4909193423328,-1.32251843100026));
#29721=CARTESIAN_POINT('Ctrl Pts',(92.,20.5014010397203,-0.896104986036221));
#29722=CARTESIAN_POINT('Ctrl Pts',(92.,20.5118795350299,-0.469821807097898));
#29723=CARTESIAN_POINT('Ctrl Pts',(92.,20.509055396132,-0.0436767532038229));
#29724=CARTESIAN_POINT('Ctrl Pts',(92.,20.4928314192176,0.381720490806974));
#29725=CARTESIAN_POINT('Ctrl Pts',(92.,20.4819546873464,0.666911463789854));
#29726=CARTESIAN_POINT('Ctrl Pts',(92.,20.4650543294267,0.951766487557669));
#29727=CARTESIAN_POINT('Ctrl Pts',(92.,20.4420879241197,1.23610201945244));
#29728=CARTESIAN_POINT('Ctrl Pts',(92.,20.4077857600276,1.66077988879583));
#29729=CARTESIAN_POINT('Ctrl Pts',(92.,20.3599539272904,2.08429948485678));
#29730=CARTESIAN_POINT('Ctrl Pts',(92.,20.2988198171285,2.50606443235308));
#29731=CARTESIAN_POINT('Ctrl Pts',(92.,20.2376806168394,2.92786449669744));
#29732=CARTESIAN_POINT('Ctrl Pts',(92.,20.1632367394275,3.34791014691897));
#29733=CARTESIAN_POINT('Ctrl Pts',(92.,20.0756652657719,3.76559140238497));
#29734=CARTESIAN_POINT('Ctrl Pts',(92.,20.0107921805636,4.07501033237003));
#29735=CARTESIAN_POINT('Ctrl Pts',(92.,19.9387137896103,4.38313147665421));
#29736=CARTESIAN_POINT('Ctrl Pts',(92.,19.8594851502963,4.68969950654939));
#29737=CARTESIAN_POINT('Ctrl Pts',(92.,19.7901600908965,4.95794653270768));
#29738=CARTESIAN_POINT('Ctrl Pts',(92.,19.7153603920804,5.22500440903414));
#29739=CARTESIAN_POINT('Ctrl Pts',(92.,19.6351142811139,5.49069696494022));
#29740=CARTESIAN_POINT('Ctrl Pts',(92.,19.6247466371941,5.52502393454163));
#29741=CARTESIAN_POINT('Ctrl Pts',(92.,19.6142877564505,5.55932912547967));
#29742=CARTESIAN_POINT('Ctrl Pts',(92.,19.6037386647578,5.59360898626946));
#29743=CARTESIAN_POINT('Ctrl Pts',(92.,19.4792224942109,5.99823121506005));
#29744=CARTESIAN_POINT('Ctrl Pts',(92.,19.34242773395,6.39839984507992));
#29745=CARTESIAN_POINT('Ctrl Pts',(92.,19.1936344458134,6.79355365066581));
#29746=CARTESIAN_POINT('Ctrl Pts',(92.,19.0438980499274,7.19121208949771));
#29747=CARTESIAN_POINT('Ctrl Pts',(92.,18.8820103888085,7.58379245980847));
#29748=CARTESIAN_POINT('Ctrl Pts',(92.,18.7082055767162,7.9707113061041));
#29749=CARTESIAN_POINT('Ctrl Pts',(92.,18.5346901736901,8.35698587897231));
#29750=CARTESIAN_POINT('Ctrl Pts',(92.,18.349297063112,8.73761827716024));
#29751=CARTESIAN_POINT('Ctrl Pts',(92.,18.1522110520214,9.11200875632698));
#29752=CARTESIAN_POINT('Ctrl Pts',(92.,17.956955229384,9.4829225547889));
#29753=CARTESIAN_POINT('Ctrl Pts',(92.,17.7502224133289,9.84771028195912));
#29754=CARTESIAN_POINT('Ctrl Pts',(92.,17.5321485463934,10.2057627247099));
#29755=CARTESIAN_POINT('Ctrl Pts',(92.,17.4227884407154,10.3853195580332));
#29756=CARTESIAN_POINT('Ctrl Pts',(92.,17.3105755743928,10.5631821215417));
#29757=CARTESIAN_POINT('Ctrl Pts',(92.,17.1955231821568,10.7392705347842));
#29758=CARTESIAN_POINT('Ctrl Pts',(92.,16.9668897465601,11.0891954525194));
#29759=CARTESIAN_POINT('Ctrl Pts',(92.,16.7270449335161,11.4321165235876));
#29760=CARTESIAN_POINT('Ctrl Pts',(92.,16.4764020151916,11.767600152219));
#29761=CARTESIAN_POINT('Ctrl Pts',(92.,16.3667457384246,11.9143742397452));
#29762=CARTESIAN_POINT('Ctrl Pts',(92.,16.2550222124525,12.0597242811191));
#29763=CARTESIAN_POINT('Ctrl Pts',(92.,16.1412641903407,12.2036116409786));
#29764=CARTESIAN_POINT('Ctrl Pts',(92.,16.0850347937596,12.2747336530385));
#29765=CARTESIAN_POINT('Ctrl Pts',(92.,16.0283083085223,12.3454982768305));
#29766=CARTESIAN_POINT('Ctrl Pts',(92.,15.9710885983828,12.4159007092191));
#29767=CARTESIAN_POINT('Ctrl Pts',(92.,15.9463460917906,12.4463435870882));
#29768=CARTESIAN_POINT('Ctrl Pts',(92.,15.9215113610675,12.476718741088));
#29769=CARTESIAN_POINT('Ctrl Pts',(92.,15.8965847152718,12.5070257774445));
#29770=CARTESIAN_POINT('Ctrl Pts',(92.,15.8714065760418,12.5376385918313));
#29771=CARTESIAN_POINT('Ctrl Pts',(92.,15.8461408680008,12.5681743492675));
#29772=CARTESIAN_POINT('Ctrl Pts',(92.,15.8207895134622,12.5986310019053));
#29773=CARTESIAN_POINT('Ctrl Pts',(92.,15.5526633401512,12.9207528716145));
#29774=CARTESIAN_POINT('Ctrl Pts',(92.,15.2749071405144,13.2340931711695));
#29775=CARTESIAN_POINT('Ctrl Pts',(92.,14.9880458141498,13.5383111481772));
#29776=CARTESIAN_POINT('Ctrl Pts',(92.,14.699003791787,13.8448417650009));
#29777=CARTESIAN_POINT('Ctrl Pts',(92.,14.4007173132838,14.1421112257004));
#29778=CARTESIAN_POINT('Ctrl Pts',(92.,14.0936803430808,14.4297399483924));
#29779=CARTESIAN_POINT('Ctrl Pts',(92.,13.7770001609194,14.7264023217761));
#29780=CARTESIAN_POINT('Ctrl Pts',(92.,13.4510109375165,15.0128094692374));
#29781=CARTESIAN_POINT('Ctrl Pts',(92.,13.1162136914518,15.2885042773823));
#29782=CARTESIAN_POINT('Ctrl Pts',(92.,12.7926192649061,15.5549739224943));
#29783=CARTESIAN_POINT('Ctrl Pts',(92.,12.4607958105108,15.8114362654091));
#29784=CARTESIAN_POINT('Ctrl Pts',(92.,12.1211651035996,16.0574364911078));
#29785=CARTESIAN_POINT('Ctrl Pts',(92.,11.7842321306937,16.3014827027533));
#29786=CARTESIAN_POINT('Ctrl Pts',(92.,11.4396150210109,16.5352326307995));
#29787=CARTESIAN_POINT('Ctrl Pts',(92.,11.0877022244914,16.7581967512111));
#29788=CARTESIAN_POINT('Ctrl Pts',(92.,10.7411333572112,16.9777750769198));
#29789=CARTESIAN_POINT('Ctrl Pts',(92.,10.3874882912748,17.186892894028));
#29790=CARTESIAN_POINT('Ctrl Pts',(92.,10.0271214322955,17.3850347542793));
#29791=CARTESIAN_POINT('Ctrl Pts',(92.,9.97739598921864,17.4123754809515));
#29792=CARTESIAN_POINT('Ctrl Pts',(92.,9.92754254225955,17.4395071465117));
#29793=CARTESIAN_POINT('Ctrl Pts',(92.,9.87756200380534,17.4664283201656));
#29794=CARTESIAN_POINT('Ctrl Pts',(91.4938431528482,-20.9233577741311,-0.000216749186123405));
#29795=CARTESIAN_POINT('Ctrl Pts',(91.5109400481646,-20.9238979401944,-1.49907582982062));
#29796=CARTESIAN_POINT('Ctrl Pts',(91.5280369434811,-20.7650628346641,-2.99782158597188));
#29797=CARTESIAN_POINT('Ctrl Pts',(91.5451338387975,-20.4456617181001,-4.46152813557956));
#29798=CARTESIAN_POINT('Ctrl Pts',(91.5847521267121,-19.7055200045274,-7.85334556392255));
#29799=CARTESIAN_POINT('Ctrl Pts',(91.6243704146266,-18.1031733232879,-11.0570099843501));
#29800=CARTESIAN_POINT('Ctrl Pts',(91.6639887025412,-15.8331329754556,-13.6836424048636));
#29801=CARTESIAN_POINT('Ctrl Pts',(91.7036069904557,-13.5630926276235,-16.3102748253768));
#29802=CARTESIAN_POINT('Ctrl Pts',(91.7432252783703,-10.6253586131987,-18.3598752459761));
#29803=CARTESIAN_POINT('Ctrl Pts',(91.7828435662849,-7.37655328853197,-19.5835940627766));
#29804=CARTESIAN_POINT('Ctrl Pts',(91.8224618541995,-4.12774796386517,-20.8073128795771));
#29805=CARTESIAN_POINT('Ctrl Pts',(91.8620801421141,-0.567871328956467,
-21.2051500925789));
#29806=CARTESIAN_POINT('Ctrl Pts',(91.9016984300287,2.87094052292124,-20.7288964638728));
#29807=CARTESIAN_POINT('Ctrl Pts',(91.9344656200191,5.71508667923201,-20.3350002619699));
#29808=CARTESIAN_POINT('Ctrl Pts',(91.9672328100095,8.47641863398564,-19.343183398648));
#29809=CARTESIAN_POINT('Ctrl Pts',(92.,10.9270703901696,-17.8460909879584));
#29810=CARTESIAN_POINT('',(68.725,-11.6499306790267,-16.3385250883756));
#29811=CARTESIAN_POINT('Ctrl Pts',(68.725,-11.6499306790269,-16.3385250883755));
#29812=CARTESIAN_POINT('Ctrl Pts',(68.725,-11.9987892920946,-16.100985275945));
#29813=CARTESIAN_POINT('Ctrl Pts',(68.725,-12.3397428201089,-15.852668582927));
#29814=CARTESIAN_POINT('Ctrl Pts',(68.725,-12.6722355485707,-15.5938760861607));
#29815=CARTESIAN_POINT('Ctrl Pts',(68.725,-12.7943494799348,-15.4988298897105));
#29816=CARTESIAN_POINT('Ctrl Pts',(68.725,-12.9153219620097,-15.4023701941502));
#29817=CARTESIAN_POINT('Ctrl Pts',(68.725,-13.0351246648751,-15.3045103400552));
#29818=CARTESIAN_POINT('Ctrl Pts',(68.725,-13.3598924567193,-15.0392264360661));
#29819=CARTESIAN_POINT('Ctrl Pts',(68.725,-13.676066145712,-14.7636562391713));
#29820=CARTESIAN_POINT('Ctrl Pts',(68.725,-13.9833264286331,-14.4783477229447));
#29821=CARTESIAN_POINT('Ctrl Pts',(68.725,-14.2918745628573,-14.1918433640893));
#29822=CARTESIAN_POINT('Ctrl Pts',(68.725,-14.5914347756753,-13.8955184759107));
#29823=CARTESIAN_POINT('Ctrl Pts',(68.725,-14.8816491181147,-13.58988796133));
#29824=CARTESIAN_POINT('Ctrl Pts',(68.725,-15.1025513098886,-13.3572514555793));
#29825=CARTESIAN_POINT('Ctrl Pts',(68.725,-15.3180380420484,-13.1192226084338));
#29826=CARTESIAN_POINT('Ctrl Pts',(68.725,-15.5279361392978,-12.8760152733416));
#29827=CARTESIAN_POINT('Ctrl Pts',(68.725,-15.5573089156157,-12.8419812599506));
#29828=CARTESIAN_POINT('Ctrl Pts',(68.725,-15.5865695773343,-12.8078488654536));
#29829=CARTESIAN_POINT('Ctrl Pts',(68.725,-15.615712402069,-12.7736250045455));
#29830=CARTESIAN_POINT('Ctrl Pts',(68.725,-15.8891395467608,-12.4525259809051));
#29831=CARTESIAN_POINT('Ctrl Pts',(68.725,-16.1523380967823,-12.1232148948141));
#29832=CARTESIAN_POINT('Ctrl Pts',(68.725,-16.4049974667961,-11.78624941686));
#29833=CARTESIAN_POINT('Ctrl Pts',(68.725,-16.6638480447255,-11.4410268798691));
#29834=CARTESIAN_POINT('Ctrl Pts',(68.725,-16.9116371170591,-11.0877699117912));
#29835=CARTESIAN_POINT('Ctrl Pts',(68.725,-17.147991537967,-10.7270379841369));
#29836=CARTESIAN_POINT('Ctrl Pts',(68.725,-17.3793535036121,-10.3739257066834));
#29837=CARTESIAN_POINT('Ctrl Pts',(68.725,-17.5997589757048,-10.0136503549057));
#29838=CARTESIAN_POINT('Ctrl Pts',(68.725,-17.8088160791237,-9.64670563770897));
#29839=CARTESIAN_POINT('Ctrl Pts',(68.725,-18.0246399056295,-9.26788371926525));
#29840=CARTESIAN_POINT('Ctrl Pts',(68.725,-18.2283694893187,-8.88195335649133));
#29841=CARTESIAN_POINT('Ctrl Pts',(68.725,-18.4195215195112,-8.48943084625261));
#29842=CARTESIAN_POINT('Ctrl Pts',(68.725,-18.4372721406238,-8.45298070575238));
#29843=CARTESIAN_POINT('Ctrl Pts',(68.725,-18.4549124068542,-8.41647747693315));
#29844=CARTESIAN_POINT('Ctrl Pts',(68.725,-18.4724385493003,-8.37992885242366));
#29845=CARTESIAN_POINT('Ctrl Pts',(68.725,-18.6436470820391,-8.02289441685841));
#29846=CARTESIAN_POINT('Ctrl Pts',(68.725,-18.8040682762284,-7.66132317967038));
#29847=CARTESIAN_POINT('Ctrl Pts',(68.725,-18.9534486909712,-7.29565499339187));
#29848=CARTESIAN_POINT('Ctrl Pts',(68.725,-19.1136552191723,-6.90348557347062));
#29849=CARTESIAN_POINT('Ctrl Pts',(68.725,-19.2611637358523,-6.50660390994598));
#29850=CARTESIAN_POINT('Ctrl Pts',(68.725,-19.3960048313395,-6.10566837001001));
#29851=CARTESIAN_POINT('Ctrl Pts',(68.725,-19.5308721958782,-5.7046547218663));
#29852=CARTESIAN_POINT('Ctrl Pts',(68.725,-19.653067281878,-5.29958508272568));
#29853=CARTESIAN_POINT('Ctrl Pts',(68.725,-19.7625728366385,-4.89109319987111));
#29854=CARTESIAN_POINT('Ctrl Pts',(68.725,-19.8725372525205,-4.48088961349667));
#29855=CARTESIAN_POINT('Ctrl Pts',(68.725,-19.9697056892801,-4.06723451410488));
#29856=CARTESIAN_POINT('Ctrl Pts',(68.725,-20.0540108703053,-3.65075241347895));
#29857=CARTESIAN_POINT('Ctrl Pts',(68.725,-20.1382310371142,-3.23469029770981));
#29858=CARTESIAN_POINT('Ctrl Pts',(68.725,-20.2096139643298,-2.81580633501393));
#29859=CARTESIAN_POINT('Ctrl Pts',(68.725,-20.2680414869829,-2.39471406072667));
#29860=CARTESIAN_POINT('Ctrl Pts',(68.725,-20.326156800138,-1.97587190764284));
#29861=CARTESIAN_POINT('Ctrl Pts',(68.725,-20.3714548499849,-1.5548444432437));
#29862=CARTESIAN_POINT('Ctrl Pts',(68.725,-20.4037677778091,-1.13223450157562));
#29863=CARTESIAN_POINT('Ctrl Pts',(68.725,-20.4091213406707,-1.06221704908848));
#29864=CARTESIAN_POINT('Ctrl Pts',(68.725,-20.4141183529857,-0.992156166950641));
#29865=CARTESIAN_POINT('Ctrl Pts',(68.725,-20.4187579119077,-0.922054610248633));
#29866=CARTESIAN_POINT('Ctrl Pts',(68.725,-20.422098764979,-0.871575889111893));
#29867=CARTESIAN_POINT('Ctrl Pts',(68.725,-20.4252544645954,-0.821072156902455));
#29868=CARTESIAN_POINT('Ctrl Pts',(68.725,-20.4282231742031,-0.770571679141828));
#29869=CARTESIAN_POINT('Ctrl Pts',(68.725,-20.4533182195221,-0.343681903620332));
#29870=CARTESIAN_POINT('Ctrl Pts',(68.725,-20.4650818340108,0.0833365859073504));
#29871=CARTESIAN_POINT('Ctrl Pts',(68.725,-20.463517702269,0.509847184542638));
#29872=CARTESIAN_POINT('Ctrl Pts',(68.725,-20.461948035478,0.937867091567226));
#29873=CARTESIAN_POINT('Ctrl Pts',(68.725,-20.4469562296846,1.36537605047279));
#29874=CARTESIAN_POINT('Ctrl Pts',(68.725,-20.4184952559188,1.79174359745879));
#29875=CARTESIAN_POINT('Ctrl Pts',(68.725,-20.3989647374653,2.0843259705317));
#29876=CARTESIAN_POINT('Ctrl Pts',(68.725,-20.373090542812,2.37637112215609));
#29877=CARTESIAN_POINT('Ctrl Pts',(68.725,-20.3408433469955,2.66767680784106));
#29878=CARTESIAN_POINT('Ctrl Pts',(68.725,-20.2938522813738,3.09217153506962));
#29879=CARTESIAN_POINT('Ctrl Pts',(68.725,-20.2333307283686,3.51509643752233));
#29880=CARTESIAN_POINT('Ctrl Pts',(68.725,-20.1595547533075,3.935873610376));
#29881=CARTESIAN_POINT('Ctrl Pts',(68.725,-20.0857891749123,4.35659148642359));
#29882=CARTESIAN_POINT('Ctrl Pts',(68.725,-19.9987727312683,4.77516275868168));
#29883=CARTESIAN_POINT('Ctrl Pts',(68.725,-19.8987294279677,5.19100075672885));
#29884=CARTESIAN_POINT('Ctrl Pts',(68.725,-19.8236846127296,5.50293053816237));
#29885=CARTESIAN_POINT('Ctrl Pts',(68.725,-19.7413086989252,5.81332221201406));
#29886=CARTESIAN_POINT('Ctrl Pts',(68.725,-19.651677945131,6.12192214555817));
#29887=CARTESIAN_POINT('Ctrl Pts',(68.725,-19.5732510355612,6.39194708740926));
#29888=CARTESIAN_POINT('Ctrl Pts',(68.725,-19.4892693892593,6.66060020105372));
#29889=CARTESIAN_POINT('Ctrl Pts',(68.725,-19.3997746480287,6.92770707799559));
#29890=CARTESIAN_POINT('Ctrl Pts',(68.725,-19.3874363192146,6.96453217443008));
#29891=CARTESIAN_POINT('Ctrl Pts',(68.725,-19.3749922652267,7.00133057306016));
#29892=CARTESIAN_POINT('Ctrl Pts',(68.725,-19.3624457063944,7.03809267495641));
#29893=CARTESIAN_POINT('Ctrl Pts',(68.725,-19.2244394670901,7.44245848548721));
#29894=CARTESIAN_POINT('Ctrl Pts',(68.725,-19.0741889509375,7.84199020533157));
#29895=CARTESIAN_POINT('Ctrl Pts',(68.725,-18.9120227648927,8.23613571192123));
#29896=CARTESIAN_POINT('Ctrl Pts',(68.725,-18.7482047332631,8.63429603522855));
#29897=CARTESIAN_POINT('Ctrl Pts',(68.725,-18.5722269355258,9.02696038238803));
#29898=CARTESIAN_POINT('Ctrl Pts',(68.725,-18.3843755501797,9.41355256367695));
#29899=CARTESIAN_POINT('Ctrl Pts',(68.725,-18.1963904566248,9.80041991221034));
#29900=CARTESIAN_POINT('Ctrl Pts',(68.725,-17.996514678722,10.1812069718227));
#29901=CARTESIAN_POINT('Ctrl Pts',(68.725,-17.7849850009624,10.5553214340206));
#29902=CARTESIAN_POINT('Ctrl Pts',(68.725,-17.5747675470806,10.9271150779981));
#29903=CARTESIAN_POINT('Ctrl Pts',(68.725,-17.3530401041389,11.2923191462909));
#29904=CARTESIAN_POINT('Ctrl Pts',(68.725,-17.119988918834,11.6503300347784));
#29905=CARTESIAN_POINT('Ctrl Pts',(68.725,-17.0041505504421,11.8282797720202));
#29906=CARTESIAN_POINT('Ctrl Pts',(68.725,-16.8855138433729,12.0044519712643));
#29907=CARTESIAN_POINT('Ctrl Pts',(68.725,-16.7640976485875,12.1787698690955));
#29908=CARTESIAN_POINT('Ctrl Pts',(68.725,-16.5175195192571,12.5327834439073));
#29909=CARTESIAN_POINT('Ctrl Pts',(68.725,-16.2594801824049,12.8791515357829));
#29910=CARTESIAN_POINT('Ctrl Pts',(68.725,-15.9904435978116,13.2174610733958));
#29911=CARTESIAN_POINT('Ctrl Pts',(68.725,-15.8727400920521,13.3654714961014));
#29912=CARTESIAN_POINT('Ctrl Pts',(68.725,-15.7529311424556,13.5119389942562));
#29913=CARTESIAN_POINT('Ctrl Pts',(68.725,-15.6310533922898,13.6568266706687));
#29914=CARTESIAN_POINT('Ctrl Pts',(68.725,-15.5693617221597,13.7301654279644));
#29915=CARTESIAN_POINT('Ctrl Pts',(68.725,-15.5071399745656,13.8030993881211));
#29916=CARTESIAN_POINT('Ctrl Pts',(68.725,-15.4443927821345,13.8756236175601));
#29917=CARTESIAN_POINT('Ctrl Pts',(68.725,-15.4207447743093,13.902956371088));
#29918=CARTESIAN_POINT('Ctrl Pts',(68.725,-15.3970214238862,13.9302317377608));
#29919=CARTESIAN_POINT('Ctrl Pts',(68.725,-15.3732251808066,13.9574469290418));
#29920=CARTESIAN_POINT('Ctrl Pts',(68.725,-15.0919796997952,14.2791006260988));
#29921=CARTESIAN_POINT('Ctrl Pts',(68.725,-14.8011916071194,14.5916249436891));
#29922=CARTESIAN_POINT('Ctrl Pts',(68.725,-14.5014254406708,14.8947134294339));
#29923=CARTESIAN_POINT('Ctrl Pts',(68.725,-14.198654557309,15.2008399334786));
#29924=CARTESIAN_POINT('Ctrl Pts',(68.725,-13.886724384795,15.4973408812269));
#29925=CARTESIAN_POINT('Ctrl Pts',(68.725,-13.5661704902236,15.7838736081083));
#29926=CARTESIAN_POINT('Ctrl Pts',(68.725,-13.2438021970466,16.0720281670401));
#29927=CARTESIAN_POINT('Ctrl Pts',(68.725,-12.9127119086089,16.350101727454));
#29928=CARTESIAN_POINT('Ctrl Pts',(68.725,-12.5734032896817,16.6177129020166));
#29929=CARTESIAN_POINT('Ctrl Pts',(68.725,-12.2344059655302,16.8850785597962));
#29930=CARTESIAN_POINT('Ctrl Pts',(68.725,-11.8872049704363,17.142001376928));
#29931=CARTESIAN_POINT('Ctrl Pts',(68.725,-11.5322676984425,17.3880627724302));
#29932=CARTESIAN_POINT('Ctrl Pts',(68.725,-11.179301167814,17.6327579451973));
#29933=CARTESIAN_POINT('Ctrl Pts',(68.725,-10.818683608423,17.8667122980006));
#29934=CARTESIAN_POINT('Ctrl Pts',(68.725,-10.4508464323994,18.0894713180186));
#29935=CARTESIAN_POINT('Ctrl Pts',(68.725,-10.0879532382318,18.3092363052824));
#29936=CARTESIAN_POINT('Ctrl Pts',(68.725,-9.71803277350823,18.5181051321412));
#29937=CARTESIAN_POINT('Ctrl Pts',(68.725,-9.3414780335832,18.7155953847213));
#29938=CARTESIAN_POINT('Ctrl Pts',(68.725,-9.22860300304108,18.7747945287718));
#29939=CARTESIAN_POINT('Ctrl Pts',(68.725,-9.11513173031872,18.8329709265167));
#29940=CARTESIAN_POINT('Ctrl Pts',(68.725,-9.0010745076591,18.8901107118929));
#29941=CARTESIAN_POINT('Ctrl Pts',(68.725,-11.6499306790267,-16.3385250883756));
#29942=CARTESIAN_POINT('Ctrl Pts',(68.7577671899904,-9.40607008510334,-17.9350305838001));
#29943=CARTESIAN_POINT('Ctrl Pts',(68.8301526678954,-3.71778776782437,-20.4401340743294));
#29944=CARTESIAN_POINT('Ctrl Pts',(68.9421564337151,5.98487983261901,-20.039336396671));
#29945=CARTESIAN_POINT('Ctrl Pts',(69.0610112974588,14.8280289192567,-14.7486055907437));
#29946=CARTESIAN_POINT('Ctrl Pts',(69.1798661612025,20.0711408256307,-5.87721609629587));
#29947=CARTESIAN_POINT('Ctrl Pts',(69.2987210249463,20.4412844203846,4.42111651613181));
#29948=CARTESIAN_POINT('Ctrl Pts',(69.4175758886899,15.8485849447886,13.6460461909995));
#29949=CARTESIAN_POINT('Ctrl Pts',(69.5364307524338,7.40808631971404,19.5579297437878));
#29950=CARTESIAN_POINT('Ctrl Pts',(69.6552856161775,-2.83098632764961,20.7214331897253));
#29951=CARTESIAN_POINT('Ctrl Pts',(69.7741404799212,-12.3827371735606,16.8540836193131));
#29952=CARTESIAN_POINT('Ctrl Pts',(69.8883354092291,-18.6715184686174,9.20687033992677));
#29953=CARTESIAN_POINT('Ctrl Pts',(69.9629120506222,-20.0646021687516,2.93742032732148));
#29954=CARTESIAN_POINT('Ctrl Pts',(69.9978704041008,-20.0670795681067,-0.000365800382557055));
#29955=CARTESIAN_POINT('Origin',(68.725,-1.75604157117454E-15,0.));
#29956=CARTESIAN_POINT('',(68.725,-20.925,-2.56257342721584E-15));
#29957=CARTESIAN_POINT('Origin',(68.725,0.,0.));
#29958=CARTESIAN_POINT('Origin',(68.725,0.,0.));
#29959=CARTESIAN_POINT('',(68.725,11.6491905967232,-16.3382590211967));
#29960=CARTESIAN_POINT('Ctrl Pts',(68.725,9.00178625489518,18.890518144815));
#29961=CARTESIAN_POINT('Ctrl Pts',(68.725,9.38925803975212,18.6968856239625));
#29962=CARTESIAN_POINT('Ctrl Pts',(68.725,9.77026673223583,18.4913974126918));
#29963=CARTESIAN_POINT('Ctrl Pts',(68.725,10.1442182949888,18.2742433770339));
#29964=CARTESIAN_POINT('Ctrl Pts',(68.725,10.2888543730052,18.1902530660648));
#29965=CARTESIAN_POINT('Ctrl Pts',(68.725,10.4324345077463,18.1045170779589));
#29966=CARTESIAN_POINT('Ctrl Pts',(68.725,10.5749234040853,18.0170445175294));
#29967=CARTESIAN_POINT('Ctrl Pts',(68.725,10.9434705568083,17.7907969718192));
#29968=CARTESIAN_POINT('Ctrl Pts',(68.725,11.3047195365857,17.5529348738655));
#29969=CARTESIAN_POINT('Ctrl Pts',(68.725,11.6582499229056,17.3039440167568));
#29970=CARTESIAN_POINT('Ctrl Pts',(68.725,12.0123054338337,17.0545833152689));
#29971=CARTESIAN_POINT('Ctrl Pts',(68.725,12.3586197932977,16.794060375687));
#29972=CARTESIAN_POINT('Ctrl Pts',(68.725,12.6967370719532,16.5228229871426));
#29973=CARTESIAN_POINT('Ctrl Pts',(68.725,12.9487607468455,16.3206498130859));
#29974=CARTESIAN_POINT('Ctrl Pts',(68.725,13.1962296143473,16.1125230269113));
#29975=CARTESIAN_POINT('Ctrl Pts',(68.725,13.4389407817561,15.8986155470502));
#29976=CARTESIAN_POINT('Ctrl Pts',(68.725,13.476935663215,15.8651296987176));
#29977=CARTESIAN_POINT('Ctrl Pts',(68.725,13.5148154030423,15.8315008121615));
#29978=CARTESIAN_POINT('Ctrl Pts',(68.725,13.5525660521234,15.7977413953055));
#29979=CARTESIAN_POINT('Ctrl Pts',(68.725,13.8742113629858,15.5101024170764));
#29980=CARTESIAN_POINT('Ctrl Pts',(68.725,14.1866885968815,15.2128157948926));
#29981=CARTESIAN_POINT('Ctrl Pts',(68.725,14.4895927569317,14.906371940508));
#29982=CARTESIAN_POINT('Ctrl Pts',(68.725,14.8024039249045,14.5899053063349));
#29983=CARTESIAN_POINT('Ctrl Pts',(68.725,15.1050061927679,14.2636724048909));
#29984=CARTESIAN_POINT('Ctrl Pts',(68.725,15.396913789591,13.9281711290047));
#29985=CARTESIAN_POINT('Ctrl Pts',(68.725,15.6785445458156,13.6044814440822));
#29986=CARTESIAN_POINT('Ctrl Pts',(68.725,15.9502205399353,13.2721638912857));
#29987=CARTESIAN_POINT('Ctrl Pts',(68.725,16.2114642691751,12.9316338894825));
#29988=CARTESIAN_POINT('Ctrl Pts',(68.725,16.4705940747135,12.5938593775202));
#29989=CARTESIAN_POINT('Ctrl Pts',(68.725,16.7194600643542,12.248004375501));
#29990=CARTESIAN_POINT('Ctrl Pts',(68.725,16.9575514286903,11.8944497505135));
#29991=CARTESIAN_POINT('Ctrl Pts',(68.725,16.9829467777613,11.8567388358725));
#29992=CARTESIAN_POINT('Ctrl Pts',(68.725,17.008220425394,11.8189389107047));
#29993=CARTESIAN_POINT('Ctrl Pts',(68.725,17.0333688243885,11.7810547868178));
#29994=CARTESIAN_POINT('Ctrl Pts',(68.725,17.2738646611779,11.4187663533783));
#29995=CARTESIAN_POINT('Ctrl Pts',(68.725,17.5024722926295,11.0494413563035));
#29996=CARTESIAN_POINT('Ctrl Pts',(68.725,17.7187805264893,10.6735630585382));
#29997=CARTESIAN_POINT('Ctrl Pts',(68.725,17.9318816017938,10.3032578324811));
#29998=CARTESIAN_POINT('Ctrl Pts',(68.725,18.1330457301988,9.92659180879433));
#29999=CARTESIAN_POINT('Ctrl Pts',(68.725,18.322187624511,9.5442034481681));
#30000=CARTESIAN_POINT('Ctrl Pts',(68.725,18.5121973296755,9.16006063345676));
#30001=CARTESIAN_POINT('Ctrl Pts',(68.725,18.69007439373,8.77014233425846));
#30002=CARTESIAN_POINT('Ctrl Pts',(68.725,18.8556856344539,8.37506995850641));
#30003=CARTESIAN_POINT('Ctrl Pts',(68.725,19.0215588002192,7.97937274987526));
#30004=CARTESIAN_POINT('Ctrl Pts',(68.725,19.1751274650245,7.57850461655889));
#30005=CARTESIAN_POINT('Ctrl Pts',(68.725,19.3162087073801,7.17307192876857));
#30006=CARTESIAN_POINT('Ctrl Pts',(68.725,19.4567700648238,6.76913326196687));
#30007=CARTESIAN_POINT('Ctrl Pts',(68.725,19.584935976176,6.36066308509569));
#30008=CARTESIAN_POINT('Ctrl Pts',(68.725,19.7004749109341,5.94825124717928));
#30009=CARTESIAN_POINT('Ctrl Pts',(68.725,19.8153479310481,5.53821636628431));
#30010=CARTESIAN_POINT('Ctrl Pts',(68.725,19.9177392069654,5.12428461199538));
#30011=CARTESIAN_POINT('Ctrl Pts',(68.725,20.0073694943154,4.70703378549649));
#30012=CARTESIAN_POINT('Ctrl Pts',(68.725,20.0203574504677,4.64657168502481));
#30013=CARTESIAN_POINT('Ctrl Pts',(68.725,20.0330773644314,4.58603989614209));
#30014=CARTESIAN_POINT('Ctrl Pts',(68.725,20.0455282938352,4.52544018357549));
#30015=CARTESIAN_POINT('Ctrl Pts',(68.725,20.0531606330853,4.48829295144747));
#30016=CARTESIAN_POINT('Ctrl Pts',(68.725,20.0606918979433,4.45112019629494));
#30017=CARTESIAN_POINT('Ctrl Pts',(68.725,20.0681218669106,4.41392232515951));
#30018=CARTESIAN_POINT('Ctrl Pts',(68.725,20.0757867204331,4.37554851298652));
#30019=CARTESIAN_POINT('Ctrl Pts',(68.725,20.0833418512032,4.33715757420951));
#30020=CARTESIAN_POINT('Ctrl Pts',(68.725,20.0907868831788,4.29875154530138));
#30021=CARTESIAN_POINT('Ctrl Pts',(68.725,20.1721779867712,3.87888644764823));
#30022=CARTESIAN_POINT('Ctrl Pts',(68.725,20.2404270161492,3.45715794634081));
#30023=CARTESIAN_POINT('Ctrl Pts',(68.725,20.2954236349033,3.03417607531588));
#30024=CARTESIAN_POINT('Ctrl Pts',(68.725,20.3504034542094,2.6113234097238));
#30025=CARTESIAN_POINT('Ctrl Pts',(68.725,20.3921390760943,2.18721760469451));
#30026=CARTESIAN_POINT('Ctrl Pts',(68.725,20.420470100454,1.76245484355877));
#30027=CARTESIAN_POINT('Ctrl Pts',(68.725,20.4394635270914,1.47768927209487));
#30028=CARTESIAN_POINT('Ctrl Pts',(68.725,20.4524312120413,1.19262816696663));
#30029=CARTESIAN_POINT('Ctrl Pts',(68.725,20.4593117811368,0.907449630746225));
#30030=CARTESIAN_POINT('Ctrl Pts',(68.725,20.4695884628776,0.481512616615602));
#30031=CARTESIAN_POINT('Ctrl Pts',(68.725,20.4662885233733,0.055313289463583));
#30032=CARTESIAN_POINT('Ctrl Pts',(68.725,20.4495757689587,-0.370531471920013));
#30033=CARTESIAN_POINT('Ctrl Pts',(68.725,20.4328616239798,-0.796411665197902));
#30034=CARTESIAN_POINT('Ctrl Pts',(68.725,20.4027323035974,-1.22193777674415));
#30035=CARTESIAN_POINT('Ctrl Pts',(68.725,20.359300157245,-1.64648465592586));
#30036=CARTESIAN_POINT('Ctrl Pts',(68.725,20.3271255537314,-1.96098966334021));
#30037=CARTESIAN_POINT('Ctrl Pts',(68.725,20.287649461122,-2.27495715534068));
#30038=CARTESIAN_POINT('Ctrl Pts',(68.725,20.2408999456565,-2.58812744623019));
#30039=CARTESIAN_POINT('Ctrl Pts',(68.725,20.1999941196242,-2.86215145075851));
#30040=CARTESIAN_POINT('Ctrl Pts',(68.725,20.1535193450914,-3.1355650759092));
#30041=CARTESIAN_POINT('Ctrl Pts',(68.725,20.1014852795674,-3.4081901651746));
#30042=CARTESIAN_POINT('Ctrl Pts',(68.725,20.094762577507,-3.44341280693583));
#30043=CARTESIAN_POINT('Ctrl Pts',(68.725,20.0879468619263,-3.4786233261834));
#30044=CARTESIAN_POINT('Ctrl Pts',(68.725,20.0810387818474,-3.51381808365658));
#30045=CARTESIAN_POINT('Ctrl Pts',(68.725,19.9994992812284,-3.9292392883932));
#30046=CARTESIAN_POINT('Ctrl Pts',(68.725,19.9052829250088,-4.34151475336195));
#30047=CARTESIAN_POINT('Ctrl Pts',(68.725,19.7986095757904,-4.75005705124187));
#30048=CARTESIAN_POINT('Ctrl Pts',(68.725,19.6912600984964,-5.16118881424805));
#30049=CARTESIAN_POINT('Ctrl Pts',(68.725,19.5712951185248,-5.56854047845237));
#30050=CARTESIAN_POINT('Ctrl Pts',(68.725,19.4388864788952,-5.97150731141695));
#30051=CARTESIAN_POINT('Ctrl Pts',(68.725,19.3066983254461,-6.3738031260997));
#30052=CARTESIAN_POINT('Ctrl Pts',(68.725,19.162107763649,-6.77172923042562));
#30053=CARTESIAN_POINT('Ctrl Pts',(68.725,19.005235896752,-7.16466984645415));
#30054=CARTESIAN_POINT('Ctrl Pts',(68.725,18.8498207943706,-7.55396148476931));
#30055=CARTESIAN_POINT('Ctrl Pts',(68.725,18.6823512228577,-7.9383602804339));
#30056=CARTESIAN_POINT('Ctrl Pts',(68.725,18.5028986988963,-8.31724614652518));
#30057=CARTESIAN_POINT('Ctrl Pts',(68.725,18.4129064453031,-8.50725067915277));
#30058=CARTESIAN_POINT('Ctrl Pts',(68.725,18.3198999557319,-8.69586841528021));
#30059=CARTESIAN_POINT('Ctrl Pts',(68.725,18.22388404251,-8.88301852833684));
#30060=CARTESIAN_POINT('Ctrl Pts',(68.725,18.0330801990091,-9.25492522259813));
#30061=CARTESIAN_POINT('Ctrl Pts',(68.725,17.8303942892476,-9.62103833894468));
#30062=CARTESIAN_POINT('Ctrl Pts',(68.725,17.6161919994574,-9.98088345991726));
#30063=CARTESIAN_POINT('Ctrl Pts',(68.725,17.5224784976742,-10.1383157003428));
#30064=CARTESIAN_POINT('Ctrl Pts',(68.725,17.4265602172733,-10.2945477810432));
#30065=CARTESIAN_POINT('Ctrl Pts',(68.725,17.3284656934938,-10.4495378548228));
#30066=CARTESIAN_POINT('Ctrl Pts',(68.725,17.2799785994724,-10.5261478223335));
#30067=CARTESIAN_POINT('Ctrl Pts',(68.725,17.2309597825059,-10.6024543190805));
#30068=CARTESIAN_POINT('Ctrl Pts',(68.725,17.1814125831296,-10.6784521643853));
#30069=CARTESIAN_POINT('Ctrl Pts',(68.725,17.1599877734037,-10.7113145541013));
#30070=CARTESIAN_POINT('Ctrl Pts',(68.725,17.1384641657444,-10.7441192310031));
#30071=CARTESIAN_POINT('Ctrl Pts',(68.725,17.1168420263571,-10.7768657711699));
#30072=CARTESIAN_POINT('Ctrl Pts',(68.725,17.0950017185671,-10.8099427254663));
#30073=CARTESIAN_POINT('Ctrl Pts',(68.725,17.0730662669445,-10.8429521983094));
#30074=CARTESIAN_POINT('Ctrl Pts',(68.725,17.0510373692289,-10.8758919521138));
#30075=CARTESIAN_POINT('Ctrl Pts',(68.725,16.818050944262,-11.2242759510445));
#30076=CARTESIAN_POINT('Ctrl Pts',(68.725,16.5745693237755,-11.564933096434));
#30077=CARTESIAN_POINT('Ctrl Pts',(68.725,16.3210789145324,-11.8974696375785));
#30078=CARTESIAN_POINT('Ctrl Pts',(68.725,16.0656614747229,-12.232534116885));
#30079=CARTESIAN_POINT('Ctrl Pts',(68.725,15.8000821665744,-12.5593544816777));
#30080=CARTESIAN_POINT('Ctrl Pts',(68.725,15.5247925724923,-12.8775015980273));
#30081=CARTESIAN_POINT('Ctrl Pts',(68.725,15.2408568295324,-13.2056409094765));
#30082=CARTESIAN_POINT('Ctrl Pts',(68.725,14.9465910767754,-13.5245542327704));
#30083=CARTESIAN_POINT('Ctrl Pts',(68.725,14.6424458081594,-13.8337345898222));
#30084=CARTESIAN_POINT('Ctrl Pts',(68.725,14.3484776729286,-14.1325693322663));
#30085=CARTESIAN_POINT('Ctrl Pts',(68.725,14.0452795397488,-14.4223117602991));
#30086=CARTESIAN_POINT('Ctrl Pts',(68.725,13.7332233336194,-14.702465464485));
#30087=CARTESIAN_POINT('Ctrl Pts',(68.725,13.4236458124489,-14.9803938875865));
#30088=CARTESIAN_POINT('Ctrl Pts',(68.725,13.1053499927846,-15.2488856416173));
#30089=CARTESIAN_POINT('Ctrl Pts',(68.725,12.7786710287523,-15.5074132815735));
#30090=CARTESIAN_POINT('Ctrl Pts',(68.725,12.4569527845981,-15.7620151003297));
#30091=CARTESIAN_POINT('Ctrl Pts',(68.725,12.1271036836736,-16.0069533777913));
#30092=CARTESIAN_POINT('Ctrl Pts',(68.725,11.7894223124711,-16.2416784451644));
#30093=CARTESIAN_POINT('Ctrl Pts',(68.725,11.7428273090342,-16.274067010995));
#30094=CARTESIAN_POINT('Ctrl Pts',(68.725,11.6960831511765,-16.3062610424414));
#30095=CARTESIAN_POINT('Ctrl Pts',(68.725,11.6491905967231,-16.3382590211968));
#30096=CARTESIAN_POINT('Origin',(68.725,0.,0.));
#30097=CARTESIAN_POINT('Origin',(65.9521295958992,0.,0.));
#30098=CARTESIAN_POINT('Ctrl Pts',(68.725,11.6491905967231,-16.3382590211968));
#30099=CARTESIAN_POINT('Ctrl Pts',(68.7646182879146,14.3605687349063,-14.4050444314105));
#30100=CARTESIAN_POINT('Ctrl Pts',(68.8438548637438,18.799624465765,-9.16469984651376));
#30101=CARTESIAN_POINT('Ctrl Pts',(68.9627097274874,20.8933712948219,0.927153582356417));
#30102=CARTESIAN_POINT('Ctrl Pts',(69.0815645912312,17.9146243999094,10.7913118927399));
#30103=CARTESIAN_POINT('Ctrl Pts',(69.200419454975,10.5864329691218,18.0367711701248));
#30104=CARTESIAN_POINT('Ctrl Pts',(69.3192743187187,0.688032188973571,20.9025284426369));
#30105=CARTESIAN_POINT('Ctrl Pts',(69.4381291824624,-9.37742221120445,18.6937889137184));
#30106=CARTESIAN_POINT('Ctrl Pts',(69.5569840462062,-17.1661730459504,11.9463094506391));
#30107=CARTESIAN_POINT('Ctrl Pts',(69.6449841840185,-19.847207074249,4.80309241700195));
#30108=CARTESIAN_POINT('Ctrl Pts',(69.6933660339161,-20.0668056364202,0.737086159903154));
#30109=CARTESIAN_POINT('Ctrl Pts',(69.7021295958992,-20.0660502412321,0.000515820514980642));
#30110=CARTESIAN_POINT('Ctrl Pts',(68.2290272512527,12.1479079354045,-17.0377216139053));
#30111=CARTESIAN_POINT('Ctrl Pts',(68.2686455391672,14.9753637768416,-15.0217435370499));
#30112=CARTESIAN_POINT('Ctrl Pts',(68.3478821149964,19.6044613858867,-9.55705283269926));
#30113=CARTESIAN_POINT('Ctrl Pts',(68.4667369787401,21.787844300626,0.966846259998003));
#30114=CARTESIAN_POINT('Ctrl Pts',(68.5855918424839,18.6815732904799,11.2533023034334));
#30115=CARTESIAN_POINT('Ctrl Pts',(68.7044467062276,11.0396522406801,18.8089493263395));
#30116=CARTESIAN_POINT('Ctrl Pts',(68.8233015699713,0.717487761819058,21.7973934781148));
#30117=CARTESIAN_POINT('Ctrl Pts',(68.9421564337151,-9.7788821246665,19.4940948731338));
#30118=CARTESIAN_POINT('Ctrl Pts',(69.0610112974588,-17.9010797388866,12.457746842518));
#30119=CARTESIAN_POINT('Ctrl Pts',(69.1798661612025,-21.6771639701384,2.39693115856188));
#30120=CARTESIAN_POINT('Ctrl Pts',(69.2987210249463,-20.1903538023596,-8.24586855545789));
#30121=CARTESIAN_POINT('Ctrl Pts',(69.41757588869,-13.8016266268924,-16.8866712137983));
#30122=CARTESIAN_POINT('Ctrl Pts',(69.5364307524337,-4.062069390721,-21.4276527915994));
#30123=CARTESIAN_POINT('Ctrl Pts',(69.6552856161776,6.66369771808618,-20.7663129975645));
#30124=CARTESIAN_POINT('Ctrl Pts',(69.7741404799212,15.7716181964099,-15.0632241959129));
#30125=CARTESIAN_POINT('Ctrl Pts',(69.892995343665,21.0504242506639,-5.70300701887552));
#30126=CARTESIAN_POINT('Ctrl Pts',(70.0118502074087,21.2185003328937,5.04181468411517));
#30127=CARTESIAN_POINT('Ctrl Pts',(70.1307050711524,16.2350400350607,14.5625591469258));
#30128=CARTESIAN_POINT('Ctrl Pts',(70.2495599348962,7.30995343255451,20.5477305886088));
#30129=CARTESIAN_POINT('Ctrl Pts',(70.3684147986399,-3.38988116968799,21.5442186838522));
#30130=CARTESIAN_POINT('Ctrl Pts',(70.4872696623837,-13.2667030288609,17.3100907863903));
#30131=CARTESIAN_POINT('Ctrl Pts',(70.6061245261274,-19.9225666650911,8.87333026802901));
#30132=CARTESIAN_POINT('Ctrl Pts',(70.7249793898711,-21.741527356917,-1.71774290924665));
#30133=CARTESIAN_POINT('Ctrl Pts',(70.8438342536149,-18.2819684963326,-11.8917736436063));
#30134=CARTESIAN_POINT('Ctrl Pts',(70.9626891173586,-10.3838195318354,-19.1786585677004));
#30135=CARTESIAN_POINT('Ctrl Pts',(71.0815439811023,0.0353664108211744,
-21.8092503703829));
#30136=CARTESIAN_POINT('Ctrl Pts',(71.2003988448461,10.4459659148443,-19.144880480705));
#30137=CARTESIAN_POINT('Ctrl Pts',(71.3192537085898,18.3204402229448,-11.8324182881816));
#30138=CARTESIAN_POINT('Ctrl Pts',(71.4381085723336,21.7469840640831,-1.64722087984511));
#30139=CARTESIAN_POINT('Ctrl Pts',(71.5569634360772,19.8936835452454,8.93789726458204));
#30140=CARTESIAN_POINT('Ctrl Pts',(71.675818299821,13.2104924744173,17.3530268568187));
#30141=CARTESIAN_POINT('Ctrl Pts',(71.7946731635647,3.31999026665197,21.555099562281));
#30142=CARTESIAN_POINT('Ctrl Pts',(71.9135280273085,-7.37655621064897,20.5239146115309));
#30143=CARTESIAN_POINT('Ctrl Pts',(72.0323828910521,-16.2821845270664,14.5098283772393));
#30144=CARTESIAN_POINT('Ctrl Pts',(72.151237754796,-21.2347405512553,4.97297156951684));
#30145=CARTESIAN_POINT('Ctrl Pts',(72.2700926185397,-21.031817323487,-5.77124878876516));
#30146=CARTESIAN_POINT('Ctrl Pts',(72.3889474822835,-15.7226815860593,-15.1142957577833));
#30147=CARTESIAN_POINT('Ctrl Pts',(72.5078023460271,-6.59631255084762,-20.7878164616172));
#30148=CARTESIAN_POINT('Ctrl Pts',(72.626657209771,4.13154308662491,-21.4143644368381));
#30149=CARTESIAN_POINT('Ctrl Pts',(72.7455120735146,13.8563214974062,-16.8418231516327));
#30150=CARTESIAN_POINT('Ctrl Pts',(72.8643669372584,20.2169910877431,-8.18033763780386));
#30151=CARTESIAN_POINT('Ctrl Pts',(72.983221801002,21.6692758622504,2.46721221544587));
#30152=CARTESIAN_POINT('Ctrl Pts',(73.102076664746,17.8605826726939,12.515759629452));
#30153=CARTESIAN_POINT('Ctrl Pts',(73.2209315284895,9.71560559143255,19.5256667108214));
#30154=CARTESIAN_POINT('Ctrl Pts',(73.3397863922334,-0.788176059440954,
21.7950322553025));
#30155=CARTESIAN_POINT('Ctrl Pts',(73.458641255977,-11.1006002830113,18.7728880534446));
#30156=CARTESIAN_POINT('Ctrl Pts',(73.5774961197208,-18.717963820288,11.1929657791286));
#30157=CARTESIAN_POINT('Ctrl Pts',(73.6963509834645,-21.790884072211,0.895557849507379));
#30158=CARTESIAN_POINT('Ctrl Pts',(73.8152058472083,-19.5733016949674,-9.61927820931176));
#30159=CARTESIAN_POINT('Ctrl Pts',(73.934060710952,-12.6036127150021,-17.79869655454));
#30160=CARTESIAN_POINT('Ctrl Pts',(74.0529155746958,-2.57395397957607,-21.656856037324));
#30161=CARTESIAN_POINT('Ctrl Pts',(74.1717704384395,8.08062250820797,-20.2570529048575));
#30162=CARTESIAN_POINT('Ctrl Pts',(74.2906253021832,16.7733440073046,-13.9391385430726));
#30163=CARTESIAN_POINT('Ctrl Pts',(74.409480165927,21.3937469957573,-4.23700861361877));
#30164=CARTESIAN_POINT('Ctrl Pts',(74.5283350296706,20.8200663319033,6.49380400424132));
#30165=CARTESIAN_POINT('Ctrl Pts',(74.6471898934145,15.1915831504761,15.6480175706868));
#30166=CARTESIAN_POINT('Ctrl Pts',(74.7660447571581,5.87480947415842,21.0031251520504));
#30167=CARTESIAN_POINT('Ctrl Pts',(74.8848996209019,-4.86828058592294,21.2589862563359));
#30168=CARTESIAN_POINT('Ctrl Pts',(75.0037544846456,-14.4294245095375,16.3534816119967));
#30169=CARTESIAN_POINT('Ctrl Pts',(75.1226093483894,-20.4873187232229,7.47759480337299));
#30170=CARTESIAN_POINT('Ctrl Pts',(75.2414642121331,-21.571196590871,-3.21374083403576));
#30171=CARTESIAN_POINT('Ctrl Pts',(75.3603190758769,-17.4179086831383,-13.1248279842522));
#30172=CARTESIAN_POINT('Ctrl Pts',(75.4791739396206,-9.03581154594236,-19.8494020619405));
#30173=CARTESIAN_POINT('Ctrl Pts',(75.5980288033643,1.54004627494346,-21.7548364733313));
#30174=CARTESIAN_POINT('Ctrl Pts',(75.7168836671081,11.7420037602749,-18.3785200765471));
#30175=CARTESIAN_POINT('Ctrl Pts',(75.8357385308518,19.0931773325003,-10.5401722879682));
#30176=CARTESIAN_POINT('Ctrl Pts',(75.9545933945955,21.8088113579133,-0.142827396904615));
#30177=CARTESIAN_POINT('Ctrl Pts',(76.0734482583393,19.2295902757642,10.289193862329));
#30178=CARTESIAN_POINT('Ctrl Pts',(76.1923031220829,11.9817106125957,18.2231518488533));
#30179=CARTESIAN_POINT('Ctrl Pts',(76.3111579858268,1.82484977694283,21.7327995389905));
#30180=CARTESIAN_POINT('Ctrl Pts',(76.4300128495704,-8.77505744961176,19.9660466609283));
#30181=CARTESIAN_POINT('Ctrl Pts',(76.5488677133143,-17.2445112097343,13.3518345424028));
#30182=CARTESIAN_POINT('Ctrl Pts',(76.6677225770579,-21.5272540685705,3.49599553454599));
#30183=CARTESIAN_POINT('Ctrl Pts',(76.7865774408017,-20.5834997430292,-7.20861920474871));
#30184=CARTESIAN_POINT('Ctrl Pts',(76.9054323045454,-14.6423777500227,-16.1630883910221));
#30185=CARTESIAN_POINT('Ctrl Pts',(77.0242871682892,-5.14630416684486,-21.1934000559766));
#30186=CARTESIAN_POINT('Ctrl Pts',(77.1431420320329,5.59921554412473,-21.0782693265074));
#30187=CARTESIAN_POINT('Ctrl Pts',(77.2619968957766,14.9853289795481,-15.8456482317723));
#30188=CARTESIAN_POINT('Ctrl Pts',(77.3808517595204,20.733227365848,-6.76593936614905));
#30189=CARTESIAN_POINT('Ctrl Pts',(77.4997066232641,21.4474064442648,3.95643897019295));
#30190=CARTESIAN_POINT('Ctrl Pts',(77.6185614870079,16.9544741541765,13.7182527555704));
#30191=CARTESIAN_POINT('Ctrl Pts',(77.7374163507515,8.34524764713181,20.1494787579826));
#30192=CARTESIAN_POINT('Ctrl Pts',(77.8562712144953,-2.29008089743881,21.6887109343442));
#30193=CARTESIAN_POINT('Ctrl Pts',(77.9751260782391,-12.3694118528912,17.9622466001307));
#30194=CARTESIAN_POINT('Ctrl Pts',(78.0939809419827,-19.4456335397104,9.87481588434143));
#30195=CARTESIAN_POINT('Ctrl Pts',(78.2128358057266,-21.8007445535193,-0.610073292771518));
#30196=CARTESIAN_POINT('Ctrl Pts',(78.3316906694703,-18.8629589599221,-10.9468457459968));
#30197=CARTESIAN_POINT('Ctrl Pts',(78.450545533214,-11.3455274171,-18.6258868282341));
#30198=CARTESIAN_POINT('Ctrl Pts',(78.5694003969577,-1.07357052181668,-21.7828395496326));
#30199=CARTESIAN_POINT('Ctrl Pts',(78.6882552607015,9.45903333250906,-19.651242732327));
#30200=CARTESIAN_POINT('Ctrl Pts',(78.8071101244452,17.6951245465407,-12.7486163873874));
#30201=CARTESIAN_POINT('Ctrl Pts',(78.925964988189,21.6351026415876,-2.75081555149077));
#30202=CARTESIAN_POINT('Ctrl Pts',(79.0448198519327,20.3223995224024,7.91484239654908));
#30203=CARTESIAN_POINT('Ctrl Pts',(79.1636747156765,14.0757199868426,16.6588943019143));
#30204=CARTESIAN_POINT('Ctrl Pts',(79.2825295794201,4.41166493998945,21.3584143832734));
#30205=CARTESIAN_POINT('Ctrl Pts',(79.4013844431639,-6.32347675422834,20.8724290452522));
#30206=CARTESIAN_POINT('Ctrl Pts',(79.5202393069077,-15.5233723206223,15.3189283014737));
#30207=CARTESIAN_POINT('Ctrl Pts',(79.6390941706513,-20.9544239152145,6.04621955372461));
#30208=CARTESIAN_POINT('Ctrl Pts',(79.7579490343952,-21.2980529688603,-4.694421396293));
#30209=CARTESIAN_POINT('Ctrl Pts',(79.8768038981389,-16.4708314569902,-14.2953266358547));
#30210=CARTESIAN_POINT('Ctrl Pts',(79.9956587618826,-7.64473698342631,-20.4255391352245));
#30211=CARTESIAN_POINT('Ctrl Pts',(80.1145136256263,3.03738595488812,-21.5967344538799));
#30212=CARTESIAN_POINT('Ctrl Pts',(80.23336848937,12.9820767483259,-17.5245637837559));
#30213=CARTESIAN_POINT('Ctrl Pts',(80.3522233531138,19.7749123466527,-9.19768961166646));
#30214=CARTESIAN_POINT('Ctrl Pts',(80.4710782168576,21.7666932739152,1.36224683139497));
#30215=CARTESIAN_POINT('Ctrl Pts',(80.5899330806012,18.4738447381279,11.591449999974));
#30216=CARTESIAN_POINT('Ctrl Pts',(80.7087879443451,10.6958214001617,19.0064214697612));
#30217=CARTESIAN_POINT('Ctrl Pts',(80.8276428080887,0.321011669723394,21.8069164261767));
#30218=CARTESIAN_POINT('Ctrl Pts',(80.9464976718325,-10.1317349207816,19.3130163362787));
#30219=CARTESIAN_POINT('Ctrl Pts',(81.0653525355763,-18.12464692822,12.1302030583876));
#30220=CARTESIAN_POINT('Ctrl Pts',(81.1842073993199,-21.7171641692642,2.00235685020962));
#30221=CARTESIAN_POINT('Ctrl Pts',(81.3030622630637,-20.0370768773855,-8.61163182678505));
#30222=CARTESIAN_POINT('Ctrl Pts',(81.4219171268075,-13.4922852646845,-17.1348443484828));
#30223=CARTESIAN_POINT('Ctrl Pts',(81.5407719905511,-3.67176741574004,-21.4979714520943));
#30224=CARTESIAN_POINT('Ctrl Pts',(81.6596268542949,7.04020096372379,-20.6417107551854));
#30225=CARTESIAN_POINT('Ctrl Pts',(81.7784817180386,16.042913234761,-14.7739496226393));
#30226=CARTESIAN_POINT('Ctrl Pts',(81.8973365817824,21.150644725453,-5.31929320568268));
#30227=CARTESIAN_POINT('Ctrl Pts',(82.0161914455261,21.1233141802142,5.42680850540308));
#30228=CARTESIAN_POINT('Ctrl Pts',(82.1350463092699,15.9675570490321,14.8553618063061));
#30229=CARTESIAN_POINT('Ctrl Pts',(82.2539011730136,6.935114498877,20.6772541551778));
#30230=CARTESIAN_POINT('Ctrl Pts',(82.3727560367573,-3.78107072864253,21.4790166594134));
#30231=CARTESIAN_POINT('Ctrl Pts',(82.491610900501,-13.5792682065756,17.0659933049395));
#30232=CARTESIAN_POINT('Ctrl Pts',(82.6104657642449,-20.0806212833829,8.50960054195855));
#30233=CARTESIAN_POINT('Ctrl Pts',(82.7293206279884,-21.7066981050834,-2.11279669753649));
#30234=CARTESIAN_POINT('Ctrl Pts',(82.8481754917323,-18.0627113986171,-12.2222383154895));
#30235=CARTESIAN_POINT('Ctrl Pts',(82.9670303554759,-10.0333669513822,-19.3643022112666));
#30236=CARTESIAN_POINT('Ctrl Pts',(83.0858852192198,0.431929798649459,-21.8050014712082));
#30237=CARTESIAN_POINT('Ctrl Pts',(83.2047400829634,10.7923604162288,-18.9517706074279));
#30238=CARTESIAN_POINT('Ctrl Pts',(83.3235949467072,18.5325664037399,-11.4973316470095));
#30239=CARTESIAN_POINT('Ctrl Pts',(83.442449810451,21.773340841834,-1.25151152438869));
#30240=CARTESIAN_POINT('Ctrl Pts',(83.5613046741946,19.7278718862347,9.29815698677236));
#30241=CARTESIAN_POINT('Ctrl Pts',(83.6801595379384,12.892768983884,17.5903712422038));
#30242=CARTESIAN_POINT('Ctrl Pts',(83.7990144016822,2.92749348365049,21.6119049232949));
#30243=CARTESIAN_POINT('Ctrl Pts',(83.9178692654259,-7.74853390350953,20.3863894512127));
#30244=CARTESIAN_POINT('Ctrl Pts',(84.0367241291696,-16.5433324771502,14.2113617595507));
#30245=CARTESIAN_POINT('Ctrl Pts',(84.1555789929134,-21.3216559194696,4.58602675113233));
#30246=CARTESIAN_POINT('Ctrl Pts',(84.2744338566571,-20.9233983508335,-6.15272735969124));
#30247=CARTESIAN_POINT('Ctrl Pts',(84.3932887204009,-15.4452507869423,-15.397690756695));
#30248=CARTESIAN_POINT('Ctrl Pts',(84.5121435841446,-6.21722599798435,-20.9043237967732));
#30249=CARTESIAN_POINT('Ctrl Pts',(84.6309984478883,4.52024881509651,-21.3356978596898));
#30250=CARTESIAN_POINT('Ctrl Pts',(84.7498533116321,14.1602744305448,-16.5870817373646));
#30251=CARTESIAN_POINT('Ctrl Pts',(84.8687081753757,20.3623959730666,-7.81136881387576));
#30252=CARTESIAN_POINT('Ctrl Pts',(84.9875630391196,21.6208305557273,2.86082830503407));
#30253=CARTESIAN_POINT('Ctrl Pts',(85.1064179028633,17.6300489743814,12.8384588510953));
#30254=CARTESIAN_POINT('Ctrl Pts',(85.225272766607,9.35895365531763,19.6991024919404));
#30255=CARTESIAN_POINT('Ctrl Pts',(85.3441276303508,-1.18435644657133,21.7770969671767));
#30256=CARTESIAN_POINT('Ctrl Pts',(85.4629824940945,-11.4401224142391,18.5679361173389));
#30257=CARTESIAN_POINT('Ctrl Pts',(85.5818373578382,-18.9183967707379,10.8507564775589));
#30258=CARTESIAN_POINT('Ctrl Pts',(85.700692221582,-21.8035657018886,0.499174512350522));
#30259=CARTESIAN_POINT('Ctrl Pts',(85.8195470853257,-19.3951530927588,-9.97359960188911));
#30260=CARTESIAN_POINT('Ctrl Pts',(85.9384019490694,-12.2778857125101,-18.0249320370673));
#30261=CARTESIAN_POINT('Ctrl Pts',(86.0572568128131,-2.17973024954803,-21.7000789986939));
#30262=CARTESIAN_POINT('Ctrl Pts',(86.1761116765569,8.44763130610374,-20.1067694527612));
#30263=CARTESIAN_POINT('Ctrl Pts',(86.2949665403006,17.0240335942439,-13.6318352650114));
#30264=CARTESIAN_POINT('Ctrl Pts',(86.4138214040445,21.4672536677061,-3.84729417600341));
#30265=CARTESIAN_POINT('Ctrl Pts',(86.532676267788,20.6985437619337,6.87131273088848));
#30266=CARTESIAN_POINT('Ctrl Pts',(86.651531131532,14.9045352115744,15.9216670809716));
#30267=CARTESIAN_POINT('Ctrl Pts',(86.7703859952754,5.49192713757767,21.1064774139573));
#30268=CARTESIAN_POINT('Ctrl Pts',(86.8892408590194,-5.25403918220026,21.1669488774896));
#30269=CARTESIAN_POINT('Ctrl Pts',(87.008095722763,-14.7244029144438,16.0883998994143));
#30270=CARTESIAN_POINT('Ctrl Pts',(87.1269505865068,-20.6199005662829,7.10382665518801));
#30271=CARTESIAN_POINT('Ctrl Pts',(87.2458054502505,-21.5091929720396,-3.60545006925838));
#30272=CARTESIAN_POINT('Ctrl Pts',(87.3646603139942,-17.1763731590936,-13.439377128793));
#30273=CARTESIAN_POINT('Ctrl Pts',(87.483515177738,-8.67338535036549,-20.0104232607513));
#30274=CARTESIAN_POINT('Ctrl Pts',(87.6023700414818,1.93537145092961,-21.7232361736755));
#30275=CARTESIAN_POINT('Ctrl Pts',(87.7212249052254,12.0742488423013,-18.1619703612943));
#30276=CARTESIAN_POINT('Ctrl Pts',(87.8400797689693,19.2816781550306,-10.1912482079563));
#30277=CARTESIAN_POINT('Ctrl Pts',(87.9589346327128,21.8078027241847,0.253757469630748));
#30278=CARTESIAN_POINT('Ctrl Pts',(88.0777894964568,19.0393170670483,10.6371546068841));
#30279=CARTESIAN_POINT('Ctrl Pts',(88.1966443602003,11.6483683346654,18.4380087767184));
#30280=CARTESIAN_POINT('Ctrl Pts',(88.3154992239443,1.4293689781864,21.7623885829307));
#30281=CARTESIAN_POINT('Ctrl Pts',(88.4343540876878,-9.13665991193285,19.8031840410625));
#30282=CARTESIAN_POINT('Ctrl Pts',(88.5532089514317,-17.4844436346792,13.0360608811034));
#30283=CARTESIAN_POINT('Ctrl Pts',(88.6720638151753,-21.5872644310895,3.10397598135163));
#30284=CARTESIAN_POINT('Ctrl Pts',(88.7909186789191,-20.4490184194228,-7.58170813158806));
#30285=CARTESIAN_POINT('Ctrl Pts',(88.9097735426628,-14.3460548059972,-16.4266662476692));
#30286=CARTESIAN_POINT('Ctrl Pts',(89.0286284064066,-4.7600824069233,-21.2834740583831));
#30287=CARTESIAN_POINT('Ctrl Pts',(89.1474832701503,5.98156721951559,-20.9729708458168));
#30288=CARTESIAN_POINT('Ctrl Pts',(89.266338133894,15.2709812692953,-15.5705421742144));
#30289=CARTESIAN_POINT('Ctrl Pts',(89.3851929976378,20.8528281411215,-6.38781739004154));
#30290=CARTESIAN_POINT('Ctrl Pts',(89.5040478613815,21.371918416116,4.3457744682298));
#30291=CARTESIAN_POINT('Ctrl Pts',(89.6229027251252,16.7022246916625,14.0242769125449));
#30292=CARTESIAN_POINT('Ctrl Pts',(89.741757588869,7.97747917221166,20.2978934460202));
#30293=CARTESIAN_POINT('Ctrl Pts',(89.8606124526128,-2.68407967420241,21.643483299709));
#30294=CARTESIAN_POINT('Ctrl Pts',(89.9794673163564,-12.6939838742683,17.7343571895906));
#30295=CARTESIAN_POINT('Ctrl Pts',(90.0983221801002,-19.6219775704911,9.5195929572056));
#30296=CARTESIAN_POINT('Ctrl Pts',(90.2171770438439,-21.7860468354839,-1.00638708659696));
#30297=CARTESIAN_POINT('Ctrl Pts',(90.3360319075877,-18.6607879782059,-11.2880309276121));
#30298=CARTESIAN_POINT('Ctrl Pts',(90.4548867713314,-11.004967087704,-18.829109461369));
#30299=CARTESIAN_POINT('Ctrl Pts',(90.5737416350751,-0.677304206385872,
-21.7987587216074));
#30300=CARTESIAN_POINT('Ctrl Pts',(90.692596498819,9.81479880737376,-19.4759964125881));
#30301=CARTESIAN_POINT('Ctrl Pts',(90.8114513625626,17.9240131542646,-12.4247460608585));
#30302=CARTESIAN_POINT('Ctrl Pts',(90.9303062263064,21.6815465004587,-2.35696335287487));
#30303=CARTESIAN_POINT('Ctrl Pts',(91.0491610900501,20.1751171149987,8.28307709509201));
#30304=CARTESIAN_POINT('Ctrl Pts',(91.1680159537938,13.77048037642,16.912066178113));
#30305=CARTESIAN_POINT('Ctrl Pts',(91.2868708175375,4.02255397575585,21.4351424078077));
#30306=CARTESIAN_POINT('Ctrl Pts',(91.4057256812813,-6.70194588462795,20.753917039625));
#30307=CARTESIAN_POINT('Ctrl Pts',(91.5245805450251,-15.7993971343879,15.0342790497535));
#30308=CARTESIAN_POINT('Ctrl Pts',(91.6434354087688,-21.0608241866243,5.6638924707422));
#30309=CARTESIAN_POINT('Ctrl Pts',(91.7622902725125,-21.2093216757592,-5.08031741261938));
#30310=CARTESIAN_POINT('Ctrl Pts',(91.8811451362563,-16.2078709329371,-14.5937344397854));
#30311=CARTESIAN_POINT('Ctrl Pts',(91.9603817120854,-10.2510427877187,-18.5696101441575));
#30312=CARTESIAN_POINT('Ctrl Pts',(92.,-6.97721143603873,-19.7274971949513));
#30313=CARTESIAN_POINT('Ctrl Pts',(68.3943515008351,11.9816688225107,-16.8045674163358));
#30314=CARTESIAN_POINT('Ctrl Pts',(68.4339697887497,14.7704320961965,-14.8161771685034));
#30315=CARTESIAN_POINT('Ctrl Pts',(68.5132063645788,19.3361824125128,-9.42626850397076));
#30316=CARTESIAN_POINT('Ctrl Pts',(68.6320612283226,21.4896866320246,0.953615367450808));
#30317=CARTESIAN_POINT('Ctrl Pts',(68.7509160920663,18.4259236602897,11.0993054998689));
#30318=CARTESIAN_POINT('Ctrl Pts',(68.86977095581,10.8885791501607,18.5515566076013));
#30319=CARTESIAN_POINT('Ctrl Pts',(68.9886258195538,0.707669237537231,21.4991051329555));
#30320=CARTESIAN_POINT('Ctrl Pts',(69.1074806832975,-9.64506215351249,19.2273262199953));
#30321=CARTESIAN_POINT('Ctrl Pts',(69.2263355470413,-17.6561108412412,12.2872677118917));
#30322=CARTESIAN_POINT('Ctrl Pts',(69.345190410785,-21.3805209162388,2.36413014363932));
#30323=CARTESIAN_POINT('Ctrl Pts',(69.4640452745287,-19.9140571327632,-8.13302724311118));
#30324=CARTESIAN_POINT('Ctrl Pts',(69.5829001382725,-13.6127570553459,-16.6555840786934));
#30325=CARTESIAN_POINT('Ctrl Pts',(69.7017550020162,-4.00648164543864,-21.134424195333));
#30326=CARTESIAN_POINT('Ctrl Pts',(69.82060986576,6.57250776149964,-20.4821345637842));
#30327=CARTESIAN_POINT('Ctrl Pts',(69.9394647295037,15.5557901022382,-14.8570901816477));
#30328=CARTESIAN_POINT('Ctrl Pts',(70.0583195932474,20.7623578714917,-5.62496371852402));
#30329=CARTESIAN_POINT('Ctrl Pts',(70.1771744569912,20.9281339018149,4.97281952833043));
#30330=CARTESIAN_POINT('Ctrl Pts',(70.2960293207349,16.0128702040433,14.3632765274886));
#30331=CARTESIAN_POINT('Ctrl Pts',(70.4148841844786,7.20991973289324,20.2665433649984));
#30332=CARTESIAN_POINT('Ctrl Pts',(70.5337390482224,-3.34349204314369,21.2493949313972));
#30333=CARTESIAN_POINT('Ctrl Pts',(70.6525939119661,-13.0851536662652,17.0732093289622));
#30334=CARTESIAN_POINT('Ctrl Pts',(70.7714487757099,-19.64993455209,8.75190240077688));
#30335=CARTESIAN_POINT('Ctrl Pts',(70.8903036394536,-21.4440035165991,-1.69423630556385));
#30336=CARTESIAN_POINT('Ctrl Pts',(71.0091585031973,-18.0317872930387,-11.7290396229207));
#30337=CARTESIAN_POINT('Ctrl Pts',(71.1280133669411,-10.2417212416112,-18.9162065303833));
#30338=CARTESIAN_POINT('Ctrl Pts',(71.2468682306848,0.0348824360666644,
-21.5107997685402));
#30339=CARTESIAN_POINT('Ctrl Pts',(71.3657230944286,10.3030171769846,-18.8828906825855));
#30340=CARTESIAN_POINT('Ctrl Pts',(71.4845779581722,18.0697325499298,-11.6704965210695));
#30341=CARTESIAN_POINT('Ctrl Pts',(71.603432821916,21.4493855509768,-1.62467934106641));
#30342=CARTESIAN_POINT('Ctrl Pts',(71.7222876856598,19.6214466858341,8.81558582459576));
#30343=CARTESIAN_POINT('Ctrl Pts',(71.8411425494034,13.02971233009,17.1155578369645));
#30344=CARTESIAN_POINT('Ctrl Pts',(71.9599974131473,3.27455756830758,21.2601269094897));
#30345=CARTESIAN_POINT('Ctrl Pts',(72.0788522768909,-7.27561107942226,20.2430532997501));
#30346=CARTESIAN_POINT('Ctrl Pts',(72.1977071406346,-16.0593695431082,14.3112673566504));
#30347=CARTESIAN_POINT('Ctrl Pts',(72.3165620043785,-20.9441518794822,4.90491850337913));
#30348=CARTESIAN_POINT('Ctrl Pts',(72.4354168681221,-20.7440055724437,-5.69227162792107));
#30349=CARTESIAN_POINT('Ctrl Pts',(72.554271731866,-15.5075231692293,-14.907462850245));
#30350=CARTESIAN_POINT('Ctrl Pts',(72.6731265956095,-6.50604473249943,-20.5033437617947));
#30351=CARTESIAN_POINT('Ctrl Pts',(72.7919814593534,4.07500462245026,-21.1213176862293));
#30352=CARTESIAN_POINT('Ctrl Pts',(72.910836323097,13.6667034491012,-16.6113497437727));
#30353=CARTESIAN_POINT('Ctrl Pts',(73.0296911868409,19.9403298978757,-8.06839308905427));
#30354=CARTESIAN_POINT('Ctrl Pts',(73.1485460505845,21.3727407538559,2.43344943322881));
#30355=CARTESIAN_POINT('Ctrl Pts',(73.2674009143284,17.616167960707,12.3444866177486));
#30356=CARTESIAN_POINT('Ctrl Pts',(73.386255778072,9.58265153355406,19.2584660100977));
#30357=CARTESIAN_POINT('Ctrl Pts',(73.5051106418158,-0.777390194942946,
21.4967762225042));
#30358=CARTESIAN_POINT('Ctrl Pts',(73.6239655055596,-10.9486931436546,18.5159888183619));
#30359=CARTESIAN_POINT('Ctrl Pts',(73.7428203693032,-18.4618162006971,11.0397946560292));
#30360=CARTESIAN_POINT('Ctrl Pts',(73.861675233047,-21.4926848055884,0.883302509473593));
#30361=CARTESIAN_POINT('Ctrl Pts',(73.9805300967907,-19.3054491291201,-9.48764235195281));
#30362=CARTESIAN_POINT('Ctrl Pts',(74.0993849605345,-12.4311374700347,-17.5551287285714));
#30363=CARTESIAN_POINT('Ctrl Pts',(74.2182398242782,-2.53873048031433,-21.3604908891143));
#30364=CARTESIAN_POINT('Ctrl Pts',(74.3370946880219,7.97004251990571,-19.9798434855358));
#30365=CARTESIAN_POINT('Ctrl Pts',(74.4559495517657,16.5438077083086,-13.7483871776337));
#30366=CARTESIAN_POINT('Ctrl Pts',(74.5748044155094,21.1009823863315,-4.17902689717862));
#30367=CARTESIAN_POINT('Ctrl Pts',(74.6936592792532,20.535152305899,6.40493897310086));
#30368=CARTESIAN_POINT('Ctrl Pts',(74.8125141429969,14.9836925968255,15.4338809001317));
#30369=CARTESIAN_POINT('Ctrl Pts',(74.9313690067407,5.79441512802099,20.7157060415467));
#30370=CARTESIAN_POINT('Ctrl Pts',(75.0502238704844,-4.80166017274356,20.9680657920826));
#30371=CARTESIAN_POINT('Ctrl Pts',(75.1690787342281,-14.2319637827367,16.1296909568189));
#30372=CARTESIAN_POINT('Ctrl Pts',(75.2879335979719,-20.2069582110894,7.37526700065154));
#30373=CARTESIAN_POINT('Ctrl Pts',(75.4067884617155,-21.2760036568783,-3.16976211538219));
#30374=CARTESIAN_POINT('Ctrl Pts',(75.5256433254593,-17.1795517822342,-12.9452201231631));
#30375=CARTESIAN_POINT('Ctrl Pts',(75.644498189203,-8.91216018937456,-19.577771176376));
#30376=CARTESIAN_POINT('Ctrl Pts',(75.7633530529468,1.51897137645698,-21.457130503241));
#30377=CARTESIAN_POINT('Ctrl Pts',(75.8822079166905,11.5813192787095,-18.1270176046752));
#30378=CARTESIAN_POINT('Ctrl Pts',(76.0010627804343,18.8318950706527,-10.3959343747228));
#30379=CARTESIAN_POINT('Ctrl Pts',(76.119917644178,21.5103667637752,-0.140872862849453));
#30380=CARTESIAN_POINT('Ctrl Pts',(76.2387725079217,18.9664412590155,10.1483904853886));
#30381=CARTESIAN_POINT('Ctrl Pts',(76.3576273716655,11.8177458415602,17.9737755271368));
#30382=CARTESIAN_POINT('Ctrl Pts',(76.4764822354092,1.79987745992357,21.4353951352633));
#30383=CARTESIAN_POINT('Ctrl Pts',(76.595337099153,-8.65497440537299,19.692819542106));
#30384=CARTESIAN_POINT('Ctrl Pts',(76.7141919628966,-17.0085271817818,13.1691201901343));
#30385=CARTESIAN_POINT('Ctrl Pts',(76.8330468266405,-21.2326624698831,3.44815427665745));
#30386=CARTESIAN_POINT('Ctrl Pts',(76.9519016903841,-20.301823033284,-7.10997222222639));
#30387=CARTESIAN_POINT('Ctrl Pts',(77.0707565541279,-14.4420028459023,-15.9419031885959));
#30388=CARTESIAN_POINT('Ctrl Pts',(77.1896114178716,-5.07587911555805,-20.9033771118414));
#30389=CARTESIAN_POINT('Ctrl Pts',(77.3084662816153,5.52259258732379,-20.7898218989497));
#30390=CARTESIAN_POINT('Ctrl Pts',(77.4273211453592,14.7802609292115,-15.6288070670808));
#30391=CARTESIAN_POINT('Ctrl Pts',(77.5461760091027,20.4495016953003,-6.67335027475135));
#30392=CARTESIAN_POINT('Ctrl Pts',(77.6650308728467,21.1539075274039,3.90229673367615));
#30393=CARTESIAN_POINT('Ctrl Pts',(77.7838857365902,16.7224591637799,13.5305241210874));
#30394=CARTESIAN_POINT('Ctrl Pts',(77.9027406003341,8.23104637287821,19.8737414465204));
#30395=CARTESIAN_POINT('Ctrl Pts',(78.0215954640777,-2.25874208429753,21.3919098649989));
#30396=CARTESIAN_POINT('Ctrl Pts',(78.1404503278216,-12.2001415501875,17.7164406592014));
#30397=CARTESIAN_POINT('Ctrl Pts',(78.2593051915652,-19.1795280599448,9.73968309922879));
#30398=CARTESIAN_POINT('Ctrl Pts',(78.378160055309,-21.5024103502743,-0.601724691223848));
#30399=CARTESIAN_POINT('Ctrl Pts',(78.4970149190527,-18.6048271416103,-10.7970426741036));
#30400=CARTESIAN_POINT('Ctrl Pts',(78.6158697827966,-11.1902685508688,-18.3709992443266));
#30401=CARTESIAN_POINT('Ctrl Pts',(78.7347246465401,-1.05887915173673,-21.4847503689857));
#30402=CARTESIAN_POINT('Ctrl Pts',(78.8535795102839,9.32959036023836,-19.3823235755097));
#30403=CARTESIAN_POINT('Ctrl Pts',(78.9724343740277,17.4529740608107,-12.5741568269321));
#30404=CARTESIAN_POINT('Ctrl Pts',(79.0912892377714,21.3390351796321,-2.7131717745173));
#30405=CARTESIAN_POINT('Ctrl Pts',(79.2101441015152,20.0442958615546,7.80653104074255));
#30406=CARTESIAN_POINT('Ctrl Pts',(79.3289989652589,13.8830995606427,16.430924199962));
#30407=CARTESIAN_POINT('Ctrl Pts',(79.4478538290026,4.35129312371388,21.0661332860859));
#30408=CARTESIAN_POINT('Ctrl Pts',(79.5667086927464,-6.23694258129774,20.5867984570989));
#30409=CARTESIAN_POINT('Ctrl Pts',(79.6855635564901,-15.3109413689372,15.1092950819216));
#30410=CARTESIAN_POINT('Ctrl Pts',(79.8044184202338,-20.6676712610629,5.96347953130122));
#30411=CARTESIAN_POINT('Ctrl Pts',(79.9232732839776,-21.0065978927488,-4.63018017446131));
#30412=CARTESIAN_POINT('Ctrl Pts',(80.0421281477213,-16.2454349175536,-14.099700983182));
#30413=CARTESIAN_POINT('Ctrl Pts',(80.160983011465,-7.54012190886456,-20.1460240512879));
#30414=CARTESIAN_POINT('Ctrl Pts',(80.2798378752088,2.99582058006459,-21.3011920447583));
#30415=CARTESIAN_POINT('Ctrl Pts',(80.3986927389524,12.8044223790604,-17.2847473517617));
#30416=CARTESIAN_POINT('Ctrl Pts',(80.5175476026964,19.5043008221382,-9.07182302049318));
#30417=CARTESIAN_POINT('Ctrl Pts',(80.6364024664399,21.4688250483962,1.34360504500695));
#30418=CARTESIAN_POINT('Ctrl Pts',(80.7552573301838,18.2210377875538,11.4328257845622));
#30419=CARTESIAN_POINT('Ctrl Pts',(80.8741121939274,10.5494534929724,18.7463264261355));
#30420=CARTESIAN_POINT('Ctrl Pts',(80.9929670576712,0.316618757339831,21.5084977633984));
#30421=CARTESIAN_POINT('Ctrl Pts',(81.111821921415,-9.99308630455384,19.048725668279));
#30422=CARTESIAN_POINT('Ctrl Pts',(81.2306767851586,-17.87661860574,11.964206229438));
#30423=CARTESIAN_POINT('Ctrl Pts',(81.3495316489024,-21.4199737291271,1.9749554220587));
#30424=CARTESIAN_POINT('Ctrl Pts',(81.4683865126461,-19.7628777393287,-8.49378519483287));
#30425=CARTESIAN_POINT('Ctrl Pts',(81.5872413763899,-13.3076489021735,-16.9003610663233));
#30426=CARTESIAN_POINT('Ctrl Pts',(81.7060962401336,-3.62152079210815,-21.2037805739435));
#30427=CARTESIAN_POINT('Ctrl Pts',(81.8249511038774,6.94385871541021,-20.3592374517327));
#30428=CARTESIAN_POINT('Ctrl Pts',(81.943805967621,15.8233725798136,-14.5717742116742));
#30429=CARTESIAN_POINT('Ctrl Pts',(82.0626608313649,20.8612068703929,-5.24650087070311));
#30430=CARTESIAN_POINT('Ctrl Pts',(82.1815156951085,20.8342503324003,5.35254486786322));
#30431=CARTESIAN_POINT('Ctrl Pts',(82.3003705588522,15.7490476124256,14.6520723031646));
#30432=CARTESIAN_POINT('Ctrl Pts',(82.4192254225961,6.84021031551958,20.3942944549468));
#30433=CARTESIAN_POINT('Ctrl Pts',(82.5380802863397,-3.72932833422693,21.1850851697874));
#30434=CARTESIAN_POINT('Ctrl Pts',(82.6569351500835,-13.3934415183581,16.8324522209313));
#30435=CARTESIAN_POINT('Ctrl Pts',(82.7757900138273,-19.8058262580784,8.39315016608327));
#30436=CARTESIAN_POINT('Ctrl Pts',(82.8946448775708,-21.4096508887207,-2.08388394559674));
#30437=CARTESIAN_POINT('Ctrl Pts',(83.0134997413149,-17.8155306383307,-12.0549820219822));
#30438=CARTESIAN_POINT('Ctrl Pts',(83.1323546050583,-9.89606446026975,-19.099309717207));
#30439=CARTESIAN_POINT('Ctrl Pts',(83.2512094688023,0.42601901739055,-21.5066090137993));
#30440=CARTESIAN_POINT('Ctrl Pts',(83.3700643325459,10.6446714123967,-18.692423438327));
#30441=CARTESIAN_POINT('Ctrl Pts',(83.4889191962897,18.2789558713762,-11.3399954024637));
#30442=CARTESIAN_POINT('Ctrl Pts',(83.6077740600334,21.475381647088,-1.23438510503342));
#30443=CARTESIAN_POINT('Ctrl Pts',(83.726628923777,19.4579040910317,9.17091554098207));
#30444=CARTESIAN_POINT('Ctrl Pts',(83.8454837875209,12.7163367545633,17.3496542622657));
#30445=CARTESIAN_POINT('Ctrl Pts',(83.9643386512646,2.88743194199966,21.3161549125525));
#30446=CARTESIAN_POINT('Ctrl Pts',(84.0831935150084,-7.64249841088016,20.1074101145649));
#30447=CARTESIAN_POINT('Ctrl Pts',(84.202048378752,-16.3169437911367,14.016885131601));
#30448=CARTESIAN_POINT('Ctrl Pts',(84.3209032424959,-21.0298778467078,4.52326886534082));
#30449=CARTESIAN_POINT('Ctrl Pts',(84.4397581062395,-20.6370702687422,-6.0685298218443));
#30450=CARTESIAN_POINT('Ctrl Pts',(84.5586129699834,-15.233888896245,-15.1869797054081));
#30451=CARTESIAN_POINT('Ctrl Pts',(84.677467833727,-6.13214582285781,-20.618256742092));
#30452=CARTESIAN_POINT('Ctrl Pts',(84.7963226974707,4.45839107324696,-21.043727628764));
#30453=CARTESIAN_POINT('Ctrl Pts',(84.9151775612146,13.966496911635,-16.360094360758));
#30454=CARTESIAN_POINT('Ctrl Pts',(85.0340324249581,20.0837449772775,-7.70447345139769));
#30455=CARTESIAN_POINT('Ctrl Pts',(85.1528872887021,21.324958401384,2.82167904887415));
#30456=CARTESIAN_POINT('Ctrl Pts',(85.2717421524456,17.388789021033,12.662769833556));
#30457=CARTESIAN_POINT('Ctrl Pts',(85.3905970161895,9.23088023217779,19.4295283940399));
#30458=CARTESIAN_POINT('Ctrl Pts',(85.5094518799331,-1.1681490167756,21.4790863714037));
#30459=CARTESIAN_POINT('Ctrl Pts',(85.628306743677,-11.2835690544629,18.3138415650235));
#30460=CARTESIAN_POINT('Ctrl Pts',(85.7471616074206,-18.6595063088358,10.7022683476975));
#30461=CARTESIAN_POINT('Ctrl Pts',(85.8660164711644,-21.5051928923911,0.492343514901928));
#30462=CARTESIAN_POINT('Ctrl Pts',(85.9848713349081,-19.1297384171023,-9.83711500231921));
#30463=CARTESIAN_POINT('Ctrl Pts',(86.1037261986519,-12.1098679073116,-17.7782682717715));
#30464=CARTESIAN_POINT('Ctrl Pts',(86.2225810623956,-2.14990153953807,-21.4031223620739));
#30465=CARTESIAN_POINT('Ctrl Pts',(86.3414359261394,8.33202895367829,-19.8316166005366));
#30466=CARTESIAN_POINT('Ctrl Pts',(86.4602907898831,16.7910667115815,-13.4452892182666));
#30467=CARTESIAN_POINT('Ctrl Pts',(86.5791456536268,21.1734831497732,-3.79464554100704));
#30468=CARTESIAN_POINT('Ctrl Pts',(86.6980005173705,20.4152927222094,6.77728164842781));
#30469=CARTESIAN_POINT('Ctrl Pts',(86.8168553811144,14.7005727906504,15.7037856296628));
#30470=CARTESIAN_POINT('Ctrl Pts',(86.9357102448579,5.41677237839747,20.8176439703498));
#30471=CARTESIAN_POINT('Ctrl Pts',(87.0545651086018,-5.18213982163527,20.8772879068292));
#30472=CARTESIAN_POINT('Ctrl Pts',(87.1734199723454,-14.522905529758,15.8682367782101));
#30473=CARTESIAN_POINT('Ctrl Pts',(87.2922748360894,-20.3377257262755,7.00661371551234));
#30474=CARTESIAN_POINT('Ctrl Pts',(87.4111296998329,-21.2148485320136,-3.55611097117801));
#30475=CARTESIAN_POINT('Ctrl Pts',(87.5299845635768,-16.9413215722784,-13.2554647923137));
#30476=CARTESIAN_POINT('Ctrl Pts',(87.6488394273203,-8.55469364689703,-19.7365888664518));
#30477=CARTESIAN_POINT('Ctrl Pts',(87.7676942910644,1.9088866903574,-21.4259626406608));
#30478=CARTESIAN_POINT('Ctrl Pts',(87.8865491548077,11.9090177237354,-17.9134312830168));
#30479=CARTESIAN_POINT('Ctrl Pts',(88.0054040185518,19.0178163371241,-10.0517851769242));
#30480=CARTESIAN_POINT('Ctrl Pts',(88.1242588822953,21.5093719327835,0.250284903254255));
#30481=CARTESIAN_POINT('Ctrl Pts',(88.2431137460391,18.7787718607328,10.4915895305791));
#30482=CARTESIAN_POINT('Ctrl Pts',(88.3619686097829,11.4889652153043,18.1856922265052));
#30483=CARTESIAN_POINT('Ctrl Pts',(88.4808234735266,1.40980865288631,21.4645792653335));
#30484=CARTESIAN_POINT('Ctrl Pts',(88.5996783372704,-9.01162848704484,19.5321856300632));
#30485=CARTESIAN_POINT('Ctrl Pts',(88.718533201014,-17.2451762303881,12.8576677612322));
#30486=CARTESIAN_POINT('Ctrl Pts',(88.8373880647578,-21.2918516153265,3.06149934946342));
#30487=CARTESIAN_POINT('Ctrl Pts',(88.9562429285016,-20.1691820311599,-7.47795558088412));
#30488=CARTESIAN_POINT('Ctrl Pts',(89.0750977922452,-14.1497349592255,-16.2018740909179));
#30489=CARTESIAN_POINT('Ctrl Pts',(89.193952655989,-4.69494264122567,-20.9922184886523));
#30490=CARTESIAN_POINT('Ctrl Pts',(89.3128075197327,5.89971193763708,-20.6859643845647));
#30491=CARTESIAN_POINT('Ctrl Pts',(89.4316623834766,15.0620041851155,-15.3574657225257));
#30492=CARTESIAN_POINT('Ctrl Pts',(89.5505172472201,20.567465783262,-6.30040274203012));
#30493=CARTESIAN_POINT('Ctrl Pts',(89.669372110964,21.0794525218052,4.28630433590113));
#30494=CARTESIAN_POINT('Ctrl Pts',(89.7882269747077,16.4736616311866,13.8323604636127));
#30495=CARTESIAN_POINT('Ctrl Pts',(89.9070818384515,7.86831065794818,20.0201251407266));
#30496=CARTESIAN_POINT('Ctrl Pts',(90.0259367021951,-2.64734915020205,21.3473011519015));
#30497=CARTESIAN_POINT('Ctrl Pts',(90.1447915659389,-12.5202719372362,17.4916698213115));
#30498=CARTESIAN_POINT('Ctrl Pts',(90.2636464296827,-19.3534588953509,9.3893212514328));
#30499=CARTESIAN_POINT('Ctrl Pts',(90.3825012934263,-21.4879137644521,-0.992615094135966));
#30500=CARTESIAN_POINT('Ctrl Pts',(90.5013561571702,-18.4054227864468,-11.1335588771404));
#30501=CARTESIAN_POINT('Ctrl Pts',(90.6202110209139,-10.8543686492063,-18.5714408594927));
#30502=CARTESIAN_POINT('Ctrl Pts',(90.7390658846576,-0.668035577497034,
-21.5004516936536));
#30503=CARTESIAN_POINT('Ctrl Pts',(90.8579207484013,9.68048733122125,-19.2094754294223));
#30504=CARTESIAN_POINT('Ctrl Pts',(90.976775612145,17.6787304222826,-12.2547185323268));
#30505=CARTESIAN_POINT('Ctrl Pts',(91.0956304758889,21.3848434734381,-2.32470928089896));
#30506=CARTESIAN_POINT('Ctrl Pts',(91.2144853396325,19.8990289531884,8.16972659921727));
#30507=CARTESIAN_POINT('Ctrl Pts',(91.3333402033763,13.5820370284732,16.6806315233889));
#30508=CARTESIAN_POINT('Ctrl Pts',(91.45219506712,3.96750698263957,21.1418113192306));
#30509=CARTESIAN_POINT('Ctrl Pts',(91.5710499308638,-6.61023251764766,20.4699082394197));
#30510=CARTESIAN_POINT('Ctrl Pts',(91.6899047946075,-15.5831888969001,14.8285411378826));
#30511=CARTESIAN_POINT('Ctrl Pts',(91.8087596583512,-20.7726154886153,5.58638443685941));
#30512=CARTESIAN_POINT('Ctrl Pts',(91.927614522095,-20.91908085082,-5.01079536286535));
#30513=CARTESIAN_POINT('Ctrl Pts',(92.0464693858386,-15.9860728998834,-14.3940251993155));
#30514=CARTESIAN_POINT('Ctrl Pts',(92.1257059616679,-10.110761492509,-18.3154926834751));
#30515=CARTESIAN_POINT('Ctrl Pts',(92.1653242495824,-6.88173117344805,-19.457534527244));
#30516=CARTESIAN_POINT('Ctrl Pts',(68.5596757504176,11.8154297096169,-16.5714132187663));
#30517=CARTESIAN_POINT('Ctrl Pts',(68.5992940383321,14.5655004155514,-14.610610799957));
#30518=CARTESIAN_POINT('Ctrl Pts',(68.6785306141613,19.0679034391389,-9.29548417524227));
#30519=CARTESIAN_POINT('Ctrl Pts',(68.797385477905,21.1915289634232,0.940384474903618));
#30520=CARTESIAN_POINT('Ctrl Pts',(68.9162403416488,18.1702740300995,10.9453086963044));
#30521=CARTESIAN_POINT('Ctrl Pts',(69.0350952053925,10.7375060596412,18.2941638888631));
#30522=CARTESIAN_POINT('Ctrl Pts',(69.1539500691362,0.6978507132554,21.2008167877962));
#30523=CARTESIAN_POINT('Ctrl Pts',(69.27280493288,-9.51124218235847,18.9605575668569));
#30524=CARTESIAN_POINT('Ctrl Pts',(69.3916597966237,-17.4111419435958,12.1167885812654));
#30525=CARTESIAN_POINT('Ctrl Pts',(69.5105146603675,-21.0838778623392,2.33132912871676));
#30526=CARTESIAN_POINT('Ctrl Pts',(69.6293695241111,-19.6377604631667,-8.02018593076447));
#30527=CARTESIAN_POINT('Ctrl Pts',(69.748224387855,-13.4238874837994,-16.4244969435884));
#30528=CARTESIAN_POINT('Ctrl Pts',(69.8670792515985,-3.95089390015628,-20.8411955990666));
#30529=CARTESIAN_POINT('Ctrl Pts',(69.9859341153425,6.48131780491308,-20.1979561300039));
#30530=CARTESIAN_POINT('Ctrl Pts',(70.1047889790861,15.3399620080666,-14.6509561673825));
#30531=CARTESIAN_POINT('Ctrl Pts',(70.2236438428299,20.4742914923196,-5.5469204181725));
#30532=CARTESIAN_POINT('Ctrl Pts',(70.3424987065737,20.637767470736,4.90382437254567));
#30533=CARTESIAN_POINT('Ctrl Pts',(70.4613535703173,15.7907003730259,14.1639939080515));
#30534=CARTESIAN_POINT('Ctrl Pts',(70.5802084340611,7.10988603323194,19.985356141388));
#30535=CARTESIAN_POINT('Ctrl Pts',(70.6990632978048,-3.29710291659937,20.9545711789422));
#30536=CARTESIAN_POINT('Ctrl Pts',(70.8179181615486,-12.9036043036696,16.8363278715341));
#30537=CARTESIAN_POINT('Ctrl Pts',(70.9367730252922,-19.3773024390889,8.63047453352477));
#30538=CARTESIAN_POINT('Ctrl Pts',(71.0556278890361,-21.1464796762811,-1.67072970188107));
#30539=CARTESIAN_POINT('Ctrl Pts',(71.1744827527797,-17.7816060897448,-11.5663056022351));
#30540=CARTESIAN_POINT('Ctrl Pts',(71.2933376165235,-10.099622951387,-18.6537544930662));
#30541=CARTESIAN_POINT('Ctrl Pts',(71.4121924802672,0.0343984613121467,
-21.2123491666975));
#30542=CARTESIAN_POINT('Ctrl Pts',(71.531047344011,10.1600684391248,-18.6209008844661));
#30543=CARTESIAN_POINT('Ctrl Pts',(71.6499022077547,17.8190248769147,-11.5085747539573));
#30544=CARTESIAN_POINT('Ctrl Pts',(71.7687570714985,21.1517870378704,-1.60213780228773));
#30545=CARTESIAN_POINT('Ctrl Pts',(71.8876119352421,19.3492098264228,8.6932743846095));
#30546=CARTESIAN_POINT('Ctrl Pts',(72.006466798986,12.8489321857626,16.8780888171102));
#30547=CARTESIAN_POINT('Ctrl Pts',(72.1253216627296,3.2291248699632,20.9651542566983));
#30548=CARTESIAN_POINT('Ctrl Pts',(72.2441765264735,-7.17466594819554,19.9621919879694));
#30549=CARTESIAN_POINT('Ctrl Pts',(72.3630313902171,-15.8365545591501,14.1127063360615));
#30550=CARTESIAN_POINT('Ctrl Pts',(72.4818862539609,-20.6535632077091,4.83686543724142));
#30551=CARTESIAN_POINT('Ctrl Pts',(72.6007411177046,-20.4561938214004,-5.61329446707699));
#30552=CARTESIAN_POINT('Ctrl Pts',(72.7195959814484,-15.2923647523993,-14.7006299427066));
#30553=CARTESIAN_POINT('Ctrl Pts',(72.838450845192,-6.41577691415126,-20.2188710619723));
#30554=CARTESIAN_POINT('Ctrl Pts',(72.9573057089359,4.01846615827561,-20.8282709356206));
#30555=CARTESIAN_POINT('Ctrl Pts',(73.0761605726795,13.4770854007962,-16.3808763359127));
#30556=CARTESIAN_POINT('Ctrl Pts',(73.1950154364233,19.6636687080083,-7.95644854030465));
#30557=CARTESIAN_POINT('Ctrl Pts',(73.3138703001669,21.0762056454613,2.39968665101172));
#30558=CARTESIAN_POINT('Ctrl Pts',(73.4327251639109,17.37175324872,12.1732136060453));
#30559=CARTESIAN_POINT('Ctrl Pts',(73.5515800276544,9.44969747567559,18.991265309374));
#30560=CARTESIAN_POINT('Ctrl Pts',(73.6704348913983,-0.766604330444966,
21.1985201897058));
#30561=CARTESIAN_POINT('Ctrl Pts',(73.7892897551419,-10.7967860042978,18.2590895832793));
#30562=CARTESIAN_POINT('Ctrl Pts',(73.9081446188858,-18.2056685811062,10.8866235329299));
#30563=CARTESIAN_POINT('Ctrl Pts',(74.0269994826294,-21.1944855389658,0.871047169439829));
#30564=CARTESIAN_POINT('Ctrl Pts',(74.1458543463732,-19.0375965632729,-9.35600649459388));
#30565=CARTESIAN_POINT('Ctrl Pts',(74.2647092101169,-12.2586622250674,-17.3115609026028));
#30566=CARTESIAN_POINT('Ctrl Pts',(74.3835640738607,-2.50350698105258,-21.0641257409046));
#30567=CARTESIAN_POINT('Ctrl Pts',(74.5024189376044,7.85946253160344,-19.7026340662141));
#30568=CARTESIAN_POINT('Ctrl Pts',(74.6212738013481,16.3142714093126,-13.5576358121948));
#30569=CARTESIAN_POINT('Ctrl Pts',(74.7401286650918,20.8082177769057,-4.12104518073847));
#30570=CARTESIAN_POINT('Ctrl Pts',(74.8589835288356,20.2502382798946,6.31607394196041));
#30571=CARTESIAN_POINT('Ctrl Pts',(74.9778383925794,14.7758020431749,15.2197442295766));
#30572=CARTESIAN_POINT('Ctrl Pts',(75.096693256323,5.71402078188356,20.428286931043));
#30573=CARTESIAN_POINT('Ctrl Pts',(75.2155481200669,-4.73503975956417,20.6771453278292));
#30574=CARTESIAN_POINT('Ctrl Pts',(75.3344029838105,-14.034503055936,15.9059003016411));
#30575=CARTESIAN_POINT('Ctrl Pts',(75.4532578475543,-19.9265976989558,7.2729391979301));
#30576=CARTESIAN_POINT('Ctrl Pts',(75.5721127112981,-20.9808107228857,-3.12578339672864));
#30577=CARTESIAN_POINT('Ctrl Pts',(75.6909675750417,-16.9411948813302,-12.7656122620739));
#30578=CARTESIAN_POINT('Ctrl Pts',(75.8098224387856,-8.78850883280678,-19.3061402908116));
#30579=CARTESIAN_POINT('Ctrl Pts',(75.9286773025292,1.49789647797051,-21.1594245331508));
#30580=CARTESIAN_POINT('Ctrl Pts',(76.0475321662729,11.4206347971442,-17.8755151328033));
#30581=CARTESIAN_POINT('Ctrl Pts',(76.1663870300168,18.570612808805,-10.2516964614774));
#30582=CARTESIAN_POINT('Ctrl Pts',(76.2852418937604,21.2119221696372,-0.138918328794305));
#30583=CARTESIAN_POINT('Ctrl Pts',(76.4040967575042,18.7032922422669,10.0075871084483));
#30584=CARTESIAN_POINT('Ctrl Pts',(76.5229516212479,11.6537810705247,17.7243992054202));
#30585=CARTESIAN_POINT('Ctrl Pts',(76.6418064849917,1.7749051429043,21.1379907315363));
#30586=CARTESIAN_POINT('Ctrl Pts',(76.7606613487353,-8.53489136113423,19.4195924232837));
#30587=CARTESIAN_POINT('Ctrl Pts',(76.8795162124791,-16.7725431538293,12.9864058378659));
#30588=CARTESIAN_POINT('Ctrl Pts',(76.9983710762229,-20.9380708711956,3.4003130187689));
#30589=CARTESIAN_POINT('Ctrl Pts',(77.1172259399666,-20.0201463235389,-7.01132523970409));
#30590=CARTESIAN_POINT('Ctrl Pts',(77.2360808037103,-14.2416279417819,-15.7207179861697));
#30591=CARTESIAN_POINT('Ctrl Pts',(77.3549356674541,-5.00545406427125,-20.6133541677062));
#30592=CARTESIAN_POINT('Ctrl Pts',(77.4737905311978,5.44596963052285,-20.501374471392));
#30593=CARTESIAN_POINT('Ctrl Pts',(77.5926453949415,14.5751928788749,-15.4119659023894));
#30594=CARTESIAN_POINT('Ctrl Pts',(77.7115002586853,20.1657760247526,-6.58076118335362));
#30595=CARTESIAN_POINT('Ctrl Pts',(77.8303551224291,20.8604086105429,3.84815449715933));
#30596=CARTESIAN_POINT('Ctrl Pts',(77.9492099861727,16.4904441733833,13.3427954866044));
#30597=CARTESIAN_POINT('Ctrl Pts',(78.0680648499165,8.11684509862461,19.5980041350581));
#30598=CARTESIAN_POINT('Ctrl Pts',(78.1869197136602,-2.22740327115626,21.0951087956537));
#30599=CARTESIAN_POINT('Ctrl Pts',(78.305774577404,-12.0308712474838,17.4706347182719));
#30600=CARTESIAN_POINT('Ctrl Pts',(78.4246294411476,-18.9134225801791,9.60455031411619));
#30601=CARTESIAN_POINT('Ctrl Pts',(78.5434843048915,-21.2040761470294,-0.593376089676207));
#30602=CARTESIAN_POINT('Ctrl Pts',(78.6623391686352,-18.3466953232985,-10.6472396022104));
#30603=CARTESIAN_POINT('Ctrl Pts',(78.7811940323789,-11.0350096846377,-18.1161116604191));
#30604=CARTESIAN_POINT('Ctrl Pts',(78.9000488961227,-1.04418778165678,-21.1866611883387));
#30605=CARTESIAN_POINT('Ctrl Pts',(79.0189037598663,9.2001473879677,-19.1134044186924));
#30606=CARTESIAN_POINT('Ctrl Pts',(79.1377586236102,17.2108235750806,-12.3996972664767));
#30607=CARTESIAN_POINT('Ctrl Pts',(79.2566134873538,21.0429677176766,-2.67552799754383));
#30608=CARTESIAN_POINT('Ctrl Pts',(79.3754683510976,19.7661922007068,7.69821968493602));
#30609=CARTESIAN_POINT('Ctrl Pts',(79.4943232148413,13.6904791344428,16.2029540980096));
#30610=CARTESIAN_POINT('Ctrl Pts',(79.6131780785851,4.29092130743831,20.7738521888983));
#30611=CARTESIAN_POINT('Ctrl Pts',(79.7320329423288,-6.15040840836714,20.3011678689456));
#30612=CARTESIAN_POINT('Ctrl Pts',(79.8508878060725,-15.0985104172522,14.8996618623695));
#30613=CARTESIAN_POINT('Ctrl Pts',(79.9697426698163,-20.3809186069113,5.88073950887784));
#30614=CARTESIAN_POINT('Ctrl Pts',(80.08859753356,-20.7151428166373,-4.56593895262964));
#30615=CARTESIAN_POINT('Ctrl Pts',(80.2074523973038,-16.0200383781171,-13.9040753305092));
#30616=CARTESIAN_POINT('Ctrl Pts',(80.3263072610475,-7.43550683430282,-19.8665089673515));
#30617=CARTESIAN_POINT('Ctrl Pts',(80.4451621247912,2.9542552052411,-21.0056496356368));
#30618=CARTESIAN_POINT('Ctrl Pts',(80.564016988535,12.6267680097947,-17.0449309197675));
#30619=CARTESIAN_POINT('Ctrl Pts',(80.6828718522787,19.2336892976239,-8.94595642931989));
#30620=CARTESIAN_POINT('Ctrl Pts',(80.8017267160225,21.1709568228772,1.32496325861892));
#30621=CARTESIAN_POINT('Ctrl Pts',(80.9205815797661,17.9682308369797,11.2742015691503));
#30622=CARTESIAN_POINT('Ctrl Pts',(81.03943644351,10.403085585783,18.4862313825099));
#30623=CARTESIAN_POINT('Ctrl Pts',(81.1582913072536,0.312225844956285,21.2100791006201));
#30624=CARTESIAN_POINT('Ctrl Pts',(81.2771461709974,-9.85443768832609,18.7844350002794));
#30625=CARTESIAN_POINT('Ctrl Pts',(81.3960010347411,-17.6285902832599,11.7982094004884));
#30626=CARTESIAN_POINT('Ctrl Pts',(81.5148558984849,-21.12278328899,1.9475539939078));
#30627=CARTESIAN_POINT('Ctrl Pts',(81.6337107622286,-19.4886786012718,-8.37593856288069));
#30628=CARTESIAN_POINT('Ctrl Pts',(81.7525656259724,-13.1230125396625,-16.6658777841638));
#30629=CARTESIAN_POINT('Ctrl Pts',(81.871420489716,-3.57127416847624,-20.9095896957926));
#30630=CARTESIAN_POINT('Ctrl Pts',(81.9902753534598,6.8475164670966,-20.07676414828));
#30631=CARTESIAN_POINT('Ctrl Pts',(82.1091302172036,15.6038319248663,-14.3695988007092));
#30632=CARTESIAN_POINT('Ctrl Pts',(82.2279850809473,20.5717690153327,-5.17370853572354));
#30633=CARTESIAN_POINT('Ctrl Pts',(82.346839944691,20.5451864845865,5.27828123032336));
#30634=CARTESIAN_POINT('Ctrl Pts',(82.4656948084347,15.5305381758191,14.4487828000231));
#30635=CARTESIAN_POINT('Ctrl Pts',(82.5845496721784,6.74530613216218,20.1113347547157));
#30636=CARTESIAN_POINT('Ctrl Pts',(82.7034045359223,-3.67758593981133,20.8911536801614));
#30637=CARTESIAN_POINT('Ctrl Pts',(82.8222593996659,-13.2076148301405,16.5989111369232));
#30638=CARTESIAN_POINT('Ctrl Pts',(82.9411142634097,-19.5310312327739,8.27669979020799));
#30639=CARTESIAN_POINT('Ctrl Pts',(83.0599691271534,-21.1126036723579,-2.05497119365699));
#30640=CARTESIAN_POINT('Ctrl Pts',(83.1788239908972,-17.5683498780442,-11.887725728475));
#30641=CARTESIAN_POINT('Ctrl Pts',(83.2976788546409,-9.75876196915726,-18.8343172231475));
#30642=CARTESIAN_POINT('Ctrl Pts',(83.4165337183847,0.420108236131625,-21.2082165563905));
#30643=CARTESIAN_POINT('Ctrl Pts',(83.5353885821283,10.4969824085646,-18.4330762692261));
#30644=CARTESIAN_POINT('Ctrl Pts',(83.6542434458721,18.0253453390124,-11.1826591579179));
#30645=CARTESIAN_POINT('Ctrl Pts',(83.7730983096158,21.1774224523421,-1.21725868567815));
#30646=CARTESIAN_POINT('Ctrl Pts',(83.8919531733597,19.1879362958286,9.04367409519178));
#30647=CARTESIAN_POINT('Ctrl Pts',(84.0108080371033,12.5399045252426,17.1089372823276));
#30648=CARTESIAN_POINT('Ctrl Pts',(84.1296629008471,2.84737040034882,21.02040490181));
#30649=CARTESIAN_POINT('Ctrl Pts',(84.2485177645907,-7.5364629182508,19.8284307779171));
#30650=CARTESIAN_POINT('Ctrl Pts',(84.3673726283346,-16.0905551051233,13.8224085036513));
#30651=CARTESIAN_POINT('Ctrl Pts',(84.4862274920782,-20.7380997739461,4.46051097954932));
#30652=CARTESIAN_POINT('Ctrl Pts',(84.605082355822,-20.3507421866508,-5.98433228399736));
#30653=CARTESIAN_POINT('Ctrl Pts',(84.7239372195658,-15.0225270055477,-14.9762686541211));
#30654=CARTESIAN_POINT('Ctrl Pts',(84.8427920833094,-6.04706564773123,-20.3321896874107));
#30655=CARTESIAN_POINT('Ctrl Pts',(84.9616469470532,4.39653333139736,-20.7517573978382));
#30656=CARTESIAN_POINT('Ctrl Pts',(85.0805018107969,13.7727193927253,-16.1331069841513));
#30657=CARTESIAN_POINT('Ctrl Pts',(85.1993566745408,19.8050939814884,-7.59757808891962));
#30658=CARTESIAN_POINT('Ctrl Pts',(85.3182115382844,21.0290862470408,2.78252979271425));
#30659=CARTESIAN_POINT('Ctrl Pts',(85.4370664020282,17.1475290676846,12.4870808160166));
#30660=CARTESIAN_POINT('Ctrl Pts',(85.5559212657719,9.102806809038,19.1599542961395));
#30661=CARTESIAN_POINT('Ctrl Pts',(85.6747761295157,-1.15194158697989,21.1810757756306));
#30662=CARTESIAN_POINT('Ctrl Pts',(85.7936309932593,-11.1270156946867,18.0597470127081));
#30663=CARTESIAN_POINT('Ctrl Pts',(85.9124858570031,-18.4006158469338,10.5537802178361));
#30664=CARTESIAN_POINT('Ctrl Pts',(86.0313407207469,-21.2068200828936,0.485512517453323));
#30665=CARTESIAN_POINT('Ctrl Pts',(86.1501955844905,-18.8643237414458,-9.70063040274928));
#30666=CARTESIAN_POINT('Ctrl Pts',(86.2690504482344,-11.9418501021132,-17.5316045064757));
#30667=CARTESIAN_POINT('Ctrl Pts',(86.387905311978,-2.12007282952809,-21.1061657254537));
#30668=CARTESIAN_POINT('Ctrl Pts',(86.5067601757219,8.21642660125285,-19.5564637483121));
#30669=CARTESIAN_POINT('Ctrl Pts',(86.6256150394655,16.558099828919,-13.2587431715217));
#30670=CARTESIAN_POINT('Ctrl Pts',(86.7444699032093,20.8797126318402,-3.74199690601068));
#30671=CARTESIAN_POINT('Ctrl Pts',(86.863324766953,20.1320416824852,6.68325056596715));
#30672=CARTESIAN_POINT('Ctrl Pts',(86.9821796306968,14.4966103697264,15.485904178354));
#30673=CARTESIAN_POINT('Ctrl Pts',(87.1010344944404,5.34161761921727,20.5288105267424));
#30674=CARTESIAN_POINT('Ctrl Pts',(87.2198893581843,-5.11024046107027,20.5876269361687));
#30675=CARTESIAN_POINT('Ctrl Pts',(87.3387442219279,-14.3214081450722,15.6480736570059));
#30676=CARTESIAN_POINT('Ctrl Pts',(87.4575990856717,-20.0555508862681,6.90940077583666));
#30677=CARTESIAN_POINT('Ctrl Pts',(87.5764539494153,-20.9205040919877,-3.50677187309764));
#30678=CARTESIAN_POINT('Ctrl Pts',(87.6953088131592,-16.7062699854633,-13.0715524558344));
#30679=CARTESIAN_POINT('Ctrl Pts',(87.8141636769028,-8.43600194342856,-19.4627544721524));
#30680=CARTESIAN_POINT('Ctrl Pts',(87.9330185406467,1.88240192978519,-21.1286891076461));
#30681=CARTESIAN_POINT('Ctrl Pts',(88.0518734043902,11.7437866051695,-17.6648922047393));
#30682=CARTESIAN_POINT('Ctrl Pts',(88.1707282681343,18.7539545192176,-9.91232214589198));
#30683=CARTESIAN_POINT('Ctrl Pts',(88.2895831318777,21.2109411413823,0.24681233687776));
#30684=CARTESIAN_POINT('Ctrl Pts',(88.4084379956217,18.5182266544175,10.3460244542741));
#30685=CARTESIAN_POINT('Ctrl Pts',(88.5272928593653,11.3295620959432,17.9333756762919));
#30686=CARTESIAN_POINT('Ctrl Pts',(88.6461477231091,1.39024832758623,21.1667699477362));
#30687=CARTESIAN_POINT('Ctrl Pts',(88.7650025868527,-8.88659706215682,19.261187219064));
#30688=CARTESIAN_POINT('Ctrl Pts',(88.8838574505966,-17.0059088260971,12.6792746413611));
#30689=CARTESIAN_POINT('Ctrl Pts',(89.0027123143402,-20.9964387995634,3.01902271757524));
#30690=CARTESIAN_POINT('Ctrl Pts',(89.1215671780841,-19.889345642897,-7.37420303018019));
#30691=CARTESIAN_POINT('Ctrl Pts',(89.2404220418276,-13.9534151124538,-15.9770819341667));
#30692=CARTESIAN_POINT('Ctrl Pts',(89.3592769055716,-4.62980287552805,-20.7009629189214));
#30693=CARTESIAN_POINT('Ctrl Pts',(89.4781317693152,5.81785665575857,-20.3989579233126));
#30694=CARTESIAN_POINT('Ctrl Pts',(89.5969866330589,14.8530271009356,-15.144389270837));
#30695=CARTESIAN_POINT('Ctrl Pts',(89.7158414968027,20.2821034254025,-6.21298809401871));
#30696=CARTESIAN_POINT('Ctrl Pts',(89.8346963605464,20.7869866274943,4.22683420357247));
#30697=CARTESIAN_POINT('Ctrl Pts',(89.9535512242901,16.2450985707107,13.6404440146805));
#30698=CARTESIAN_POINT('Ctrl Pts',(90.072406088034,7.7591421436847,19.7423568354331));
#30699=CARTESIAN_POINT('Ctrl Pts',(90.1912609517776,-2.61061862620169,21.051119004094));
#30700=CARTESIAN_POINT('Ctrl Pts',(90.3101158155214,-12.3465600002041,17.2489824530325));
#30701=CARTESIAN_POINT('Ctrl Pts',(90.428970679265,-19.0849402202106,9.25904954565997));
#30702=CARTESIAN_POINT('Ctrl Pts',(90.5478255430088,-21.1897806934203,-0.978843101674954));
#30703=CARTESIAN_POINT('Ctrl Pts',(90.6666804067526,-18.1500575946877,-10.9790868266686));
#30704=CARTESIAN_POINT('Ctrl Pts',(90.7855352704963,-10.7037702107086,-18.3137722576163));
#30705=CARTESIAN_POINT('Ctrl Pts',(90.9043901342401,-0.658766948608187,
-21.2021446656999));
#30706=CARTESIAN_POINT('Ctrl Pts',(91.0232449979838,9.54617585506875,-18.9429544462565));
#30707=CARTESIAN_POINT('Ctrl Pts',(91.1420998617275,17.4334476903006,-12.084691003795));
#30708=CARTESIAN_POINT('Ctrl Pts',(91.2609547254713,21.0881404464175,-2.29245520892303));
#30709=CARTESIAN_POINT('Ctrl Pts',(91.379809589215,19.6229407913781,8.0563761033425));
#30710=CARTESIAN_POINT('Ctrl Pts',(91.4986644529587,13.3935936805263,16.4491968686648));
#30711=CARTESIAN_POINT('Ctrl Pts',(91.6175193167025,3.9124599895233,20.8484802306535));
#30712=CARTESIAN_POINT('Ctrl Pts',(91.7363741804461,-6.51851915066736,20.1858994392144));
#30713=CARTESIAN_POINT('Ctrl Pts',(91.8552290441899,-15.3669806594123,14.6228032260118));
#30714=CARTESIAN_POINT('Ctrl Pts',(91.9740839079338,-20.4844067906062,5.50887640297662));
#30715=CARTESIAN_POINT('Ctrl Pts',(92.0929387716773,-20.6288400258807,-4.94127331311132));
#30716=CARTESIAN_POINT('Ctrl Pts',(92.2117936354212,-15.7642748668298,-14.1943159588457));
#30717=CARTESIAN_POINT('Ctrl Pts',(92.2910302112503,-9.97048019729925,-18.0613752227927));
#30718=CARTESIAN_POINT('Ctrl Pts',(92.3306484991649,-6.78625091085736,-19.1875718595368));
#30719=CARTESIAN_POINT('Ctrl Pts',(68.725,11.6491905967231,-16.3382590211968));
#30720=CARTESIAN_POINT('Ctrl Pts',(68.7646182879146,14.3605687349063,-14.4050444314105));
#30721=CARTESIAN_POINT('Ctrl Pts',(68.8438548637438,18.799624465765,-9.16469984651376));
#30722=CARTESIAN_POINT('Ctrl Pts',(68.9627097274874,20.8933712948219,0.927153582356417));
#30723=CARTESIAN_POINT('Ctrl Pts',(69.0815645912312,17.9146243999094,10.7913118927399));
#30724=CARTESIAN_POINT('Ctrl Pts',(69.200419454975,10.5864329691218,18.0367711701248));
#30725=CARTESIAN_POINT('Ctrl Pts',(69.3192743187187,0.688032188973571,20.9025284426369));
#30726=CARTESIAN_POINT('Ctrl Pts',(69.4381291824624,-9.37742221120445,18.6937889137184));
#30727=CARTESIAN_POINT('Ctrl Pts',(69.5569840462062,-17.1661730459504,11.9463094506391));
#30728=CARTESIAN_POINT('Ctrl Pts',(69.6758389099499,-20.7872348084396,2.29852811379418));
#30729=CARTESIAN_POINT('Ctrl Pts',(69.7946937736936,-19.3614637935703,-7.90734461841775));
#30730=CARTESIAN_POINT('Ctrl Pts',(69.9135486374375,-13.2350179122529,-16.1934098084835));
#30731=CARTESIAN_POINT('Ctrl Pts',(70.032403501181,-3.89530615487391,-20.5479670028002));
#30732=CARTESIAN_POINT('Ctrl Pts',(70.1512583649248,6.39012784832653,-19.9137776962236));
#30733=CARTESIAN_POINT('Ctrl Pts',(70.2701132286686,15.124133913895,-14.4448221531172));
#30734=CARTESIAN_POINT('Ctrl Pts',(70.3889680924123,20.1862251131474,-5.46887711782098));
#30735=CARTESIAN_POINT('Ctrl Pts',(70.5078229561561,20.3474010396572,4.83482921676092));
#30736=CARTESIAN_POINT('Ctrl Pts',(70.6266778198998,15.5685305420084,13.9647112886144));
#30737=CARTESIAN_POINT('Ctrl Pts',(70.7455326836435,7.00985233357066,19.7041689177776));
#30738=CARTESIAN_POINT('Ctrl Pts',(70.8643875473874,-3.25071379005506,20.6597474264871));
#30739=CARTESIAN_POINT('Ctrl Pts',(70.9832424111308,-12.7220549410739,16.599446414106));
#30740=CARTESIAN_POINT('Ctrl Pts',(71.1020972748749,-19.1046703260878,8.50904666627266));
#30741=CARTESIAN_POINT('Ctrl Pts',(71.2209521386184,-20.8489558359632,-1.64722309819828));
#30742=CARTESIAN_POINT('Ctrl Pts',(71.3398070023622,-17.5314248864508,-11.4035715815495));
#30743=CARTESIAN_POINT('Ctrl Pts',(71.458661866106,-9.95752466116282,-18.3913024557491));
#30744=CARTESIAN_POINT('Ctrl Pts',(71.5775167298497,0.0339144865576418,
-20.9138985648547));
#30745=CARTESIAN_POINT('Ctrl Pts',(71.6963715935934,10.017119701265,-18.3589110863466));
#30746=CARTESIAN_POINT('Ctrl Pts',(71.8152264573371,17.5683172038997,-11.3466529868452));
#30747=CARTESIAN_POINT('Ctrl Pts',(71.9340813210809,20.8541885247641,-1.57959626350904));
#30748=CARTESIAN_POINT('Ctrl Pts',(72.0529361848246,19.0769729670116,8.57096294462323));
#30749=CARTESIAN_POINT('Ctrl Pts',(72.1717910485684,12.6681520414353,16.640619797256));
#30750=CARTESIAN_POINT('Ctrl Pts',(72.2906459123121,3.18369217161882,20.670181603907));
#30751=CARTESIAN_POINT('Ctrl Pts',(72.4095007760559,-7.07372081696884,19.6813306761887));
#30752=CARTESIAN_POINT('Ctrl Pts',(72.5283556397995,-15.6137395751919,13.9141453154726));
#30753=CARTESIAN_POINT('Ctrl Pts',(72.6472105035434,-20.362974535936,4.76881237110371));
#30754=CARTESIAN_POINT('Ctrl Pts',(72.766065367287,-20.1683820703571,-5.5343173062329));
#30755=CARTESIAN_POINT('Ctrl Pts',(72.8849202310308,-15.0772063355693,-14.4937970351682));
#30756=CARTESIAN_POINT('Ctrl Pts',(73.0037750947745,-6.32550909580307,-19.9343983621499));
#30757=CARTESIAN_POINT('Ctrl Pts',(73.1226299585183,3.96192769410095,-20.5352241850118));
#30758=CARTESIAN_POINT('Ctrl Pts',(73.241484822262,13.2874673524912,-16.1504029280528));
#30759=CARTESIAN_POINT('Ctrl Pts',(73.3603396860058,19.3870075181409,-7.84450399155505));
#30760=CARTESIAN_POINT('Ctrl Pts',(73.4791945497494,20.7796705370668,2.36592386879463));
#30761=CARTESIAN_POINT('Ctrl Pts',(73.5980494134933,17.1273385367331,12.0019405943419));
#30762=CARTESIAN_POINT('Ctrl Pts',(73.7169042772369,9.31674341779712,18.7240646086503));
#30763=CARTESIAN_POINT('Ctrl Pts',(73.8357591409808,-0.75581846594697,20.9002641569074));
#30764=CARTESIAN_POINT('Ctrl Pts',(73.9546140047244,-10.6448788649411,18.0021903481967));
#30765=CARTESIAN_POINT('Ctrl Pts',(74.0734688684682,-17.9495209615153,10.7334524098305));
#30766=CARTESIAN_POINT('Ctrl Pts',(74.1923237322118,-20.8962862723432,0.858791829406043));
#30767=CARTESIAN_POINT('Ctrl Pts',(74.3111785959557,-18.7697439974256,-9.22437063723492));
#30768=CARTESIAN_POINT('Ctrl Pts',(74.4300334596993,-12.0861869801001,-17.0679930766342));
#30769=CARTESIAN_POINT('Ctrl Pts',(74.5488883234432,-2.46828348179083,-20.7677605926949));
#30770=CARTESIAN_POINT('Ctrl Pts',(74.6677431871868,7.74888254330118,-19.4254246468925));
#30771=CARTESIAN_POINT('Ctrl Pts',(74.7865980509306,16.0847351103166,-13.3668844467559));
#30772=CARTESIAN_POINT('Ctrl Pts',(74.9054529146743,20.5154531674799,-4.06306346429831));
#30773=CARTESIAN_POINT('Ctrl Pts',(75.024307778418,19.9653242538903,6.22720891081994));
#30774=CARTESIAN_POINT('Ctrl Pts',(75.1431626421618,14.5679114895243,15.0056075590215));
#30775=CARTESIAN_POINT('Ctrl Pts',(75.2620175059054,5.63362643574612,20.1408678205393));
#30776=CARTESIAN_POINT('Ctrl Pts',(75.3808723696493,-4.66841934638479,20.3862248635758));
#30777=CARTESIAN_POINT('Ctrl Pts',(75.499727233393,-13.8370423291352,15.6821096464633));
#30778=CARTESIAN_POINT('Ctrl Pts',(75.6185820971368,-19.6462371868223,7.17061139520864));
#30779=CARTESIAN_POINT('Ctrl Pts',(75.7374369608804,-20.6856177888931,-3.08180467807508));
#30780=CARTESIAN_POINT('Ctrl Pts',(75.8562918246243,-16.7028379804262,-12.5860044009848));
#30781=CARTESIAN_POINT('Ctrl Pts',(75.9751466883679,-8.66485747623899,-19.0345094052471));
#30782=CARTESIAN_POINT('Ctrl Pts',(76.0940015521117,1.47682157948402,-20.8617185630606));
#30783=CARTESIAN_POINT('Ctrl Pts',(76.2128564158554,11.2599503155789,-17.6240126609314));
#30784=CARTESIAN_POINT('Ctrl Pts',(76.3317112795992,18.3093305469575,-10.1074585482319));
#30785=CARTESIAN_POINT('Ctrl Pts',(76.4505661433428,20.9134775754992,-0.136963794739155));
#30786=CARTESIAN_POINT('Ctrl Pts',(76.5694210070867,18.4401432255183,9.86678373150789));
#30787=CARTESIAN_POINT('Ctrl Pts',(76.6882758708303,11.4898162994893,17.4750228837036));
#30788=CARTESIAN_POINT('Ctrl Pts',(76.8071307345741,1.74993282588505,20.8405863278091));
#30789=CARTESIAN_POINT('Ctrl Pts',(76.9259855983178,-8.41480831689548,19.1463653044614));
#30790=CARTESIAN_POINT('Ctrl Pts',(77.0448404620616,-16.5365591258767,12.8036914855974));
#30791=CARTESIAN_POINT('Ctrl Pts',(77.1636953258053,-20.6434792725082,3.35247176088037));
#30792=CARTESIAN_POINT('Ctrl Pts',(77.2825501895491,-19.7384696137938,-6.91267825718176));
#30793=CARTESIAN_POINT('Ctrl Pts',(77.4014050532927,-14.0412530376615,-15.4995327837435));
#30794=CARTESIAN_POINT('Ctrl Pts',(77.5202599170366,-4.93502901298443,-20.323331223571));
#30795=CARTESIAN_POINT('Ctrl Pts',(77.6391147807802,5.3693466737219,-20.2129270438343));
#30796=CARTESIAN_POINT('Ctrl Pts',(77.7579696445241,14.3701248285384,-15.1951247376979));
#30797=CARTESIAN_POINT('Ctrl Pts',(77.8768245082677,19.8820503542049,-6.48817209195593));
#30798=CARTESIAN_POINT('Ctrl Pts',(77.9956793720115,20.566909693682,3.79401226064252));
#30799=CARTESIAN_POINT('Ctrl Pts',(78.1145342357552,16.2584291829867,13.1550668521213));
#30800=CARTESIAN_POINT('Ctrl Pts',(78.2333890994989,8.002643824371,19.3222668235958));
#30801=CARTESIAN_POINT('Ctrl Pts',(78.3522439632428,-2.19606445801497,20.7983077263084));
#30802=CARTESIAN_POINT('Ctrl Pts',(78.4710988269864,-11.8616009447801,17.2248287773426));
#30803=CARTESIAN_POINT('Ctrl Pts',(78.5899536907302,-18.6473171004135,9.46941752900355));
#30804=CARTESIAN_POINT('Ctrl Pts',(78.7088085544739,-20.9057419437845,-0.585027488128542));
#30805=CARTESIAN_POINT('Ctrl Pts',(78.8276634182176,-18.0885635049867,-10.4974365303172));
#30806=CARTESIAN_POINT('Ctrl Pts',(78.9465182819614,-10.8797508184065,-17.8612240765116));
#30807=CARTESIAN_POINT('Ctrl Pts',(79.0653731457051,-1.02949641157685,-20.8885720076918));
#30808=CARTESIAN_POINT('Ctrl Pts',(79.1842280094488,9.07070441569705,-18.8444852618751));
#30809=CARTESIAN_POINT('Ctrl Pts',(79.3030828731926,16.9686730893506,-12.2252377060213));
#30810=CARTESIAN_POINT('Ctrl Pts',(79.4219377369363,20.7469002557211,-2.63788422057037));
#30811=CARTESIAN_POINT('Ctrl Pts',(79.5407926006801,19.488088539859,7.58990832912952));
#30812=CARTESIAN_POINT('Ctrl Pts',(79.6596474644237,13.4978587082429,15.9749839960573));
#30813=CARTESIAN_POINT('Ctrl Pts',(79.7785023281676,4.23054949116273,20.4815710917107));
#30814=CARTESIAN_POINT('Ctrl Pts',(79.8973571919112,-6.06387423543652,20.0155372807922));
#30815=CARTESIAN_POINT('Ctrl Pts',(80.0162120556551,-14.8860794655671,14.6900286428174));
#30816=CARTESIAN_POINT('Ctrl Pts',(80.1350669193987,-20.0941659527598,5.79799948645444));
#30817=CARTESIAN_POINT('Ctrl Pts',(80.2539217831425,-20.4236877405258,-4.50169773079794));
#30818=CARTESIAN_POINT('Ctrl Pts',(80.3727766468861,-15.7946418386806,-13.7084496778365));
#30819=CARTESIAN_POINT('Ctrl Pts',(80.49163151063,-7.33089175974107,-19.586993883415));
#30820=CARTESIAN_POINT('Ctrl Pts',(80.6104863743736,2.91268983041759,-20.7101072265152));
#30821=CARTESIAN_POINT('Ctrl Pts',(80.7293412381174,12.4491136405291,-16.8051144877733));
#30822=CARTESIAN_POINT('Ctrl Pts',(80.8481961018612,18.9630777731095,-8.82008983814658));
#30823=CARTESIAN_POINT('Ctrl Pts',(80.9670509656049,20.8730885973582,1.30632147223087));
#30824=CARTESIAN_POINT('Ctrl Pts',(81.0859058293486,17.7154238864056,11.1155773537385));
#30825=CARTESIAN_POINT('Ctrl Pts',(81.2047606930925,10.2567176785937,18.2261363388843));
#30826=CARTESIAN_POINT('Ctrl Pts',(81.323615556836,0.307832932572739,20.9116604378418));
#30827=CARTESIAN_POINT('Ctrl Pts',(81.44247042058,-9.71578907209836,18.5201443322797));
#30828=CARTESIAN_POINT('Ctrl Pts',(81.5613252843235,-17.3805619607799,11.6322125715389));
#30829=CARTESIAN_POINT('Ctrl Pts',(81.6801801480674,-20.8255928488529,1.92015256575688));
#30830=CARTESIAN_POINT('Ctrl Pts',(81.799035011811,-19.214479463215,-8.25809193092852));
#30831=CARTESIAN_POINT('Ctrl Pts',(81.9178898755548,-12.9383761771515,-16.4313945020042));
#30832=CARTESIAN_POINT('Ctrl Pts',(82.0367447392985,-3.52102754484433,-20.6153988176417));
#30833=CARTESIAN_POINT('Ctrl Pts',(82.1555996030423,6.75117421878302,-19.7942908448273));
#30834=CARTESIAN_POINT('Ctrl Pts',(82.274454466786,15.3842912699189,-14.1674233897442));
#30835=CARTESIAN_POINT('Ctrl Pts',(82.3933093305298,20.2823311602726,-5.10091620074396));
#30836=CARTESIAN_POINT('Ctrl Pts',(82.5121641942734,20.2561226367727,5.20401759278348));
#30837=CARTESIAN_POINT('Ctrl Pts',(82.6310190580173,15.3120287392127,14.2454932968817));
#30838=CARTESIAN_POINT('Ctrl Pts',(82.7498739217609,6.65040194880476,19.8283750544846));
#30839=CARTESIAN_POINT('Ctrl Pts',(82.8687287855047,-3.62584354539574,20.5972221905355));
#30840=CARTESIAN_POINT('Ctrl Pts',(82.9875836492484,-13.0217881419229,16.3653700529151));
#30841=CARTESIAN_POINT('Ctrl Pts',(83.1064385129922,-19.2562362074694,8.16024941433271));
#30842=CARTESIAN_POINT('Ctrl Pts',(83.2252933767359,-20.8155564559951,-2.02605844171725));
#30843=CARTESIAN_POINT('Ctrl Pts',(83.3441482404796,-17.3211691177578,-11.7204694349677));
#30844=CARTESIAN_POINT('Ctrl Pts',(83.4630031042234,-9.62145947804478,-18.5693247290879));
#30845=CARTESIAN_POINT('Ctrl Pts',(83.581857967967,0.41419745487271,-20.9098240989816));
#30846=CARTESIAN_POINT('Ctrl Pts',(83.7007128317109,10.3492934047325,-18.1737291001251));
#30847=CARTESIAN_POINT('Ctrl Pts',(83.8195676954545,17.7717348066487,-11.025322913372));
#30848=CARTESIAN_POINT('Ctrl Pts',(83.9384225591984,20.8794632575961,-1.20013226632287));
#30849=CARTESIAN_POINT('Ctrl Pts',(84.057277422942,18.9179685006256,8.91643264940149));
#30850=CARTESIAN_POINT('Ctrl Pts',(84.1761322866858,12.3634722959219,16.8682203023895));
#30851=CARTESIAN_POINT('Ctrl Pts',(84.2949871504295,2.80730885869799,20.7246548910676));
#30852=CARTESIAN_POINT('Ctrl Pts',(84.4138420141732,-7.43042742562143,19.5494514412693));
#30853=CARTESIAN_POINT('Ctrl Pts',(84.532696877917,-15.8641664191098,13.6279318757016));
#30854=CARTESIAN_POINT('Ctrl Pts',(84.6515517416607,-20.4463217011843,4.39775309375782));
#30855=CARTESIAN_POINT('Ctrl Pts',(84.7704066054045,-20.0644141045594,-5.90013474615043));
#30856=CARTESIAN_POINT('Ctrl Pts',(84.8892614691482,-14.8111651148504,-14.7655576028342));
#30857=CARTESIAN_POINT('Ctrl Pts',(85.0081163328919,-5.96198547260468,-20.0461226327294));
#30858=CARTESIAN_POINT('Ctrl Pts',(85.1269711966356,4.33467558954779,-20.4597871669124));
#30859=CARTESIAN_POINT('Ctrl Pts',(85.2458260603795,13.5789418738155,-15.9061196075446));
#30860=CARTESIAN_POINT('Ctrl Pts',(85.364680924123,19.5264429856993,-7.49068272644153));
#30861=CARTESIAN_POINT('Ctrl Pts',(85.483535787867,20.7332140926975,2.74338053655433));
#30862=CARTESIAN_POINT('Ctrl Pts',(85.6023906516105,16.9062691143363,12.3113917984773));
#30863=CARTESIAN_POINT('Ctrl Pts',(85.7212455153543,8.97473338589818,18.890380198239));
#30864=CARTESIAN_POINT('Ctrl Pts',(85.8401003790982,-1.13573415718418,20.8830651798576));
#30865=CARTESIAN_POINT('Ctrl Pts',(85.9589552428418,-10.9704623349105,17.8056524603926));
#30866=CARTESIAN_POINT('Ctrl Pts',(86.0778101065857,-18.1417253850317,10.4052920879747));
#30867=CARTESIAN_POINT('Ctrl Pts',(86.1966649703292,-20.908447273396,0.478681520004721));
#30868=CARTESIAN_POINT('Ctrl Pts',(86.3155198340731,-18.5989090657894,-9.56414580317936));
#30869=CARTESIAN_POINT('Ctrl Pts',(86.4343746978168,-11.7738322969147,-17.28494074118));
#30870=CARTESIAN_POINT('Ctrl Pts',(86.5532295615605,-2.09024411951815,-20.8092090888336));
#30871=CARTESIAN_POINT('Ctrl Pts',(86.6720844253043,8.10082424882741,-19.2813108960876));
#30872=CARTESIAN_POINT('Ctrl Pts',(86.7909392890479,16.3251329462566,-13.0721971247768));
#30873=CARTESIAN_POINT('Ctrl Pts',(86.9097941527918,20.5859421139072,-3.68934827101431));
#30874=CARTESIAN_POINT('Ctrl Pts',(87.0286490165353,19.8487906427609,6.58921948350647));
#30875=CARTESIAN_POINT('Ctrl Pts',(87.1475038802793,14.2926479488024,15.2680227270453));
#30876=CARTESIAN_POINT('Ctrl Pts',(87.2663587440228,5.26646286003707,20.2399770831349));
#30877=CARTESIAN_POINT('Ctrl Pts',(87.3852136077667,-5.03834110050527,20.2979659655083));
#30878=CARTESIAN_POINT('Ctrl Pts',(87.5040684715104,-14.1199107603864,15.4279105358017));
#30879=CARTESIAN_POINT('Ctrl Pts',(87.6229233352541,-19.7733760462607,6.81218783616099));
#30880=CARTESIAN_POINT('Ctrl Pts',(87.7417781989979,-20.6261596519617,-3.45743277501727));
#30881=CARTESIAN_POINT('Ctrl Pts',(87.8606330627416,-16.4712183986482,-12.887640119355));
#30882=CARTESIAN_POINT('Ctrl Pts',(87.9794879264853,-8.3173102399601,-19.1889200778529));
#30883=CARTESIAN_POINT('Ctrl Pts',(88.0983427902292,1.85591716921299,-20.8314155746315));
#30884=CARTESIAN_POINT('Ctrl Pts',(88.2171976539728,11.5785554866035,-17.4163531264618));
#30885=CARTESIAN_POINT('Ctrl Pts',(88.3360525177166,18.4900927013111,-9.77285911485978));
#30886=CARTESIAN_POINT('Ctrl Pts',(88.4549073814602,20.9125103499811,0.243339770501251));
#30887=CARTESIAN_POINT('Ctrl Pts',(88.5737622452041,18.2576814481021,10.2004593779692));
#30888=CARTESIAN_POINT('Ctrl Pts',(88.6926171089477,11.170158976582,17.6810591260786));
#30889=CARTESIAN_POINT('Ctrl Pts',(88.8114719726915,1.37068800228615,20.868960630139));
#30890=CARTESIAN_POINT('Ctrl Pts',(88.9303268364353,-8.76156563726881,18.9901888080648));
#30891=CARTESIAN_POINT('Ctrl Pts',(89.049181700179,-16.766641421806,12.5008815214899));
#30892=CARTESIAN_POINT('Ctrl Pts',(89.1680365639226,-20.7010259838003,2.97654608568703));
#30893=CARTESIAN_POINT('Ctrl Pts',(89.2868914276665,-19.6095092546341,-7.27045047947625));
#30894=CARTESIAN_POINT('Ctrl Pts',(89.4057462914101,-13.7570952656821,-15.7522897774154));
#30895=CARTESIAN_POINT('Ctrl Pts',(89.524601155154,-4.56466310983042,-20.4097073491906));
#30896=CARTESIAN_POINT('Ctrl Pts',(89.6434560188976,5.73600137388006,-20.1119514620605));
#30897=CARTESIAN_POINT('Ctrl Pts',(89.7623108826413,14.6440500167558,-14.9313128191482));
#30898=CARTESIAN_POINT('Ctrl Pts',(89.8811657463853,19.996741067543,-6.12557344600731));
#30899=CARTESIAN_POINT('Ctrl Pts',(90.0000206101288,20.4945207331834,4.16736407124383));
#30900=CARTESIAN_POINT('Ctrl Pts',(90.1188754738726,16.0165355102348,13.4485275657482));
#30901=CARTESIAN_POINT('Ctrl Pts',(90.2377303376165,7.64997362942123,19.4645885301395));
#30902=CARTESIAN_POINT('Ctrl Pts',(90.3565852013599,-2.57388810220134,20.7549368562865));
#30903=CARTESIAN_POINT('Ctrl Pts',(90.475440065104,-12.172848063172,17.0062950847534));
#30904=CARTESIAN_POINT('Ctrl Pts',(90.5942949288474,-18.8164215450704,9.12877783988716));
#30905=CARTESIAN_POINT('Ctrl Pts',(90.7131497925914,-20.8916476223885,-0.965071109213948));
#30906=CARTESIAN_POINT('Ctrl Pts',(90.8320046563349,-17.8946924029286,-10.8246147761969));
#30907=CARTESIAN_POINT('Ctrl Pts',(90.9508595200788,-10.5531717722109,-18.05610365574));
#30908=CARTESIAN_POINT('Ctrl Pts',(91.0697143838226,-0.649498319719339,
-20.9038376377461));
#30909=CARTESIAN_POINT('Ctrl Pts',(91.1885692475662,9.41186437891623,-18.6764334630907));
#30910=CARTESIAN_POINT('Ctrl Pts',(91.30742411131,17.1881649583186,-11.9146634752632));
#30911=CARTESIAN_POINT('Ctrl Pts',(91.4262789750537,20.7914374193968,-2.26020113694711));
#30912=CARTESIAN_POINT('Ctrl Pts',(91.5451338387974,19.3468526295679,7.94302560746775));
#30913=CARTESIAN_POINT('Ctrl Pts',(91.6639887025412,13.2051503325794,16.2177622139406));
#30914=CARTESIAN_POINT('Ctrl Pts',(91.7828435662849,3.85741299640702,20.5551491420764));
#30915=CARTESIAN_POINT('Ctrl Pts',(91.9016984300287,-6.42680578368705,19.901890639009));
#30916=CARTESIAN_POINT('Ctrl Pts',(92.0205532937724,-15.1507724219245,14.417065314141));
#30917=CARTESIAN_POINT('Ctrl Pts',(92.1394081575162,-20.1961980925971,5.43136836909382));
#30918=CARTESIAN_POINT('Ctrl Pts',(92.2582630212598,-20.3385992009415,-4.87175126335728));
#30919=CARTESIAN_POINT('Ctrl Pts',(92.3771178850036,-15.5424768337762,-13.9946067183758));
#30920=CARTESIAN_POINT('Ctrl Pts',(92.4563544608328,-9.83019890208951,-17.8072577621103));
#30921=CARTESIAN_POINT('Ctrl Pts',(92.4959727487473,-6.69077064826668,-18.9176091918295));
#30922=CARTESIAN_POINT('',(92.,-6.97721143603873,-19.7274971949513));
#30923=CARTESIAN_POINT('Ctrl Pts',(92.,-13.2939520371397,15.0312716283101));
#30924=CARTESIAN_POINT('Ctrl Pts',(92.,-13.6160698917503,14.758567432308));
#30925=CARTESIAN_POINT('Ctrl Pts',(92.,-13.9291994758583,14.475971697715));
#30926=CARTESIAN_POINT('Ctrl Pts',(92.,-14.2328195904016,14.183841939621));
#30927=CARTESIAN_POINT('Ctrl Pts',(92.,-14.3443295390009,14.0765520311168));
#30928=CARTESIAN_POINT('Ctrl Pts',(92.,-14.4545565403831,13.9679756804271));
#30929=CARTESIAN_POINT('Ctrl Pts',(92.,-14.5634738142937,13.8581291163106));
#30930=CARTESIAN_POINT('Ctrl Pts',(92.,-14.858732771742,13.5603509876831));
#30931=CARTESIAN_POINT('Ctrl Pts',(92.,-15.1443694959895,13.2532412422133));
#30932=CARTESIAN_POINT('Ctrl Pts',(92.,-15.4201237116956,12.9373782285482));
#30933=CARTESIAN_POINT('Ctrl Pts',(92.,-15.697033728144,12.6201913014671));
#30934=CARTESIAN_POINT('Ctrl Pts',(92.,-15.9639785353498,12.294177135262));
#30935=CARTESIAN_POINT('Ctrl Pts',(92.,-16.2206559670913,11.9598852286998));
#30936=CARTESIAN_POINT('Ctrl Pts',(92.,-16.4160308888044,11.7054325694582));
#30937=CARTESIAN_POINT('Ctrl Pts',(92.,-16.6054563648391,11.4461831784212));
#30938=CARTESIAN_POINT('Ctrl Pts',(92.,-16.788782522303,11.1823678395403));
#30939=CARTESIAN_POINT('Ctrl Pts',(92.,-16.8144368585662,11.1454499904528));
#30940=CARTESIAN_POINT('Ctrl Pts',(92.,-16.8399694108848,11.108446018421));
#30941=CARTESIAN_POINT('Ctrl Pts',(92.,-16.8653752109956,11.071363398425));
#30942=CARTESIAN_POINT('Ctrl Pts',(92.,-17.1037405056281,10.723442466885));
#30943=CARTESIAN_POINT('Ctrl Pts',(92.,-17.3310748449526,10.3684236388796));
#30944=CARTESIAN_POINT('Ctrl Pts',(92.,-17.5471276373729,10.0068939956817));
#30945=CARTESIAN_POINT('Ctrl Pts',(92.,-17.7684746335703,9.63650535287952));
#30946=CARTESIAN_POINT('Ctrl Pts',(92.,-17.9779808926936,9.2592825348923));
#30947=CARTESIAN_POINT('Ctrl Pts',(92.,-18.1753337935665,8.87582095352862));
#30948=CARTESIAN_POINT('Ctrl Pts',(92.,-18.3685180548043,8.50045914237103));
#30949=CARTESIAN_POINT('Ctrl Pts',(92.,-18.5500570976423,8.11911876362687));
#30950=CARTESIAN_POINT('Ctrl Pts',(92.,-18.7196128001755,7.7323317844173));
#30951=CARTESIAN_POINT('Ctrl Pts',(92.,-18.8946566564853,7.33302534175734));
#30952=CARTESIAN_POINT('Ctrl Pts',(92.,-19.0569294873076,6.92791358991489));
#30953=CARTESIAN_POINT('Ctrl Pts',(92.,-19.2060045971,6.51756051797982));
#30954=CARTESIAN_POINT('Ctrl Pts',(92.,-19.2198478928059,6.47945463345951));
#30955=CARTESIAN_POINT('Ctrl Pts',(92.,-19.2335758890648,6.4413074867314));
#30956=CARTESIAN_POINT('Ctrl Pts',(92.,-19.2471856417164,6.40312712225039));
#30957=CARTESIAN_POINT('Ctrl Pts',(92.,-19.3801360300814,6.03015235807848));
#30958=CARTESIAN_POINT('Ctrl Pts',(92.,-19.5018839462995,5.65379323102824));
#30959=CARTESIAN_POINT('Ctrl Pts',(92.,-19.612223314782,5.27451367654917));
#30960=CARTESIAN_POINT('Ctrl Pts',(92.,-19.7305593453794,4.86774646751861));
#30961=CARTESIAN_POINT('Ctrl Pts',(92.,-19.8357743611108,4.45762013617097));
#30962=CARTESIAN_POINT('Ctrl Pts',(92.,-19.92796760317,4.0447862442832));
#30963=CARTESIAN_POINT('Ctrl Pts',(92.,-20.0201788060094,3.63187192547301));
#30964=CARTESIAN_POINT('Ctrl Pts',(92.,-20.0993631833585,3.21624845084337));
#30965=CARTESIAN_POINT('Ctrl Pts',(92.,-20.1655698219861,2.79854789811281));
#30966=CARTESIAN_POINT('Ctrl Pts',(92.,-20.2320538863996,2.37909705407441));
#30967=CARTESIAN_POINT('Ctrl Pts',(92.,-20.2854512878204,1.95755114980799));
#30968=CARTESIAN_POINT('Ctrl Pts',(92.,-20.325760397772,1.53453830704263));
#30969=CARTESIAN_POINT('Ctrl Pts',(92.,-20.3660288602495,1.11195202798934));
#30970=CARTESIAN_POINT('Ctrl Pts',(92.,-20.3932354432298,0.687901217036152));
#30971=CARTESIAN_POINT('Ctrl Pts',(92.,-20.4073267612968,0.263008398905277));
#30972=CARTESIAN_POINT('Ctrl Pts',(92.,-20.421342781554,-0.159613978774176));
#30973=CARTESIAN_POINT('Ctrl Pts',(92.,-20.4223833262527,-0.583069928986948));
#30974=CARTESIAN_POINT('Ctrl Pts',(92.,-20.4103444698736,-1.00674237530884));
#30975=CARTESIAN_POINT('Ctrl Pts',(92.,-20.408349887765,-1.076935876648));
#30976=CARTESIAN_POINT('Ctrl Pts',(92.,-20.4059961685756,-1.14713530012027));
#30977=CARTESIAN_POINT('Ctrl Pts',(92.,-20.4032827023909,-1.21733781136343));
#30978=CARTESIAN_POINT('Ctrl Pts',(92.,-20.4013287910156,-1.26788920060626));
#30979=CARTESIAN_POINT('Ctrl Pts',(92.,-20.3991881262455,-1.31844611013296));
#30980=CARTESIAN_POINT('Ctrl Pts',(92.,-20.3968618361394,-1.36898023731617));
#30981=CARTESIAN_POINT('Ctrl Pts',(92.,-20.377197273692,-1.79615460269462));
#30982=CARTESIAN_POINT('Ctrl Pts',(92.,-20.3442608580358,-2.22206346610525));
#30983=CARTESIAN_POINT('Ctrl Pts',(92.,-20.2981227972436,-2.64607409640738));
#30984=CARTESIAN_POINT('Ctrl Pts',(92.,-20.2518214654591,-3.07158519368148));
#30985=CARTESIAN_POINT('Ctrl Pts',(92.,-20.1922249321044,-3.4951851506192));
#30986=CARTESIAN_POINT('Ctrl Pts',(92.,-20.1193523275807,-3.91624204251575));
#30987=CARTESIAN_POINT('Ctrl Pts',(92.,-20.069345617195,-4.20518011720942));
#30988=CARTESIAN_POINT('Ctrl Pts',(92.,-20.013086138115,-4.4929208214171));
#30989=CARTESIAN_POINT('Ctrl Pts',(92.,-19.9505658664369,-4.77925995369804));
#30990=CARTESIAN_POINT('Ctrl Pts',(92.,-19.8594604469175,-5.19651736591093));
#30991=CARTESIAN_POINT('Ctrl Pts',(92.,-19.7550627546659,-5.61079923843387));
#30992=CARTESIAN_POINT('Ctrl Pts',(92.,-19.6377077496538,-6.02155968710754));
#30993=CARTESIAN_POINT('Ctrl Pts',(92.,-19.5203692827226,-6.43226224997153));
#30994=CARTESIAN_POINT('Ctrl Pts',(92.,-19.3900769227109,-6.83944488042613));
#30995=CARTESIAN_POINT('Ctrl Pts',(92.,-19.2471147713027,-7.24254753502617));
#30996=CARTESIAN_POINT('Ctrl Pts',(92.,-19.1398755268731,-7.54492423879746));
#30997=CARTESIAN_POINT('Ctrl Pts',(92.,-19.0255061208544,-7.84500495401166));
#30998=CARTESIAN_POINT('Ctrl Pts',(92.,-18.9041089056825,-8.14254540778852));
#30999=CARTESIAN_POINT('Ctrl Pts',(92.,-18.7978863424071,-8.40289330484327));
#31000=CARTESIAN_POINT('Ctrl Pts',(92.,-18.6862828670782,-8.6612962612323));
#31001=CARTESIAN_POINT('Ctrl Pts',(92.,-18.5693581238797,-8.91758517612054));
#31002=CARTESIAN_POINT('Ctrl Pts',(92.,-18.5532381230933,-8.95291882233212));
#31003=CARTESIAN_POINT('Ctrl Pts',(92.,-18.5370157670781,-8.9882148657338));
#31004=CARTESIAN_POINT('Ctrl Pts',(92.,-18.5206952618725,-9.02346409661682));
#31005=CARTESIAN_POINT('Ctrl Pts',(92.,-18.3411773006904,-9.41118923022199));
#31006=CARTESIAN_POINT('Ctrl Pts',(92.,-18.1499874366914,-9.79282687859415));
#31007=CARTESIAN_POINT('Ctrl Pts',(92.,-17.9475101887474,-10.1678622906306));
#31008=CARTESIAN_POINT('Ctrl Pts',(92.,-17.7429704910178,-10.5467178440062));
#31009=CARTESIAN_POINT('Ctrl Pts',(92.,-17.5269121246835,-10.9188364850125));
#31010=CARTESIAN_POINT('Ctrl Pts',(92.,-17.299679928222,-11.2836750922875));
#31011=CARTESIAN_POINT('Ctrl Pts',(92.,-17.0722860038054,-11.6487733661187));
#31012=CARTESIAN_POINT('Ctrl Pts',(92.,-16.8337020963105,-12.0065817412458));
#31013=CARTESIAN_POINT('Ctrl Pts',(92.,-16.58422560562,-12.3565359028326));
#31014=CARTESIAN_POINT('Ctrl Pts',(92.,-16.3362967632301,-12.7043190944734));
#31015=CARTESIAN_POINT('Ctrl Pts',(92.,-16.0776097838226,-13.044345683683));
#31016=CARTESIAN_POINT('Ctrl Pts',(92.,-15.8084129870003,-13.3760348394112));
#31017=CARTESIAN_POINT('Ctrl Pts',(92.,-15.6746083502117,-13.5409013888383));
#31018=CARTESIAN_POINT('Ctrl Pts',(92.,-15.5382065058082,-13.7037076289432));
#31019=CARTESIAN_POINT('Ctrl Pts',(92.,-15.3992342253977,-13.8643791870089));
#31020=CARTESIAN_POINT('Ctrl Pts',(92.,-15.1170023822946,-14.1906790061758));
#31021=CARTESIAN_POINT('Ctrl Pts',(92.,-14.8241712853989,-14.508177194315));
#31022=CARTESIAN_POINT('Ctrl Pts',(92.,-14.5212455312031,-14.8165114420203));
#31023=CARTESIAN_POINT('Ctrl Pts',(92.,-14.3887155137425,-14.9514076753914));
#31024=CARTESIAN_POINT('Ctrl Pts',(92.,-14.2542528654501,-15.084549356486));
#31025=CARTESIAN_POINT('Ctrl Pts',(92.,-14.1178978857168,-15.2159036206765));
#31026=CARTESIAN_POINT('Ctrl Pts',(92.,-14.0488781796834,-15.2823920812989));
#31027=CARTESIAN_POINT('Ctrl Pts',(92.,-13.9793736127407,-15.3484225538464));
#31028=CARTESIAN_POINT('Ctrl Pts',(92.,-13.9093893078444,-15.4139906160304));
#31029=CARTESIAN_POINT('Ctrl Pts',(92.,-13.8830137967218,-15.438701744561));
#31030=CARTESIAN_POINT('Ctrl Pts',(92.,-13.8565693542944,-15.4633479251348));
#31031=CARTESIAN_POINT('Ctrl Pts',(92.,-13.8300587085628,-15.4879266405824));
#31032=CARTESIAN_POINT('Ctrl Pts',(92.,-13.5167319996439,-15.7784200558922));
#31033=CARTESIAN_POINT('Ctrl Pts',(92.,-13.1948692359732,-16.058836627676));
#31034=CARTESIAN_POINT('Ctrl Pts',(92.,-12.8650638961591,-16.3289305947836));
#31035=CARTESIAN_POINT('Ctrl Pts',(92.,-12.5319527241127,-16.6017318720359));
#31036=CARTESIAN_POINT('Ctrl Pts',(92.,-12.1907385840942,-16.8640029162961));
#31037=CARTESIAN_POINT('Ctrl Pts',(92.,-11.8419899279349,-17.115458924327));
#31038=CARTESIAN_POINT('Ctrl Pts',(92.,-11.4912672606211,-17.3683382409669));
#31039=CARTESIAN_POINT('Ctrl Pts',(92.,-11.1329241297363,-17.6102800876755));
#31040=CARTESIAN_POINT('Ctrl Pts',(92.,-10.76750130731,-17.8409578158456));
#31041=CARTESIAN_POINT('Ctrl Pts',(92.,-10.4024136912143,-18.0714239408261));
#31042=CARTESIAN_POINT('Ctrl Pts',(92.,-10.0302589179817,-18.2906469148638));
#31043=CARTESIAN_POINT('Ctrl Pts',(92.,-9.65154557559993,-18.4982593079888));
#31044=CARTESIAN_POINT('Ctrl Pts',(92.,-9.27493495961211,-18.7047189768501));
#31045=CARTESIAN_POINT('Ctrl Pts',(92.,-8.8918379483303,-18.8996969149001));
#31046=CARTESIAN_POINT('Ctrl Pts',(92.,-8.50273110093215,-19.0827861959131));
#31047=CARTESIAN_POINT('Ctrl Pts',(92.,-8.11885407809306,-19.2634146494574));
#31048=CARTESIAN_POINT('Ctrl Pts',(92.,-7.72912723839731,-19.432472082855));
#31049=CARTESIAN_POINT('Ctrl Pts',(92.,-7.33399185124482,-19.5895198058331));
#31050=CARTESIAN_POINT('Ctrl Pts',(92.,-7.21554722023826,-19.6365959731504));
#31051=CARTESIAN_POINT('Ctrl Pts',(92.,-7.09661652008284,-19.6825926742559));
#31052=CARTESIAN_POINT('Ctrl Pts',(92.,-6.97721143603873,-19.7274971949513));
#31053=CARTESIAN_POINT('Ctrl Pts',(92.,-6.97721143603902,-19.7274971949512));
#31054=CARTESIAN_POINT('Ctrl Pts',(91.9603817120854,-10.2510427877189,-18.5696101441574));
#31055=CARTESIAN_POINT('Ctrl Pts',(91.9207634241708,-13.229456860328,-16.5816722919714));
#31056=CARTESIAN_POINT('Ctrl Pts',(91.8811451362562,-15.5522390204362,-14.0021338613507));
#31057=CARTESIAN_POINT('Ctrl Pts',(91.8415268483417,-17.8750211805444,-11.4225954307301));
#31058=CARTESIAN_POINT('Ctrl Pts',(91.8019085604271,-19.5421714281517,-8.25145642167493));
#31059=CARTESIAN_POINT('Ctrl Pts',(91.7622902725125,-20.350996970433,-4.87518526992051));
#31060=CARTESIAN_POINT('Ctrl Pts',(91.7435791307256,-20.7329935230127,-3.28062145717681));
#31061=CARTESIAN_POINT('Ctrl Pts',(91.7248679889387,-20.923537688795,-1.64030218838607));
#31062=CARTESIAN_POINT('Ctrl Pts',(91.7061568471519,-20.9232794228044,4.20060754047213E-5));
#31063=CARTESIAN_POINT('Origin',(101.6,4.3,25.25));
#31064=CARTESIAN_POINT('',(101.,4.3,34.));
#31065=CARTESIAN_POINT('',(101.6,4.9,36.8354893757516));
#31066=CARTESIAN_POINT('Ctrl Pts',(101.,4.3,34.));
#31067=CARTESIAN_POINT('Ctrl Pts',(101.,4.44326450824761,34.4893414541742));
#31068=CARTESIAN_POINT('Ctrl Pts',(101.064916666253,4.61344480367674,35.0734607689975));
#31069=CARTESIAN_POINT('Ctrl Pts',(101.268537390365,4.81706552778855,35.9649713605754));
#31070=CARTESIAN_POINT('Ctrl Pts',(101.427042536443,4.9,36.4451060520726));
#31071=CARTESIAN_POINT('Ctrl Pts',(101.6,4.9,36.8354893757516));
#31072=CARTESIAN_POINT('',(101.6,4.9,25.5340948537441));
#31073=CARTESIAN_POINT('',(101.6,4.9,25.25));
#31074=CARTESIAN_POINT('',(101.,4.3,25.6419578035687));
#31075=CARTESIAN_POINT('Ctrl Pts',(101.,4.3,25.6419578035687));
#31076=CARTESIAN_POINT('Ctrl Pts',(101.,4.37551113136118,25.6292950471856));
#31077=CARTESIAN_POINT('Ctrl Pts',(101.015114297469,4.45605670300991,25.6154099532735));
#31078=CARTESIAN_POINT('Ctrl Pts',(101.076714673797,4.60433114552009,25.5891735528367));
#31079=CARTESIAN_POINT('Ctrl Pts',(101.123204104127,4.67206195455091,25.5768410722651));
#31080=CARTESIAN_POINT('Ctrl Pts',(101.230018577124,4.7782143249361,25.5572207559602));
#31081=CARTESIAN_POINT('Ctrl Pts',(101.297146680589,4.82405550675615,25.5485703918952));
#31082=CARTESIAN_POINT('Ctrl Pts',(101.44448562384,4.88495263372662,25.5369966591618));
#31083=CARTESIAN_POINT('Ctrl Pts',(101.524701702258,4.9,25.5340948537441));
#31084=CARTESIAN_POINT('Ctrl Pts',(101.6,4.9,25.5340948537441));
#31085=CARTESIAN_POINT('',(101.,4.3,25.25));
#31086=CARTESIAN_POINT('Origin',(108.,-4.9,34.));
#31087=CARTESIAN_POINT('',(101.,-4.3,34.));
#31088=CARTESIAN_POINT('',(101.,-4.9,34.));
#31089=CARTESIAN_POINT('',(101.6,-4.9,36.8354893757516));
#31090=CARTESIAN_POINT('Ctrl Pts',(101.6,-4.9,36.8354893757516));
#31091=CARTESIAN_POINT('Ctrl Pts',(101.427042536443,-4.9,36.4451060520726));
#31092=CARTESIAN_POINT('Ctrl Pts',(101.268537390365,-4.81706552778855,35.9649713605754));
#31093=CARTESIAN_POINT('Ctrl Pts',(101.064916666253,-4.61344480367674,35.0734607689975));
#31094=CARTESIAN_POINT('Ctrl Pts',(101.,-4.44326450824761,34.4893414541742));
#31095=CARTESIAN_POINT('Ctrl Pts',(101.,-4.3,34.));
#31096=CARTESIAN_POINT('',(114.402897902826,-4.9,36.8289394560486));
#31097=CARTESIAN_POINT('Origin',(108.,-4.9,34.));
#31098=CARTESIAN_POINT('',(115.,-4.35889894354063,34.));
#31099=CARTESIAN_POINT('Ctrl Pts',(115.,-4.35889894354085,34.));
#31100=CARTESIAN_POINT('Ctrl Pts',(115.,-4.35889894354085,34.1229692605315));
#31101=CARTESIAN_POINT('Ctrl Pts',(114.996901424204,-4.39006230423687,34.2401264537803));
#31102=CARTESIAN_POINT('Ctrl Pts',(114.984616986144,-4.45009707127197,34.4790000665593));
#31103=CARTESIAN_POINT('Ctrl Pts',(114.975348582715,-4.48313072407473,34.5996468313749));
#31104=CARTESIAN_POINT('Ctrl Pts',(114.937384384277,-4.58154753518053,34.9658966690121));
#31105=CARTESIAN_POINT('Ctrl Pts',(114.898348782177,-4.64734858287202,35.2151996628246));
#31106=CARTESIAN_POINT('Ctrl Pts',(114.745032017671,-4.81487871806176,35.9328510722238));
#31107=CARTESIAN_POINT('Ctrl Pts',(114.592738308154,-4.90000000000001,36.3992629811611));
#31108=CARTESIAN_POINT('Ctrl Pts',(114.402897902826,-4.90000000000001,36.8289394560486));
#31109=CARTESIAN_POINT('Ctrl Pts',(115.,-4.35889894354063,34.));
#31110=CARTESIAN_POINT('Ctrl Pts',(115.,-4.35889894354063,34.4224068534569));
#31111=CARTESIAN_POINT('Ctrl Pts',(114.958162834155,-4.27540728759944,34.8694586605386));
#31112=CARTESIAN_POINT('Ctrl Pts',(114.806829998337,-3.93948854882627,35.6849438766281));
#31113=CARTESIAN_POINT('Ctrl Pts',(114.699216397495,-3.68627980790566,36.0534032907636));
#31114=CARTESIAN_POINT('Ctrl Pts',(114.552214908899,-3.27956064047775,36.4668024429472));
#31115=CARTESIAN_POINT('Ctrl Pts',(114.504985020473,-3.14149575848544,36.5883975490726));
#31116=CARTESIAN_POINT('Ctrl Pts',(114.458327956987,-2.99274032010601,36.6999999999994));
#31117=CARTESIAN_POINT('',(115.,4.35889894354063,34.));
#31118=CARTESIAN_POINT('Ctrl Pts',(114.458327956987,2.99274032010601,36.6999999999995));
#31119=CARTESIAN_POINT('Ctrl Pts',(114.504985020473,3.14149575848544,36.5883975490726));
#31120=CARTESIAN_POINT('Ctrl Pts',(114.552214908899,3.27956064047774,36.4668024429472));
#31121=CARTESIAN_POINT('Ctrl Pts',(114.699216397495,3.68627980790566,36.0534032907636));
#31122=CARTESIAN_POINT('Ctrl Pts',(114.806829998337,3.93948854882627,35.6849438766281));
#31123=CARTESIAN_POINT('Ctrl Pts',(114.958162834155,4.27540728759944,34.8694586605386));
#31124=CARTESIAN_POINT('Ctrl Pts',(115.,4.35889894354063,34.4224068534569));
#31125=CARTESIAN_POINT('Ctrl Pts',(115.,4.35889894354063,34.));
#31126=CARTESIAN_POINT('',(114.402897902826,4.9,36.8289394560486));
#31127=CARTESIAN_POINT('Ctrl Pts',(114.402897902826,4.90000000000001,36.8289394560486));
#31128=CARTESIAN_POINT('Ctrl Pts',(114.592738308154,4.90000000000001,36.3992629811611));
#31129=CARTESIAN_POINT('Ctrl Pts',(114.745032017671,4.81487871806176,35.9328510722238));
#31130=CARTESIAN_POINT('Ctrl Pts',(114.898348782177,4.64734858287202,35.2151996628246));
#31131=CARTESIAN_POINT('Ctrl Pts',(114.937384384277,4.58154753518053,34.9658966690121));
#31132=CARTESIAN_POINT('Ctrl Pts',(114.975348582715,4.48313072407473,34.5996468313749));
#31133=CARTESIAN_POINT('Ctrl Pts',(114.984616986144,4.45009707127197,34.4790000665593));
#31134=CARTESIAN_POINT('Ctrl Pts',(114.996901424204,4.39006230423687,34.2401264537803));
#31135=CARTESIAN_POINT('Ctrl Pts',(115.,4.35889894354085,34.1229692605315));
#31136=CARTESIAN_POINT('Ctrl Pts',(115.,4.35889894354085,34.));
#31137=CARTESIAN_POINT('Origin',(108.,4.9,34.));
#31138=CARTESIAN_POINT('Origin',(101.,-4.9,20.));
#31139=CARTESIAN_POINT('',(101.,-4.3,25.6419578035687));
#31140=CARTESIAN_POINT('Origin',(101.,0.,0.));
#31141=CARTESIAN_POINT('',(101.,-4.3,25.25));
#31142=CARTESIAN_POINT('Origin',(101.6,-4.3,25.25));
#31143=CARTESIAN_POINT('',(101.6,-4.9,25.5340948537441));
#31144=CARTESIAN_POINT('Ctrl Pts',(101.6,-4.9,25.5340948537441));
#31145=CARTESIAN_POINT('Ctrl Pts',(101.524701702258,-4.9,25.5340948537441));
#31146=CARTESIAN_POINT('Ctrl Pts',(101.44448562384,-4.88495263372662,25.5369966591618));
#31147=CARTESIAN_POINT('Ctrl Pts',(101.297146680589,-4.82405550675615,25.5485703918952));
#31148=CARTESIAN_POINT('Ctrl Pts',(101.230018577124,-4.7782143249361,25.5572207559602));
#31149=CARTESIAN_POINT('Ctrl Pts',(101.123204104127,-4.67206195455091,25.5768410722651));
#31150=CARTESIAN_POINT('Ctrl Pts',(101.076714673797,-4.60433114552009,25.5891735528367));
#31151=CARTESIAN_POINT('Ctrl Pts',(101.015114297469,-4.4560567030099,25.6154099532735));
#31152=CARTESIAN_POINT('Ctrl Pts',(101.,-4.37551113136118,25.6292950471856));
#31153=CARTESIAN_POINT('Ctrl Pts',(101.,-4.3,25.6419578035687));
#31154=CARTESIAN_POINT('',(101.6,-4.9,25.25));
#31155=CARTESIAN_POINT('Origin',(114.402897902826,4.3,10.));
#31156=CARTESIAN_POINT('',(114.402897902826,4.9,25.5340948537441));
#31157=CARTESIAN_POINT('',(115.,4.35889894354067,25.6320112359526));
#31158=CARTESIAN_POINT('Ctrl Pts',(114.402897902826,4.9,25.5340948537441));
#31159=CARTESIAN_POINT('Ctrl Pts',(114.478511084744,4.90000000000001,25.5340948537441));
#31160=CARTESIAN_POINT('Ctrl Pts',(114.559040039281,4.88482760707762,25.5370208646519));
#31161=CARTESIAN_POINT('Ctrl Pts',(114.706854852562,4.82346334338894,25.5486824859048));
#31162=CARTESIAN_POINT('Ctrl Pts',(114.774145994538,4.77728004571152,25.5573962293562));
#31163=CARTESIAN_POINT('Ctrl Pts',(114.880625044276,4.67080099597391,25.5770712542939));
#31164=CARTESIAN_POINT('Ctrl Pts',(114.926771808833,4.60323529106133,25.5893699985255));
#31165=CARTESIAN_POINT('Ctrl Pts',(114.980036874495,4.47446184335992,25.6121513464705));
#31166=CARTESIAN_POINT('Ctrl Pts',(114.994355992236,4.4161164192633,25.6222810125931));
#31167=CARTESIAN_POINT('Ctrl Pts',(115.,4.35889894354067,25.6320112359526));
#31168=CARTESIAN_POINT('',(114.402897902826,4.9,10.));
#31169=CARTESIAN_POINT('',(115.,4.35889894354067,10.));
#31170=CARTESIAN_POINT('Origin',(114.402897902826,-4.3,10.));
#31171=CARTESIAN_POINT('',(114.402897902826,-4.9,25.5340948537441));
#31172=CARTESIAN_POINT('',(114.402897902826,-4.9,10.));
#31173=CARTESIAN_POINT('',(115.,-4.35889894354067,25.6320112359526));
#31174=CARTESIAN_POINT('Ctrl Pts',(115.,-4.35889894354067,25.6320112359526));
#31175=CARTESIAN_POINT('Ctrl Pts',(114.994326080485,-4.41641965677671,25.6222294449785));
#31176=CARTESIAN_POINT('Ctrl Pts',(114.979885641476,-4.47506740166339,25.6120461078662));
#31177=CARTESIAN_POINT('Ctrl Pts',(114.926183229029,-4.60433114552009,25.5891735528367));
#31178=CARTESIAN_POINT('Ctrl Pts',(114.879693798699,-4.67206195455091,25.5768410722651));
#31179=CARTESIAN_POINT('Ctrl Pts',(114.772879325702,-4.7782143249361,25.5572207559602));
#31180=CARTESIAN_POINT('Ctrl Pts',(114.705751222236,-4.82405550675616,25.5485703918952));
#31181=CARTESIAN_POINT('Ctrl Pts',(114.558412278986,-4.88495263372663,25.5369966591618));
#31182=CARTESIAN_POINT('Ctrl Pts',(114.478196200568,-4.9,25.5340948537441));
#31183=CARTESIAN_POINT('Ctrl Pts',(114.402897902826,-4.9,25.5340948537441));
#31184=CARTESIAN_POINT('',(115.,-4.35889894354067,10.));
#31185=CARTESIAN_POINT('Origin',(136.,-29.8,0.));
#31186=CARTESIAN_POINT('',(130.55,-30.,-6.67432505535307E-16));
#31187=CARTESIAN_POINT('Origin',(136.,-30.,0.));
#31188=CARTESIAN_POINT('',(130.95,-29.6,6.18446633569414E-16));
#31189=CARTESIAN_POINT('',(130.75,-29.8,-6.42939569552361E-16));
#31190=CARTESIAN_POINT('Origin',(136.,-29.6,0.));
#31191=CARTESIAN_POINT('Origin',(136.,-30.,0.));
#31192=CARTESIAN_POINT('',(123.8,-30.,1.49406909495977E-15));
#31193=CARTESIAN_POINT('Origin',(136.,-30.,0.));
#31194=CARTESIAN_POINT('Origin',(136.,-30.,0.));
#31195=CARTESIAN_POINT('',(130.95,-14.,6.18446633569414E-16));
#31196=CARTESIAN_POINT('',(130.95,-30.,6.18446633569414E-16));
#31197=CARTESIAN_POINT('Origin',(136.,-14.,0.));
#31198=CARTESIAN_POINT('Origin',(124.,0.,37.8));
#31199=CARTESIAN_POINT('',(119.99,4.91083366458088E-16,37.6));
#31200=CARTESIAN_POINT('',(119.79,-5.15576302441035E-16,37.8));
#31201=CARTESIAN_POINT('Origin',(124.,0.,37.6));
#31202=CARTESIAN_POINT('Origin',(124.,0.,38.));
#31203=CARTESIAN_POINT('',(119.99,-4.91083366458088E-16,14.));
#31204=CARTESIAN_POINT('',(119.99,4.91083366458088E-16,38.));
#31205=CARTESIAN_POINT('Origin',(124.,0.,14.));
#31206=CARTESIAN_POINT('Origin',(136.,-29.6,0.));
#31207=CARTESIAN_POINT('',(123.,-29.2,-1.59204083889156E-15));
#31208=CARTESIAN_POINT('',(123.4,-29.6,-1.54305496692567E-15));
#31209=CARTESIAN_POINT('Origin',(136.,-29.2,0.));
#31210=CARTESIAN_POINT('Origin',(136.,-10.,0.));
#31211=CARTESIAN_POINT('',(123.,-26.,1.75424727101232E-16));
#31212=CARTESIAN_POINT('',(123.,-10.,-1.59204083889156E-15));
#31213=CARTESIAN_POINT('Ctrl Pts',(149.,-26.,2.22044604925031E-15));
#31214=CARTESIAN_POINT('Ctrl Pts',(149.,-26.,-0.831709457206476));
#31215=CARTESIAN_POINT('Ctrl Pts',(148.918892814918,-25.9591289790221,-1.68724313385081));
#31216=CARTESIAN_POINT('Ctrl Pts',(148.582552741345,-25.7933948769122,-3.37993305619291));
#31217=CARTESIAN_POINT('Ctrl Pts',(148.327434591979,-25.6686324247972,-4.21712194988806));
#31218=CARTESIAN_POINT('Ctrl Pts',(147.32514603902,-25.1974429335132,-6.61362985548687));
#31219=CARTESIAN_POINT('Ctrl Pts',(146.328719603369,-24.7502659309165,-8.05605670748142));
#31220=CARTESIAN_POINT('Ctrl Pts',(144.052950545147,-23.8901060781349,-10.3318257657034));
#31221=CARTESIAN_POINT('Ctrl Pts',(142.611570673602,-23.4155481619888,-11.325973226571));
#31222=CARTESIAN_POINT('Ctrl Pts',(140.218494030717,-22.8951850410383,-12.3268777552912));
#31223=CARTESIAN_POINT('Ctrl Pts',(139.382475328567,-22.7537733940447,-12.5818558368984));
#31224=CARTESIAN_POINT('Ctrl Pts',(137.690251278654,-22.5643527281993,-12.9184862150897));
#31225=CARTESIAN_POINT('Ctrl Pts',(136.833982935243,-22.5166604983954,-13.));
#31226=CARTESIAN_POINT('Ctrl Pts',(136.,-22.5166604983954,-13.));
#31227=CARTESIAN_POINT('Ctrl Pts',(135.166017064757,-22.5166604983954,-13.));
#31228=CARTESIAN_POINT('Ctrl Pts',(134.309748721346,-22.5643527281993,-12.9184862150897));
#31229=CARTESIAN_POINT('Ctrl Pts',(132.617524671433,-22.7537733940447,-12.5818558368984));
#31230=CARTESIAN_POINT('Ctrl Pts',(131.781505969283,-22.8951850410383,-12.3268777552912));
#31231=CARTESIAN_POINT('Ctrl Pts',(129.388429326398,-23.4155481619888,-11.325973226571));
#31232=CARTESIAN_POINT('Ctrl Pts',(127.947049454853,-23.8901060781349,-10.3318257657035));
#31233=CARTESIAN_POINT('Ctrl Pts',(125.671280396631,-24.7502659309165,-8.05605670748142));
#31234=CARTESIAN_POINT('Ctrl Pts',(124.67485396098,-25.1974429335132,-6.61362985548688));
#31235=CARTESIAN_POINT('Ctrl Pts',(123.672565408021,-25.6686324247972,-4.21712194988807));
#31236=CARTESIAN_POINT('Ctrl Pts',(123.417447258655,-25.7933948769122,-3.37993305619291));
#31237=CARTESIAN_POINT('Ctrl Pts',(123.081107185082,-25.9591289790221,-1.68724313385082));
#31238=CARTESIAN_POINT('Ctrl Pts',(123.,-26.,-0.831709457206481));
#31239=CARTESIAN_POINT('Ctrl Pts',(123.,-26.,1.38777878078145E-15));
#31240=CARTESIAN_POINT('Ctrl Pts',(123.,-26.,1.94289029309402E-15));
#31241=CARTESIAN_POINT('Ctrl Pts',(123.,-26.,0.831709457206478));
#31242=CARTESIAN_POINT('Ctrl Pts',(123.081107185082,-25.9591289790221,1.68724313385081));
#31243=CARTESIAN_POINT('Ctrl Pts',(123.417447258655,-25.7933948769122,3.37993305619291));
#31244=CARTESIAN_POINT('Ctrl Pts',(123.672565408021,-25.6686324247972,4.21712194988806));
#31245=CARTESIAN_POINT('Ctrl Pts',(124.67485396098,-25.1974429335132,6.61362985548687));
#31246=CARTESIAN_POINT('Ctrl Pts',(125.671280396631,-24.7502659309165,8.05605670748142));
#31247=CARTESIAN_POINT('Ctrl Pts',(127.947049454853,-23.8901060781349,10.3318257657034));
#31248=CARTESIAN_POINT('Ctrl Pts',(129.388429326398,-23.4155481619888,11.325973226571));
#31249=CARTESIAN_POINT('Ctrl Pts',(131.781505969283,-22.8951850410383,12.3268777552912));
#31250=CARTESIAN_POINT('Ctrl Pts',(132.617524671433,-22.7537733940447,12.5818558368984));
#31251=CARTESIAN_POINT('Ctrl Pts',(134.309748721346,-22.5643527281993,12.9184862150897));
#31252=CARTESIAN_POINT('Ctrl Pts',(135.166017064757,-22.5166604983954,13.));
#31253=CARTESIAN_POINT('Ctrl Pts',(136.833982935243,-22.5166604983954,13.));
#31254=CARTESIAN_POINT('Ctrl Pts',(137.690251278654,-22.5643527281993,12.9184862150897));
#31255=CARTESIAN_POINT('Ctrl Pts',(139.382475328567,-22.7537733940447,12.5818558368984));
#31256=CARTESIAN_POINT('Ctrl Pts',(140.218494030717,-22.8951850410383,12.3268777552912));
#31257=CARTESIAN_POINT('Ctrl Pts',(142.611570673602,-23.4155481619888,11.325973226571));
#31258=CARTESIAN_POINT('Ctrl Pts',(144.052950545147,-23.8901060781349,10.3318257657035));
#31259=CARTESIAN_POINT('Ctrl Pts',(146.328719603369,-24.7502659309165,8.05605670748142));
#31260=CARTESIAN_POINT('Ctrl Pts',(147.32514603902,-25.1974429335132,6.61362985548688));
#31261=CARTESIAN_POINT('Ctrl Pts',(148.327434591979,-25.6686324247972,4.21712194988807));
#31262=CARTESIAN_POINT('Ctrl Pts',(148.582552741345,-25.7933948769122,3.37993305619291));
#31263=CARTESIAN_POINT('Ctrl Pts',(148.918892814918,-25.9591289790221,1.68724313385082));
#31264=CARTESIAN_POINT('Ctrl Pts',(149.,-26.,0.831709457206481));
#31265=CARTESIAN_POINT('Ctrl Pts',(149.,-26.,2.22044604925031E-15));
#31266=CARTESIAN_POINT('Origin',(124.,0.,10.));
#31267=CARTESIAN_POINT('Ctrl Pts',(115.,4.35889894354066,25.6320112359526));
#31268=CARTESIAN_POINT('Ctrl Pts',(115.497714669606,5.38655112921263,25.4572519482316));
#31269=CARTESIAN_POINT('Ctrl Pts',(116.172977789672,6.31511341340259,25.2336373509982));
#31270=CARTESIAN_POINT('Ctrl Pts',(117.809882463292,7.9520180870225,24.7710207384202));
#31271=CARTESIAN_POINT('Ctrl Pts',(118.925456325839,8.7191257276253,24.500550059198));
#31272=CARTESIAN_POINT('Ctrl Pts',(121.384603519825,9.74339902991552,24.1115387621796));
#31273=CARTESIAN_POINT('Ctrl Pts',(122.729514475929,10.,24.));
#31274=CARTESIAN_POINT('Ctrl Pts',(125.270485524071,10.,24.));
#31275=CARTESIAN_POINT('Ctrl Pts',(126.615396480175,9.74339902991553,24.1115387621796));
#31276=CARTESIAN_POINT('Ctrl Pts',(129.074543674161,8.71912572762531,24.500550059198));
#31277=CARTESIAN_POINT('Ctrl Pts',(130.190117536708,7.9520180870225,24.7710207384202));
#31278=CARTESIAN_POINT('Ctrl Pts',(131.95126588442,6.19086973931097,25.2687506893427));
#31279=CARTESIAN_POINT('Ctrl Pts',(132.718946209375,5.07500736860867,25.5302046420434));
#31280=CARTESIAN_POINT('Ctrl Pts',(133.743654926725,2.61474940838325,25.8980720227517));
#31281=CARTESIAN_POINT('Ctrl Pts',(134.,1.2694007153771,26.));
#31282=CARTESIAN_POINT('Ctrl Pts',(134.,-1.26940071537709,26.));
#31283=CARTESIAN_POINT('Ctrl Pts',(133.743654926725,-2.61474940838325,25.8980720227516));
#31284=CARTESIAN_POINT('Ctrl Pts',(132.718946209375,-5.07500736860866,25.5302046420434));
#31285=CARTESIAN_POINT('Ctrl Pts',(131.95126588442,-6.19086973931097,25.2687506893427));
#31286=CARTESIAN_POINT('Ctrl Pts',(130.190117536708,-7.95201808702249,24.7710207384202));
#31287=CARTESIAN_POINT('Ctrl Pts',(129.074543674161,-8.7191257276253,24.500550059198));
#31288=CARTESIAN_POINT('Ctrl Pts',(126.615396480175,-9.74339902991553,24.1115387621796));
#31289=CARTESIAN_POINT('Ctrl Pts',(125.270485524071,-10.,24.));
#31290=CARTESIAN_POINT('Ctrl Pts',(124.,-10.,24.));
#31291=CARTESIAN_POINT('Ctrl Pts',(122.729514475929,-10.,24.));
#31292=CARTESIAN_POINT('Ctrl Pts',(121.384603519825,-9.74339902991552,24.1115387621796));
#31293=CARTESIAN_POINT('Ctrl Pts',(118.925456325839,-8.7191257276253,24.500550059198));
#31294=CARTESIAN_POINT('Ctrl Pts',(117.809882463292,-7.9520180870225,24.7710207384202));
#31295=CARTESIAN_POINT('Ctrl Pts',(116.172977789672,-6.31511341340259,25.2336373509982));
#31296=CARTESIAN_POINT('Ctrl Pts',(115.497714669606,-5.38655112921264,25.4572519482316));
#31297=CARTESIAN_POINT('Ctrl Pts',(115.,-4.35889894354067,25.6320112359526));
#31298=CARTESIAN_POINT('Origin',(136.,-14.,0.));
#31299=CARTESIAN_POINT('Origin',(124.,0.,14.));
#31300=CARTESIAN_POINT('Origin',(108.,-5.5,34.));
#31301=CARTESIAN_POINT('',(104.95,-4.9,34.));
#31302=CARTESIAN_POINT('Origin',(108.,-4.9,34.));
#31303=CARTESIAN_POINT('',(104.95,4.9,34.));
#31304=CARTESIAN_POINT('',(104.95,-5.5,34.));
#31305=CARTESIAN_POINT('Origin',(108.,4.9,34.));
#31306=CARTESIAN_POINT('Origin',(121.,0.,0.));
#31307=CARTESIAN_POINT('',(93.,-26.,-3.18408167778312E-15));
#31308=CARTESIAN_POINT('',(121.,-26.,-3.18408167778312E-15));
#31309=CARTESIAN_POINT('Origin',(93.,0.,0.));
#31310=CARTESIAN_POINT('',(121.,-4.9,25.5340948537441));
#31311=CARTESIAN_POINT('',(121.,4.9,25.5340948537441));
#31312=CARTESIAN_POINT('Origin',(108.,-4.9,30.5));
#31313=CARTESIAN_POINT('Origin',(108.,4.9,30.5));
#31314=CARTESIAN_POINT('Origin',(89.,0.,0.));
#31315=CARTESIAN_POINT('',(68.,-18.,-2.20436423846524E-15));
#31316=CARTESIAN_POINT('',(89.,-18.,-2.20436423846524E-15));
#31317=CARTESIAN_POINT('Origin',(68.,0.,0.));
#31318=CARTESIAN_POINT('Origin',(68.,20.2,0.));
#31319=CARTESIAN_POINT('',(68.,-20.2,-2.47378653427765E-15));
#31320=CARTESIAN_POINT('Origin',(68.,0.,0.));
#31321=CARTESIAN_POINT('Origin',(68.4,0.,0.));
#31322=CARTESIAN_POINT('',(68.4,-20.6,-2.52277240624355E-15));
#31323=CARTESIAN_POINT('Origin',(80.4,0.,0.));
#31324=CARTESIAN_POINT('Origin',(92.,0.,0.));
#31325=CARTESIAN_POINT('Origin',(92.,25.,0.));
#31326=CARTESIAN_POINT('',(92.,-25.,-3.06161699786838E-15));
#31327=CARTESIAN_POINT('Origin',(92.,0.,0.));
#31328=CARTESIAN_POINT('Origin',(92.5,0.,0.));
#31329=CARTESIAN_POINT('',(92.5,-25.5,-3.12284933782575E-15));
#31330=CARTESIAN_POINT('Origin',(165.6,0.,0.));
#31331=CARTESIAN_POINT('',(165.6,-16.1,-1.97168134662724E-15));
#31332=CARTESIAN_POINT('',(0.,0.,0.));
#31333=CARTESIAN_POINT('Origin',(57.,0.,0.));
#31334=CARTESIAN_POINT('',(57.,-3.73517273739943E-16,3.05));
#31335=CARTESIAN_POINT('Origin',(57.,0.,0.));
#31336=CARTESIAN_POINT('',(62.1,-3.73517273739943E-16,3.05));
#31337=CARTESIAN_POINT('',(57.,-3.73517273739943E-16,3.05));
#31338=CARTESIAN_POINT('Origin',(62.1,0.,0.));
#31339=CARTESIAN_POINT('Origin',(62.1,0.,0.));
#31340=CARTESIAN_POINT('Origin',(57.,14.2,0.));
#31341=CARTESIAN_POINT('',(57.,-14.2,-1.73899845478924E-15));
#31342=CARTESIAN_POINT('Origin',(57.,0.,0.));
#31343=CARTESIAN_POINT('Origin',(57.4,0.,0.));
#31344=CARTESIAN_POINT('',(57.8,-15.,-1.83697019872103E-15));
#31345=CARTESIAN_POINT('Origin',(57.8,0.,0.));
#31346=CARTESIAN_POINT('',(57.4,-14.6,-1.78798432675514E-15));
#31347=CARTESIAN_POINT('Origin',(73.9,0.,0.));
#31348=CARTESIAN_POINT('',(90.,-15.,-1.83697019872103E-15));
#31349=CARTESIAN_POINT('Origin',(90.,0.,0.));
#31350=CARTESIAN_POINT('',(73.9,-15.,-1.83697019872103E-15));
#31351=CARTESIAN_POINT('Origin',(90.,17.46,0.));
#31352=CARTESIAN_POINT('',(90.,-17.46,-2.13823331131128E-15));
#31353=CARTESIAN_POINT('Origin',(90.,0.,0.));
#31354=CARTESIAN_POINT('Origin',(90.25,0.,0.));
#31355=CARTESIAN_POINT('',(90.5,-17.96,-2.19946565126865E-15));
#31356=CARTESIAN_POINT('Origin',(90.5,0.,0.));
#31357=CARTESIAN_POINT('',(90.25,-17.71,-2.16884948128996E-15));
#31358=CARTESIAN_POINT('Origin',(92.25,0.,0.));
#31359=CARTESIAN_POINT('',(94.,-17.96,-2.19946565126865E-15));
#31360=CARTESIAN_POINT('Origin',(94.,0.,0.));
#31361=CARTESIAN_POINT('',(92.25,-17.96,-2.19946565126865E-15));
#31362=CARTESIAN_POINT('Origin',(94.,15.05,0.));
#31363=CARTESIAN_POINT('',(94.,-15.05,-1.84309343271677E-15));
#31364=CARTESIAN_POINT('Origin',(94.,0.,0.));
#31365=CARTESIAN_POINT('Origin',(96.6,0.,0.));
#31366=CARTESIAN_POINT('',(99.2,-15.05,-1.84309343271677E-15));
#31367=CARTESIAN_POINT('Origin',(99.2,0.,0.));
#31368=CARTESIAN_POINT('',(96.6,-15.05,-1.84309343271677E-15));
#31369=CARTESIAN_POINT('Origin',(99.2,17.96,0.));
#31370=CARTESIAN_POINT('',(99.2,-17.96,-2.19946565126865E-15));
#31371=CARTESIAN_POINT('Origin',(99.2,0.,0.));
#31372=CARTESIAN_POINT('Origin',(100.6,0.,0.));
#31373=CARTESIAN_POINT('',(102.,-17.96,-2.19946565126865E-15));
#31374=CARTESIAN_POINT('Origin',(102.,0.,0.));
#31375=CARTESIAN_POINT('',(100.6,-17.96,-2.19946565126865E-15));
#31376=CARTESIAN_POINT('Origin',(102.,15.05,0.));
#31377=CARTESIAN_POINT('',(102.,-15.05,-1.84309343271677E-15));
#31378=CARTESIAN_POINT('Origin',(102.,0.,0.));
#31379=CARTESIAN_POINT('Origin',(103.6,0.,0.));
#31380=CARTESIAN_POINT('',(105.2,-15.05,-1.84309343271677E-15));
#31381=CARTESIAN_POINT('Origin',(105.2,0.,0.));
#31382=CARTESIAN_POINT('',(103.6,-15.05,-1.84309343271677E-15));
#31383=CARTESIAN_POINT('Origin',(105.2,17.96,0.));
#31384=CARTESIAN_POINT('',(105.2,-17.96,-2.19946565126865E-15));
#31385=CARTESIAN_POINT('Origin',(105.2,0.,0.));
#31386=CARTESIAN_POINT('Origin',(107.3,0.,0.));
#31387=CARTESIAN_POINT('',(109.4,-17.96,-2.19946565126865E-15));
#31388=CARTESIAN_POINT('Origin',(109.4,0.,0.));
#31389=CARTESIAN_POINT('',(107.3,-17.96,-2.19946565126865E-15));
#31390=CARTESIAN_POINT('Origin',(109.65,0.,0.));
#31391=CARTESIAN_POINT('',(109.9,-17.46,-2.13823331131128E-15));
#31392=CARTESIAN_POINT('Origin',(109.9,0.,0.));
#31393=CARTESIAN_POINT('',(109.65,-17.71,-2.16884948128996E-15));
#31394=CARTESIAN_POINT('Origin',(109.9,0.,0.));
#31395=CARTESIAN_POINT('',(0.,0.,0.));
#31396=CARTESIAN_POINT('Ctrl Pts',(69.6184828603025,16.4616571598233,-0.030902239567753));
#31397=CARTESIAN_POINT('Ctrl Pts',(69.6789219655699,16.458754897209,1.53438465601481));
#31398=CARTESIAN_POINT('Ctrl Pts',(69.7997830801149,16.0266321943109,4.57501994136558));
#31399=CARTESIAN_POINT('Ctrl Pts',(70.0414349064678,13.4941722421641,10.2617903021912));
#31400=CARTESIAN_POINT('Ctrl Pts',(70.3432064666604,7.54051932200945,15.5847054098009));
#31401=CARTESIAN_POINT('Ctrl Pts',(70.7049768750637,-1.90873983484295,17.1894487135762));
#31402=CARTESIAN_POINT('Ctrl Pts',(71.0663492060979,-10.7475553396686,13.525924310196));
#31403=CARTESIAN_POINT('Ctrl Pts',(71.4273437518671,-16.2818464768058,5.72657424978343));
#31404=CARTESIAN_POINT('Ctrl Pts',(71.7278512234343,-16.7210289894503,-2.21659997283488));
#31405=CARTESIAN_POINT('Ctrl Pts',(71.9680675578449,-14.5106197428725,-7.98557322489482));
#31406=CARTESIAN_POINT('Ctrl Pts',(72.1481344157904,-11.7288725172833,-11.6852538002611));
#31407=CARTESIAN_POINT('Ctrl Pts',(72.328106524648,-8.03024824250695,-14.4669696417765));
#31408=CARTESIAN_POINT('Ctrl Pts',(72.5279702250768,-3.22977654241172,-16.300670274406));
#31409=CARTESIAN_POINT('Ctrl Pts',(72.7476856540044,2.4587525001183,-16.5141747132305));
#31410=CARTESIAN_POINT('Ctrl Pts',(72.9872078330289,8.31673840998305,-14.4634243432854));
#31411=CARTESIAN_POINT('Ctrl Pts',(73.2265632969346,13.0163496494046,-10.4182667032949));
#31412=CARTESIAN_POINT('Ctrl Pts',(73.4657526686465,15.9141590581627,-4.93897396144999));
#31413=CARTESIAN_POINT('Ctrl Pts',(73.7047766516472,16.6034312776959,1.21397241511146));
#31414=CARTESIAN_POINT('Ctrl Pts',(73.9834458021771,14.7409225736484,8.19195097348461));
#31415=CARTESIAN_POINT('Ctrl Pts',(74.301651818573,9.13086318160831,14.4766680019069));
#31416=CARTESIAN_POINT('Ctrl Pts',(74.6592672763964,0.0266353994119735,
17.0966775050227));
#31417=CARTESIAN_POINT('Ctrl Pts',(75.016519558125,-9.06348425632334,14.4765973593132));
#31418=CARTESIAN_POINT('Ctrl Pts',(75.3734117874807,-15.3610417662207,7.42742367726323));
#31419=CARTESIAN_POINT('Ctrl Pts',(75.7299471567895,-16.9418739975217,-1.88122771580553));
#31420=CARTESIAN_POINT('Ctrl Pts',(76.0861289312927,-13.3290621410899,-10.5975142741848));
#31421=CARTESIAN_POINT('Ctrl Pts',(76.4419606933661,-5.64617345782912,-16.0463992053949));
#31422=CARTESIAN_POINT('Ctrl Pts',(76.810612386967,4.11087115606672,-16.6005218369866));
#31423=CARTESIAN_POINT('Ctrl Pts',(77.0868204963524,10.4484384772329,-12.8295775485076));
#31424=CARTESIAN_POINT('Ctrl Pts',(77.3234199677928,14.1464940116618,-8.0565595801055));
#31425=CARTESIAN_POINT('Ctrl Pts',(77.5073642434964,16.0558684975652,-3.69288655028273));
#31426=CARTESIAN_POINT('Ctrl Pts',(77.743715642047,16.2835727900373,2.42892269363191));
#31427=CARTESIAN_POINT('Ctrl Pts',(77.9799198273595,14.2624210045081,8.20410639070391));
#31428=CARTESIAN_POINT('Ctrl Pts',(78.2159782861261,10.2721221270508,12.8404255794219));
#31429=CARTESIAN_POINT('Ctrl Pts',(78.451892297019,4.86870939460828,15.6955819848942));
#31430=CARTESIAN_POINT('Ctrl Pts',(78.687663274949,-1.20342672163651,16.3804065631851));
#31431=CARTESIAN_POINT('Ctrl Pts',(78.923292730736,-7.09646797598974,14.7976258939457));
#31432=CARTESIAN_POINT('Ctrl Pts',(79.1849474554113,-12.559397153018,10.7746599228106));
#31433=CARTESIAN_POINT('Ctrl Pts',(79.4202749429787,-15.5097121162534,5.34934186422077));
#31434=CARTESIAN_POINT('Ctrl Pts',(79.6946643695902,-16.3852200323318,-1.64037324259347));
#31435=CARTESIAN_POINT('Ctrl Pts',(79.9819403068823,-14.2884064522935,-8.94742064680176));
#31436=CARTESIAN_POINT('Ctrl Pts',(80.3342067288376,-7.3260467326971,-15.165426706738));
#31437=CARTESIAN_POINT('Ctrl Pts',(80.6861788812633,1.86167912032264,-16.7248261450382));
#31438=CARTESIAN_POINT('Ctrl Pts',(81.037862268153,10.4673895230379,-13.1602039003653));
#31439=CARTESIAN_POINT('Ctrl Pts',(81.3892625213115,15.8514527926196,-5.5687461546451));
#31440=CARTESIAN_POINT('Ctrl Pts',(81.7403859218982,16.3720606810702,3.71439472873355));
#31441=CARTESIAN_POINT('Ctrl Pts',(82.0912385240458,11.8761863054331,11.8495550298708));
#31442=CARTESIAN_POINT('Ctrl Pts',(82.4028723251709,4.65229996881944,15.8345467687591));
#31443=CARTESIAN_POINT('Ctrl Pts',(82.6753839687717,-2.4057965557233,16.0912478601411));
#31444=CARTESIAN_POINT('Ctrl Pts',(82.9088524431066,-8.11448174868296,14.0955831155642));
#31445=CARTESIAN_POINT('Ctrl Pts',(83.1422098352473,-12.6971950976412,10.1502287241044));
#31446=CARTESIAN_POINT('Ctrl Pts',(83.3754581634701,-15.522088392645,4.8081952387983));
#31447=CARTESIAN_POINT('Ctrl Pts',(83.6085992893649,-16.1966474690964,-1.19488542166675));
#31448=CARTESIAN_POINT('Ctrl Pts',(83.8416352233784,-14.6339538883274,-7.02670369688337));
#31449=CARTESIAN_POINT('Ctrl Pts',(84.0745679545012,-11.0497598473816,-11.8824317127295));
#31450=CARTESIAN_POINT('Ctrl Pts',(84.3073996737489,-5.94248428783527,-15.09263970399));
#31451=CARTESIAN_POINT('Ctrl Pts',(84.540132268385,-0.0171665032603614,
-16.2129461632812));
#31452=CARTESIAN_POINT('Ctrl Pts',(84.7727680106188,5.90520262635639,-15.0923025294507));
#31453=CARTESIAN_POINT('Ctrl Pts',(85.0053088744204,11.0065171159269,-11.8864785100097));
#31454=CARTESIAN_POINT('Ctrl Pts',(85.2377570340819,14.5833427924651,-7.04062680693156));
#31455=CARTESIAN_POINT('Ctrl Pts',(85.4701144791861,16.1401640578478,-1.22533588346504));
#31456=CARTESIAN_POINT('Ctrl Pts',(85.7023835299595,15.4662929248669,4.7550040735545));
#31457=CARTESIAN_POINT('Ctrl Pts',(85.9345662446591,12.6553888178413,10.0730373304554));
#31458=CARTESIAN_POINT('Ctrl Pts',(86.1666649327954,8.09679983295076,13.9966583914468));
#31459=CARTESIAN_POINT('Ctrl Pts',(86.3986815381799,2.42358552200963,15.9794357678464));
#31460=CARTESIAN_POINT('Ctrl Pts',(86.6692750541127,-4.58486198073758,15.7239726419428));
#31461=CARTESIAN_POINT('Ctrl Pts',(86.9783943834765,-11.7499252678846,11.7698005968098));
#31462=CARTESIAN_POINT('Ctrl Pts',(87.3259902517892,-16.2024151439095,3.70954956442589));
#31463=CARTESIAN_POINT('Ctrl Pts',(87.6734207471648,-15.6862303609498,-5.47622167055361));
#31464=CARTESIAN_POINT('Ctrl Pts',(88.0207132272952,-10.3628479251535,-12.9771513909202));
#31465=CARTESIAN_POINT('Ctrl Pts',(88.3678323138933,-1.8703041859877,-16.4954810466909));
#31466=CARTESIAN_POINT('Ctrl Pts',(88.7148821316246,7.193051660985,-14.9532751855446));
#31467=CARTESIAN_POINT('Ctrl Pts',(89.003856786706,12.8943942592402,-9.85553205895293));
#31468=CARTESIAN_POINT('Ctrl Pts',(89.2351907747089,15.3179503044652,-4.41141050395984));
#31469=CARTESIAN_POINT('Ctrl Pts',(89.3506074633962,15.7305922894428,-1.50774141983879));
#31470=CARTESIAN_POINT('Ctrl Pts',(89.4085387704217,15.7333741285005,-0.00740294277221285));
#31471=CARTESIAN_POINT('Ctrl Pts',(69.6299635796842,16.7007411089511,-0.030902239567753));
#31472=CARTESIAN_POINT('Ctrl Pts',(69.6912334101605,16.6977989552313,1.55589925782231));
#31473=CARTESIAN_POINT('Ctrl Pts',(69.8138990070948,16.2591916609345,4.64186903714546));
#31474=CARTESIAN_POINT('Ctrl Pts',(70.0590053500828,13.6903812708504,10.4098634757414));
#31475=CARTESIAN_POINT('Ctrl Pts',(70.3651870367565,7.65014590609584,15.8105713921737));
#31476=CARTESIAN_POINT('Ctrl Pts',(70.7321817761829,-1.93568018811406,17.4381266158968));
#31477=CARTESIAN_POINT('Ctrl Pts',(71.098790206296,-10.902202057407,13.7218082112497));
#31478=CARTESIAN_POINT('Ctrl Pts',(71.4649915562623,-16.5161793686399,5.80994623870215));
#31479=CARTESIAN_POINT('Ctrl Pts',(71.7698338155353,-16.9616095340376,-2.24746365248745));
#31480=CARTESIAN_POINT('Ctrl Pts',(72.0134956355215,-14.7194966934706,-8.09911469764596));
#31481=CARTESIAN_POINT('Ctrl Pts',(72.1961430998093,-11.8979192255808,-11.8517332522967));
#31482=CARTESIAN_POINT('Ctrl Pts',(72.3786898054422,-8.14642913059767,-14.6731732353235));
#31483=CARTESIAN_POINT('Ctrl Pts',(72.5814069366342,-3.2774945734574,-16.5329935539285));
#31484=CARTESIAN_POINT('Ctrl Pts',(72.8042563013791,2.492037402214,-16.7494956008958));
#31485=CARTESIAN_POINT('Ctrl Pts',(73.0471841649293,8.43315113900825,-14.6695887137585));
#31486=CARTESIAN_POINT('Ctrl Pts',(73.2899316670396,13.1992567794014,-10.5671940850375));
#31487=CARTESIAN_POINT('Ctrl Pts',(73.5324951429592,16.1378423633534,-5.01067722190336));
#31488=CARTESIAN_POINT('Ctrl Pts',(73.7748792762995,16.8367888818105,1.22864251856273));
#31489=CARTESIAN_POINT('Ctrl Pts',(74.0574511370909,14.9481657499348,8.30419026726172));
#31490=CARTESIAN_POINT('Ctrl Pts',(74.3801042223558,9.25988647762291,14.6764058998477));
#31491=CARTESIAN_POINT('Ctrl Pts',(74.7426760471007,0.0297310386788871,
17.3325017860091));
#31492=CARTESIAN_POINT('Ctrl Pts',(75.104846156915,-9.18512009888459,14.6763349999953));
#31493=CARTESIAN_POINT('Ctrl Pts',(75.4666115601473,-15.5683097019005,7.53105835502853));
#31494=CARTESIAN_POINT('Ctrl Pts',(75.8279755375281,-17.1703047170958,-1.90331404102187));
#31495=CARTESIAN_POINT('Ctrl Pts',(76.188938501318,-13.5089512690439,-10.7361694860703));
#31496=CARTESIAN_POINT('Ctrl Pts',(76.5495030570368,-5.72407492543645,-16.2571081843157));
#31497=CARTESIAN_POINT('Ctrl Pts',(76.9230101424883,4.16106946480652,-16.8182717566536));
#31498=CARTESIAN_POINT('Ctrl Pts',(77.202818264229,10.5808314274358,-12.9982088799238));
#31499=CARTESIAN_POINT('Ctrl Pts',(77.4424552125793,14.3263048597699,-8.16392560339528));
#31500=CARTESIAN_POINT('Ctrl Pts',(77.6287702720463,16.2601131044503,-3.74422807442518));
#31501=CARTESIAN_POINT('Ctrl Pts',(77.8681200492692,16.4905653153525,2.45516469208262));
#31502=CARTESIAN_POINT('Ctrl Pts',(78.1073167318528,14.4438592167683,8.30318709138602));
#31503=CARTESIAN_POINT('Ctrl Pts',(78.3463319999749,10.4036277093244,12.9973204036373));
#31504=CARTESIAN_POINT('Ctrl Pts',(78.5851753685171,4.93332187654749,15.8877883112078));
#31505=CARTESIAN_POINT('Ctrl Pts',(78.8238536783697,-1.2133830481093,16.5809207741654));
#31506=CARTESIAN_POINT('Ctrl Pts',(79.0623433276802,-7.17782048654887,14.9789375723993));
#31507=CARTESIAN_POINT('Ctrl Pts',(79.3271592739995,-12.7064511092803,10.9074960661302));
#31508=CARTESIAN_POINT('Ctrl Pts',(79.5652827398898,-15.6916289014183,5.4178031995205));
#31509=CARTESIAN_POINT('Ctrl Pts',(79.842897654509,-16.577371391909,-1.65388631398067));
#31510=CARTESIAN_POINT('Ctrl Pts',(80.1335376112271,-14.4559690043196,-9.04592183069228));
#31511=CARTESIAN_POINT('Ctrl Pts',(80.4898408484177,-7.41398466215342,-15.3346562519615));
#31512=CARTESIAN_POINT('Ctrl Pts',(80.8457786444577,1.87672500454577,-16.9113054373767));
#31513=CARTESIAN_POINT('Ctrl Pts',(81.2013471369382,10.5769015012641,-13.3072352789264));
#31514=CARTESIAN_POINT('Ctrl Pts',(81.5565536242783,16.0187171293741,-5.63382944603668));
#31515=CARTESIAN_POINT('Ctrl Pts',(81.9114041755206,16.5444635000022,3.74727126004245));
#31516=CARTESIAN_POINT('Ctrl Pts',(82.2658984013975,12.0018869829841,11.9662350574611));
#31517=CARTESIAN_POINT('Ctrl Pts',(82.580705722997,4.7048385127119,15.9911824539821));
#31518=CARTESIAN_POINT('Ctrl Pts',(82.8559194126613,-2.42294966179176,16.2502803669511));
#31519=CARTESIAN_POINT('Ctrl Pts',(83.0916726679261,-8.18711284436968,14.2350674883706));
#31520=CARTESIAN_POINT('Ctrl Pts',(83.3272719462452,-12.8135954548322,10.2519305382705));
#31521=CARTESIAN_POINT('Ctrl Pts',(83.5627180336617,-15.6648270622522,4.85970543368255));
#31522=CARTESIAN_POINT('Ctrl Pts',(83.7980160722245,-16.3455482298039,-1.19867931322076));
#31523=CARTESIAN_POINT('Ctrl Pts',(84.0331762295264,-14.7685260231452,-7.08329288367993));
#31524=CARTESIAN_POINT('Ctrl Pts',(84.268196402248,-11.152406439379,-11.9821788257332));
#31525=CARTESIAN_POINT('Ctrl Pts',(84.5030544855061,-6.00074180238162,-15.220102481595));
#31526=CARTESIAN_POINT('Ctrl Pts',(84.7377942906585,-0.0247637862782051,
-16.349923638104));
#31527=CARTESIAN_POINT('Ctrl Pts',(84.9723852268477,5.94701813960035,-15.2197727933618));
#31528=CARTESIAN_POINT('Ctrl Pts',(85.2068382906793,11.0899618363975,-11.9877327276318));
#31529=CARTESIAN_POINT('Ctrl Pts',(85.4411634196362,14.69529952864,-7.10303215385319));
#31530=CARTESIAN_POINT('Ctrl Pts',(85.6753317373745,16.2641505061611,-1.24258983811037));
#31531=CARTESIAN_POINT('Ctrl Pts',(85.9093834453529,15.585023498085,4.78327339443017));
#31532=CARTESIAN_POINT('Ctrl Pts',(86.1433022075475,12.753189678752,10.1407102289761));
#31533=CARTESIAN_POINT('Ctrl Pts',(86.3770904163802,8.16161557939224,14.092613988289));
#31534=CARTESIAN_POINT('Ctrl Pts',(86.6107514938686,2.44850143153797,16.0892442032996));
#31535=CARTESIAN_POINT('Ctrl Pts',(86.8832033492737,-4.60774973811352,15.8319258548194));
#31536=CARTESIAN_POINT('Ctrl Pts',(87.1943932596932,-11.8200353832729,11.8513593361907));
#31537=CARTESIAN_POINT('Ctrl Pts',(87.5441993244538,-16.3001894463018,3.74019158563494));
#31538=CARTESIAN_POINT('Ctrl Pts',(87.8937391620268,-15.7805135997167,-5.50056638327167));
#31539=CARTESIAN_POINT('Ctrl Pts',(88.2430281368494,-10.4265102210085,-13.0439396213998));
#31540=CARTESIAN_POINT('Ctrl Pts',(88.5920456840267,-1.88797983749057,-16.5806798110945));
#31541=CARTESIAN_POINT('Ctrl Pts',(88.9408683355879,7.22126413171238,-15.0304223652045));
#31542=CARTESIAN_POINT('Ctrl Pts',(89.2312672507147,12.9500498613897,-9.90768422321171));
#31543=CARTESIAN_POINT('Ctrl Pts',(89.4636241947003,15.3843347561836,-4.4396343063962));
#31544=CARTESIAN_POINT('Ctrl Pts',(89.579568951633,15.7989939693362,-1.52285979480461));
#31545=CARTESIAN_POINT('Ctrl Pts',(89.6377374019334,15.8017871959225,-0.016379644123816));
#31546=CARTESIAN_POINT('Ctrl Pts',(69.4240531709196,17.1884297818141,-0.0220473507209931));
#31547=CARTESIAN_POINT('Ctrl Pts',(69.4870264995728,17.1854058267664,1.60887232745941));
#31548=CARTESIAN_POINT('Ctrl Pts',(69.6133825166773,16.7336094867537,4.78766921575342));
#31549=CARTESIAN_POINT('Ctrl Pts',(69.8655902618346,14.0901641326339,10.722743766396));
#31550=CARTESIAN_POINT('Ctrl Pts',(70.1808991871154,7.87082916461279,16.2850634142074));
#31551=CARTESIAN_POINT('Ctrl Pts',(70.5588258651904,-2.00097801197751,17.9608997165613));
#31552=CARTESIAN_POINT('Ctrl Pts',(70.9364976647261,-11.2379749124772,14.1333434106797));
#31553=CARTESIAN_POINT('Ctrl Pts',(71.3138189090291,-17.022765187301,5.98116984148052));
#31554=CARTESIAN_POINT('Ctrl Pts',(71.6279973568013,-17.4821577443558,-2.32283482661027));
#31555=CARTESIAN_POINT('Ctrl Pts',(71.8791587044794,-15.1710757913127,-8.35466252474748));
#31556=CARTESIAN_POINT('Ctrl Pts',(72.0674480802091,-12.2623824355508,-12.2232151758295));
#31557=CARTESIAN_POINT('Ctrl Pts',(72.2556517362955,-8.39465033453757,-15.1321399832916));
#31558=CARTESIAN_POINT('Ctrl Pts',(72.4646714233985,-3.37434570819596,-17.0498317563071));
#31559=CARTESIAN_POINT('Ctrl Pts',(72.6944730924827,2.57520497582538,-17.2731773805752));
#31560=CARTESIAN_POINT('Ctrl Pts',(72.9450091193642,8.70245453300236,-15.1282047436106));
#31561=CARTESIAN_POINT('Ctrl Pts',(73.1953872307492,13.6184515692381,-10.8968875890289));
#31562=CARTESIAN_POINT('Ctrl Pts',(73.4456025501822,16.6498267526876,-5.16509270015882));
#31563=CARTESIAN_POINT('Ctrl Pts',(73.6956575744498,17.3709549472363,1.27172072423803));
#31564=CARTESIAN_POINT('Ctrl Pts',(73.9871985164346,15.4224581181395,8.57192585469278));
#31565=CARTESIAN_POINT('Ctrl Pts',(74.3201228056949,9.55312842944366,15.147214623983));
#31566=CARTESIAN_POINT('Ctrl Pts',(74.694282229127,0.0278963775676262,17.8884110165378));
#31567=CARTESIAN_POINT('Ctrl Pts',(75.0680626554788,-9.48257511274735,15.1471822094838));
#31568=CARTESIAN_POINT('Ctrl Pts',(75.4414566077462,-16.0711692555847,7.77218199232533));
#31569=CARTESIAN_POINT('Ctrl Pts',(75.8144609438332,-17.7249238578617,-1.96628250261766));
#31570=CARTESIAN_POINT('Ctrl Pts',(76.1870708489347,-13.9454473073086,-11.0843892045722));
#31571=CARTESIAN_POINT('Ctrl Pts',(76.5592825554438,-5.90895378486479,-16.7838920968456));
#31572=CARTESIAN_POINT('Ctrl Pts',(76.944862466462,4.29597064015474,-17.3632704575972));
#31573=CARTESIAN_POINT('Ctrl Pts',(77.233714179634,10.9234377023668,-13.419633731763));
#31574=CARTESIAN_POINT('Ctrl Pts',(77.481110180057,14.7902150666366,-8.42881512726714));
#31575=CARTESIAN_POINT('Ctrl Pts',(77.6734420678579,16.786574081098,-3.86622860214854));
#31576=CARTESIAN_POINT('Ctrl Pts',(77.9205334101491,17.0245270944407,2.53374212629342));
#31577=CARTESIAN_POINT('Ctrl Pts',(78.1674468691423,14.9117140996151,8.57064368391211));
#31578=CARTESIAN_POINT('Ctrl Pts',(78.4141712309578,10.7410900027972,13.4163330220923));
#31579=CARTESIAN_POINT('Ctrl Pts',(78.6607089908048,5.09438525439352,16.3999664439789));
#31580=CARTESIAN_POINT('Ctrl Pts',(78.907060486491,-1.2501642558568,17.115417594678));
#31581=CARTESIAN_POINT('Ctrl Pts',(79.1532182906523,-7.40645575193075,15.4618484055836));
#31582=CARTESIAN_POINT('Ctrl Pts',(79.4265206417368,-13.1124389073509,11.2597518864601));
#31583=CARTESIAN_POINT('Ctrl Pts',(79.6722671305222,-16.1931862086824,5.59418186052905));
#31584=CARTESIAN_POINT('Ctrl Pts',(79.9587481865963,-17.107208902634,-1.70351483576795));
#31585=CARTESIAN_POINT('Ctrl Pts',(80.2586234108375,-14.9181543555872,-9.33083857880673));
#31586=CARTESIAN_POINT('Ctrl Pts',(80.6262139427276,-7.65267738846512,-15.8189271434239));
#31587=CARTESIAN_POINT('Ctrl Pts',(80.993369645609,1.93135544061078,-17.4451185003386));
#31588=CARTESIAN_POINT('Ctrl Pts',(81.3600870123395,10.9046720730943,-13.7276751808303));
#31589=CARTESIAN_POINT('Ctrl Pts',(81.7263654465945,16.516198667685,-5.81456179905747));
#31590=CARTESIAN_POINT('Ctrl Pts',(82.0922035782066,17.058047794173,3.85756185847759));
#31591=CARTESIAN_POINT('Ctrl Pts',(82.4575998851323,12.3753093119527,12.3295869826222));
#31592=CARTESIAN_POINT('Ctrl Pts',(82.7820047281608,4.85519133781646,16.4773647557847));
#31593=CARTESIAN_POINT('Ctrl Pts',(83.06556961557,-2.48914093741938,16.7442492288014));
#31594=CARTESIAN_POINT('Ctrl Pts',(83.3084289758973,-8.42735448041435,14.6681468183089));
#31595=CARTESIAN_POINT('Ctrl Pts',(83.5510909458127,-13.1926413221872,10.5653533262531));
#31596=CARTESIAN_POINT('Ctrl Pts',(83.7935551432849,-16.1289593487553,5.01216886238094));
#31597=CARTESIAN_POINT('Ctrl Pts',(84.0358223101127,-16.8297188132406,-1.22589245673049));
#31598=CARTESIAN_POINT('Ctrl Pts',(84.2778927289577,-15.2062416115988,-7.28372473114384));
#31599=CARTESIAN_POINT('Ctrl Pts',(84.519766488978,-11.484320451343,-12.3256879562995));
#31600=CARTESIAN_POINT('Ctrl Pts',(84.761441837939,-6.18293902347355,-15.6576372355493));
#31601=CARTESIAN_POINT('Ctrl Pts',(85.0029217884757,-0.0349046563979193,
-16.8198288925798));
#31602=CARTESIAN_POINT('Ctrl Pts',(85.2442044100241,6.10753989381876,-15.6573076159067));
#31603=CARTESIAN_POINT('Ctrl Pts',(85.4852907630462,11.3961830117023,-12.3334882012418));
#31604=CARTESIAN_POINT('Ctrl Pts',(85.726181088518,15.1027170540795,-7.31150778152954));
#31605=CARTESIAN_POINT('Ctrl Pts',(85.966875037897,16.7151551608915,-1.28752411788782));
#31606=CARTESIAN_POINT('Ctrl Pts',(86.2073738077064,16.0171614768628,4.90467811860692));
#31607=CARTESIAN_POINT('Ctrl Pts',(86.447677494623,13.1077224596251,10.4085994658324));
#31608=CARTESIAN_POINT('Ctrl Pts',(86.6877865663515,8.39163183364423,14.4674371565703));
#31609=CARTESIAN_POINT('Ctrl Pts',(86.9277014259927,2.52521683523347,16.5174726601838));
#31610=CARTESIAN_POINT('Ctrl Pts',(87.2073764041283,-4.71846893122861,16.2531082314488));
#31611=CARTESIAN_POINT('Ctrl Pts',(87.5266824785365,-12.119252917514,12.1679209131024));
#31612=CARTESIAN_POINT('Ctrl Pts',(87.8854707031164,-16.7142851347075,3.84758826535438));
#31613=CARTESIAN_POINT('Ctrl Pts',(88.2438268345246,-16.1808605256974,-5.62684461281575));
#31614=CARTESIAN_POINT('Ctrl Pts',(88.6017596804731,-10.6935017851311,-13.3572996474587));
#31615=CARTESIAN_POINT('Ctrl Pts',(88.9592581284196,-1.94684933313455,-16.9793506731735));
#31616=CARTESIAN_POINT('Ctrl Pts',(89.3163558666232,7.37927353005637,-15.3920445435929));
#31617=CARTESIAN_POINT('Ctrl Pts',(89.6135475815425,13.2414270899268,-10.148282449374));
#31618=CARTESIAN_POINT('Ctrl Pts',(89.8511629514236,15.7308559147538,-4.55632603911814));
#31619=CARTESIAN_POINT('Ctrl Pts',(89.9698142754425,16.1550130455499,-1.57126098134776));
#31620=CARTESIAN_POINT('Ctrl Pts',(90.029242413098,16.157866761838,-0.0321567193703245));
#31621=CARTESIAN_POINT('Ctrl Pts',(68.6597607285732,17.4006280941266,0.00785707557859578));
#31622=CARTESIAN_POINT('Ctrl Pts',(68.7235009699529,17.3975673122243,1.65863870299843));
#31623=CARTESIAN_POINT('Ctrl Pts',(68.8514963705168,16.9400695695691,4.87883884057858));
#31624=CARTESIAN_POINT('Ctrl Pts',(69.1069562397825,14.262686949915,10.8906064157376));
#31625=CARTESIAN_POINT('Ctrl Pts',(69.4266395295462,7.95798755464706,16.5315448855194));
#31626=CARTESIAN_POINT('Ctrl Pts',(69.8101364767553,-2.05974367394959,18.2332011185647));
#31627=CARTESIAN_POINT('Ctrl Pts',(70.1937597880174,-11.4432175552833,14.3466336126088));
#31628=CARTESIAN_POINT('Ctrl Pts',(70.5773880629489,-17.3260775571641,6.0584389009168));
#31629=CARTESIAN_POINT('Ctrl Pts',(70.8971087240495,-17.7947199866996,-2.39254166927833));
#31630=CARTESIAN_POINT('Ctrl Pts',(71.1529016677111,-15.441149366048,-8.53590454680965));
#31631=CARTESIAN_POINT('Ctrl Pts',(71.3447498253948,-12.4775139902205,-12.4777911778366));
#31632=CARTESIAN_POINT('Ctrl Pts',(71.5365993719199,-8.53482928977716,-15.4433197010116));
#31633=CARTESIAN_POINT('Ctrl Pts',(71.7497680377377,-3.41478972728435,-17.3993154029907));
#31634=CARTESIAN_POINT('Ctrl Pts',(71.9842483873757,2.65613898428773,-17.6275734717924));
#31635=CARTESIAN_POINT('Ctrl Pts',(72.2400436052835,8.91240965773181,-15.4378542921431));
#31636=CARTESIAN_POINT('Ctrl Pts',(72.4958333516622,13.9350486173369,-11.1151391614399));
#31637=CARTESIAN_POINT('Ctrl Pts',(72.7516190270194,17.0343485207352,-5.2557825150929));
#31638=CARTESIAN_POINT('Ctrl Pts',(73.0073922590926,17.7722806554582,1.32842090373711));
#31639=CARTESIAN_POINT('Ctrl Pts',(73.3057778782715,15.7784440622631,8.80031303306672));
#31640=CARTESIAN_POINT('Ctrl Pts',(73.6467483653377,9.76765350955319,15.5355999090755));
#31641=CARTESIAN_POINT('Ctrl Pts',(74.0303001928062,0.00324086649956546,
18.3469216573022));
#31642=CARTESIAN_POINT('Ctrl Pts',(74.4137917659782,-9.75515672015961,15.5354418730925));
#31643=CARTESIAN_POINT('Ctrl Pts',(74.7972167116253,-16.5219402379097,7.9627758146546));
#31644=CARTESIAN_POINT('Ctrl Pts',(75.1805634519762,-18.2228041626385,-2.04597779745445));
#31645=CARTESIAN_POINT('Ctrl Pts',(75.5638233687855,-14.3362306118562,-11.4255797117487));
#31646=CARTESIAN_POINT('Ctrl Pts',(75.9469859200462,-6.0636041500258,-17.293973869085));
#31647=CARTESIAN_POINT('Ctrl Pts',(76.3442286759065,4.45035809519592,-17.8921316341132));
#31648=CARTESIAN_POINT('Ctrl Pts',(76.6420630145241,11.2847744272317,-13.8265238405078));
#31649=CARTESIAN_POINT('Ctrl Pts',(76.8973083073728,15.2743398861069,-8.67734593552654));
#31650=CARTESIAN_POINT('Ctrl Pts',(77.0957897594511,17.3348436194496,-3.96875396903001));
#31651=CARTESIAN_POINT('Ctrl Pts',(77.3509344220687,17.5809444731262,2.63986365468201));
#31652=CARTESIAN_POINT('Ctrl Pts',(77.6060046004046,15.3984975693097,8.87656313529381));
#31653=CARTESIAN_POINT('Ctrl Pts',(77.8610143191004,11.0879602445291,13.8853489397089));
#31654=CARTESIAN_POINT('Ctrl Pts',(78.1159555466501,5.24871190651801,16.9710023515976));
#31655=CARTESIAN_POINT('Ctrl Pts',(78.3708228158246,-1.31537487006328,17.7115205686433));
#31656=CARTESIAN_POINT('Ctrl Pts',(78.6256256627463,-7.68805341091284,16.000075751367));
#31657=CARTESIAN_POINT('Ctrl Pts',(78.9086472803925,-13.5973264027015,11.6486643509849));
#31658=CARTESIAN_POINT('Ctrl Pts',(79.1632815997527,-16.7899751467946,5.77830465705051));
#31659=CARTESIAN_POINT('Ctrl Pts',(79.4602587190341,-17.7376470533284,-1.78688963502401));
#31660=CARTESIAN_POINT('Ctrl Pts',(79.7712540029704,-15.4679962299785,-9.69759166027641));
#31661=CARTESIAN_POINT('Ctrl Pts',(80.1527404854897,-7.92824878930432,-16.4318552784184));
#31662=CARTESIAN_POINT('Ctrl Pts',(80.5340186637714,2.02466878417038,-18.1214851807052));
#31663=CARTESIAN_POINT('Ctrl Pts',(80.9150837007837,11.3496854121677,-14.2592766110511));
#31664=CARTESIAN_POINT('Ctrl Pts',(81.2959255170471,17.1852011053556,-6.03175011440449));
#31665=CARTESIAN_POINT('Ctrl Pts',(81.6765347527869,17.7497716308165,4.03117053838598));
#31666=CARTESIAN_POINT('Ctrl Pts',(82.0569046689732,12.8757070820106,12.8510081252502));
#31667=CARTESIAN_POINT('Ctrl Pts',(82.3947862972429,5.04321613190222,17.1718637553676));
#31668=CARTESIAN_POINT('Ctrl Pts',(82.6902738480198,-2.61005988977363,17.4502374567792));
#31669=CARTESIAN_POINT('Ctrl Pts',(82.9434300076959,-8.80025952764612,15.2862649770185));
#31670=CARTESIAN_POINT('Ctrl Pts',(83.1964687178264,-13.7695371664239,11.0080918574343));
#31671=CARTESIAN_POINT('Ctrl Pts',(83.4493880807088,-16.8327170478229,5.21547004081706));
#31672=CARTESIAN_POINT('Ctrl Pts',(83.7021843180637,-17.5641109077076,-1.29378561473781));
#31673=CARTESIAN_POINT('Ctrl Pts',(83.9548528665527,-15.8697255170729,-7.61700457494452));
#31674=CARTESIAN_POINT('Ctrl Pts',(84.2073923691056,-11.9837143457694,-12.8815110092968));
#31675=CARTESIAN_POINT('Ctrl Pts',(84.4598079448926,-6.44679302894026,-16.3617271312645));
#31676=CARTESIAN_POINT('Ctrl Pts',(84.7120847855581,-0.0237395979090416,
-17.5760510646781));
#31677=CARTESIAN_POINT('Ctrl Pts',(84.9642303272761,6.39538656732633,-16.3613398560058));
#31678=CARTESIAN_POINT('Ctrl Pts',(85.2162395408117,11.9238107247879,-12.886977573222));
#31679=CARTESIAN_POINT('Ctrl Pts',(85.4681084387409,15.7994707310197,-7.63609786493631));
#31680=CARTESIAN_POINT('Ctrl Pts',(85.719842902167,17.486012423623,-1.33577274741051));
#31681=CARTESIAN_POINT('Ctrl Pts',(85.9714309934085,16.7559602965917,5.14206670856116));
#31682=CARTESIAN_POINT('Ctrl Pts',(86.2228753368623,13.7117014917251,10.9012971452895));
#31683=CARTESIAN_POINT('Ctrl Pts',(86.4741737949277,8.77584705906915,15.1494265813195));
#31684=CARTESIAN_POINT('Ctrl Pts',(86.7253242351102,2.63465796664165,17.2956018092232));
#31685=CARTESIAN_POINT('Ctrl Pts',(87.0181593012597,-4.94995751639123,17.0189226482735));
#31686=CARTESIAN_POINT('Ctrl Pts',(87.3525707654822,-12.7010842904221,12.7407348698173));
#31687=CARTESIAN_POINT('Ctrl Pts',(87.728436564811,-17.5152394101686,4.0243596939246));
#31688=CARTESIAN_POINT('Ctrl Pts',(88.1039527740728,-16.9565472756951,-5.90364377027598));
#31689=CARTESIAN_POINT('Ctrl Pts',(88.4791004609346,-11.2053993769732,-14.006553928488));
#31690=CARTESIAN_POINT('Ctrl Pts',(88.8539049876026,-2.035744278159,-17.8033917672818));
#31691=CARTESIAN_POINT('Ctrl Pts',(89.2282904122505,7.74277152007772,-16.1403772233317));
#31692=CARTESIAN_POINT('Ctrl Pts',(89.5400581478773,13.8914564051538,-10.6388851155824));
#31693=CARTESIAN_POINT('Ctrl Pts',(89.7891264886643,16.5013623504881,-4.77745809816874));
#31694=CARTESIAN_POINT('Ctrl Pts',(89.9137512217624,16.946855069725,-1.64209065688647));
#31695=CARTESIAN_POINT('Ctrl Pts',(89.97593701968,16.9498412077971,-0.0315669153498612));
#31696=CARTESIAN_POINT('Ctrl Pts',(68.014332389863,16.9368226517689,0.0319184960226097));
#31697=CARTESIAN_POINT('Ctrl Pts',(68.0764705480552,16.9338388012858,1.64120844668688));
#31698=CARTESIAN_POINT('Ctrl Pts',(68.2009984722761,16.4886744022683,4.77406298181688));
#31699=CARTESIAN_POINT('Ctrl Pts',(68.4498749428734,13.8807131815627,10.6308858370252));
#31700=CARTESIAN_POINT('Ctrl Pts',(68.761416689418,7.73692033746066,16.128273198334));
#31701=CARTESIAN_POINT('Ctrl Pts',(69.1355280034991,-2.03476959494914,17.7898195120724));
#31702=CARTESIAN_POINT('Ctrl Pts',(69.5100668032795,-11.1962298165234,13.9962376482653));
#31703=CARTESIAN_POINT('Ctrl Pts',(69.8849504935975,-16.945783170327,5.89821129851622));
#31704=CARTESIAN_POINT('Ctrl Pts',(70.1976715900557,-17.4051344806488,-2.36731702515499));
#31705=CARTESIAN_POINT('Ctrl Pts',(70.4480172764557,-15.101928416316,-8.3797986420383));
#31706=CARTESIAN_POINT('Ctrl Pts',(70.6358677465942,-12.2002491246392,-12.2395111621439));
#31707=CARTESIAN_POINT('Ctrl Pts',(70.8238060359331,-8.33813940883176,-15.1446030697862));
#31708=CARTESIAN_POINT('Ctrl Pts',(71.0327237000049,-3.3204037438702,-17.0616804506108));
#31709=CARTESIAN_POINT('Ctrl Pts',(71.2626597523326,2.63261163312919,-17.2858315776882));
#31710=CARTESIAN_POINT('Ctrl Pts',(71.5136511052112,8.7712694878663,-15.1376581309978));
#31711=CARTESIAN_POINT('Ctrl Pts',(71.7647927622528,13.7027463103588,-10.8939740892587));
#31712=CARTESIAN_POINT('Ctrl Pts',(72.0160805068755,16.7477786072646,-5.13797793175056));
#31713=CARTESIAN_POINT('Ctrl Pts',(72.2675155482385,17.4736046987134,1.33432392506951));
#31714=CARTESIAN_POINT('Ctrl Pts',(72.5610257212911,15.5128311991003,8.68399749862113));
#31715=CARTESIAN_POINT('Ctrl Pts',(72.8967121588295,9.59650585111651,15.3152930648782));
#31716=CARTESIAN_POINT('Ctrl Pts',(73.274669438999,-0.0246868277003993,
18.0868136163285));
#31717=CARTESIAN_POINT('Ctrl Pts',(73.6529358009447,-9.65000244600368,15.315138165857));
#31718=CARTESIAN_POINT('Ctrl Pts',(74.0315016957638,-16.331744326295,7.8397084676337));
#31719=CARTESIAN_POINT('Ctrl Pts',(74.4103614589508,-18.0139710668216,-2.05116003639906));
#31720=CARTESIAN_POINT('Ctrl Pts',(74.7895076049163,-14.170564539168,-11.3301737685776));
#31721=CARTESIAN_POINT('Ctrl Pts',(75.1689333581195,-5.97980433672152,-17.1421185404384));
#31722=CARTESIAN_POINT('Ctrl Pts',(75.5626937216784,4.44136041994808,-17.7365097499734));
#31723=CARTESIAN_POINT('Ctrl Pts',(75.8582312621752,11.2233892267941,-13.7036013137413));
#31724=CARTESIAN_POINT('Ctrl Pts',(76.1116496313081,15.1844323227741,-8.59128840354336));
#31725=CARTESIAN_POINT('Ctrl Pts',(76.3088229628224,17.2314721741726,-3.91415213897931));
#31726=CARTESIAN_POINT('Ctrl Pts',(76.5624281235002,17.4764311383519,2.65449037292804));
#31727=CARTESIAN_POINT('Ctrl Pts',(76.816152542962,15.3060174966826,8.85808296957702));
#31728=CARTESIAN_POINT('Ctrl Pts',(77.0699772467878,11.0159391984402,13.8436381261701));
#31729=CARTESIAN_POINT('Ctrl Pts',(77.3239049175782,5.20035674827198,16.9173023230172));
#31730=CARTESIAN_POINT('Ctrl Pts',(77.577936234861,-1.34181378896731,17.6557574765637));
#31731=CARTESIAN_POINT('Ctrl Pts',(77.8320552996849,-7.69737922244923,15.9493639766937));
#31732=CARTESIAN_POINT('Ctrl Pts',(78.1145243916325,-13.5951231236606,11.6070912487124));
#31733=CARTESIAN_POINT('Ctrl Pts',(78.3688471472273,-16.7844178817442,5.74438589068073));
#31734=CARTESIAN_POINT('Ctrl Pts',(78.6656608116319,-17.7318026091762,-1.81641343765658));
#31735=CARTESIAN_POINT('Ctrl Pts',(78.9767385896377,-15.462822425123,-9.72895758703099));
#31736=CARTESIAN_POINT('Ctrl Pts',(79.3586932597966,-7.91515306456073,-16.4722820318529));
#31737=CARTESIAN_POINT('Ctrl Pts',(79.7408288150502,2.05935680779579,-18.1670862463568));
#31738=CARTESIAN_POINT('Ctrl Pts',(80.1231324309674,11.4147636910949,-14.2938551204881));
#31739=CARTESIAN_POINT('Ctrl Pts',(80.5055971190963,17.2760338856779,-6.03251997755934));
#31740=CARTESIAN_POINT('Ctrl Pts',(80.8882139858091,17.844936685304,4.08285450666647));
#31741=CARTESIAN_POINT('Ctrl Pts',(81.2709714329646,12.9417717016896,12.9583263956821));
#31742=CARTESIAN_POINT('Ctrl Pts',(81.6113241079054,5.05304097073616,17.3115655713565));
#31743=CARTESIAN_POINT('Ctrl Pts',(81.9092036538918,-2.66196224769219,17.5926673075212));
#31744=CARTESIAN_POINT('Ctrl Pts',(82.1645848689637,-8.90638889298226,15.4101212359073));
#31745=CARTESIAN_POINT('Ctrl Pts',(82.4200136325472,-13.9227166542397,11.0920226111291));
#31746=CARTESIAN_POINT('Ctrl Pts',(82.6754866039489,-17.0170240494153,5.24127019003033));
#31747=CARTESIAN_POINT('Ctrl Pts',(82.9310030857056,-17.756717250709,-1.33778819487169));
#31748=CARTESIAN_POINT('Ctrl Pts',(83.1865644655235,-16.0433394548369,-7.73323614893282));
#31749=CARTESIAN_POINT('Ctrl Pts',(83.4421661736319,-12.1107655448105,-13.0615834286996));
#31750=CARTESIAN_POINT('Ctrl Pts',(83.6977931804047,-6.50370995420041,-16.586309544005));
#31751=CARTESIAN_POINT('Ctrl Pts',(83.9534640397682,0.00531481089540298,
-17.8173430226054));
#31752=CARTESIAN_POINT('Ctrl Pts',(84.2091594317815,6.5146243017338,-16.5859416183189));
#31753=CARTESIAN_POINT('Ctrl Pts',(84.4648814125953,12.12450727094,-13.0609202293272));
#31754=CARTESIAN_POINT('Ctrl Pts',(84.7206310049753,16.0599935964609,-7.72964432252528));
#31755=CARTESIAN_POINT('Ctrl Pts',(84.9763905740002,17.7738878064829,-1.32882848634198));
#31756=CARTESIAN_POINT('Ctrl Pts',(85.2321758096326,17.03207406858,5.25685256337923));
#31757=CARTESIAN_POINT('Ctrl Pts',(85.4879751575384,13.9355754035496,11.1157872024267));
#31758=CARTESIAN_POINT('Ctrl Pts',(85.7437858116849,8.91155809052332,15.4403568542271));
#31759=CARTESIAN_POINT('Ctrl Pts',(85.9996060974355,2.65654793570823,17.6267315370253));
#31760=CARTESIAN_POINT('Ctrl Pts',(86.2980666948127,-5.07351735129217,17.3452336162104));
#31761=CARTESIAN_POINT('Ctrl Pts',(86.6391833189476,-12.9801532360575,12.9825944194009));
#31762=CARTESIAN_POINT('Ctrl Pts',(87.0229268046549,-17.8961913498233,4.08451505234094));
#31763=CARTESIAN_POINT('Ctrl Pts',(87.4066687860505,-17.3265839015146,-6.0604305607405));
#31764=CARTESIAN_POINT('Ctrl Pts',(87.7903709222829,-11.4455386605879,-14.348712512324));
#31765=CARTESIAN_POINT('Ctrl Pts',(88.1740825929623,-2.05902204053203,-18.2363604026539));
#31766=CARTESIAN_POINT('Ctrl Pts',(88.5576667221726,7.96004300481042,-16.5342363554814));
#31767=CARTESIAN_POINT('Ctrl Pts',(88.8774482190082,14.2667445785016,-10.8921034944438));
#31768=CARTESIAN_POINT('Ctrl Pts',(89.1329596343274,16.9446486652469,-4.87923821628262));
#31769=CARTESIAN_POINT('Ctrl Pts',(89.2609907780456,17.4024388597611,-1.65829899794939));
#31770=CARTESIAN_POINT('Ctrl Pts',(89.3247406611467,17.4055001046014,-0.0072676741977367));
#31771=CARTESIAN_POINT('Ctrl Pts',(67.9785110845474,16.1431896342132,0.0318301264118968));
#31772=CARTESIAN_POINT('Ctrl Pts',(68.0378858846227,16.1403384791252,1.569553030724));
#31773=CARTESIAN_POINT('Ctrl Pts',(68.1564254451454,15.7165770004678,4.55178190463174));
#31774=CARTESIAN_POINT('Ctrl Pts',(68.3938219334874,13.2293798077654,10.1385336217139));
#31775=CARTESIAN_POINT('Ctrl Pts',(68.6907420120926,7.37292663615509,15.3774902252066));
#31776=CARTESIAN_POINT('Ctrl Pts',(69.0475082724276,-1.94493333057598,16.9631236785857));
#31777=CARTESIAN_POINT('Ctrl Pts',(69.4046728281513,-10.6819468555142,13.3449418751655));
#31778=CARTESIAN_POINT('Ctrl Pts',(69.7622677199762,-16.1665520224338,5.62093383043492));
#31779=CARTESIAN_POINT('Ctrl Pts',(70.0606157014478,-16.60504542502,-2.26502246803787));
#31780=CARTESIAN_POINT('Ctrl Pts',(70.2995058763236,-14.4073009182687,-8.00238558857723));
#31781=CARTESIAN_POINT('Ctrl Pts',(70.4787806828198,-11.6380989564286,-11.6859690320109));
#31782=CARTESIAN_POINT('Ctrl Pts',(70.6581631675788,-7.95182529872869,-14.4588656285554));
#31783=CARTESIAN_POINT('Ctrl Pts',(70.8575964721588,-3.16186856987872,-16.2889865245856));
#31784=CARTESIAN_POINT('Ctrl Pts',(71.0771282073065,2.52182904090697,-16.5031150354075));
#31785=CARTESIAN_POINT('Ctrl Pts',(71.3168096314304,8.38398534374628,-14.4518485098465));
#31786=CARTESIAN_POINT('Ctrl Pts',(71.5566843359071,13.0943431381348,-10.3985989843744));
#31787=CARTESIAN_POINT('Ctrl Pts',(71.7967518576259,16.0035661257044,-4.89963928653314));
#31788=CARTESIAN_POINT('Ctrl Pts',(72.0370139613808,16.6972678826331,1.28510323855206));
#31789=CARTESIAN_POINT('Ctrl Pts',(72.3175466529949,14.8233549849365,8.30992155597743));
#31790=CARTESIAN_POINT('Ctrl Pts',(72.6384820627477,9.16722602236474,14.6502440480075));
#31791=CARTESIAN_POINT('Ctrl Pts',(72.9999735466316,-0.034818267257906,
17.301604261126));
#31792=CARTESIAN_POINT('Ctrl Pts',(73.3619064145069,-9.24486652526365,14.6501004295558));
#31793=CARTESIAN_POINT('Ctrl Pts',(73.7242810319573,-15.641416905871,7.49465763351948));
#31794=CARTESIAN_POINT('Ctrl Pts',(74.0870981624789,-17.2530825064288,-1.97749200747249));
#31795=CARTESIAN_POINT('Ctrl Pts',(74.4503580843669,-13.571256654549,-10.8681906954034));
#31796=CARTESIAN_POINT('Ctrl Pts',(74.8140609279404,-5.72011949551101,-16.440006102462));
#31797=CARTESIAN_POINT('Ctrl Pts',(75.1916935457088,4.27441446084024,-17.0108569349597));
#31798=CARTESIAN_POINT('Ctrl Pts',(75.4752811028074,10.7827639267889,-13.1414831702565));
#31799=CARTESIAN_POINT('Ctrl Pts',(75.7185548673632,14.5853175807895,-8.23381412747197));
#31800=CARTESIAN_POINT('Ctrl Pts',(75.907867413484,16.5509807384611,-3.74306843918247));
#31801=CARTESIAN_POINT('Ctrl Pts',(76.1514680483462,16.7865607653339,2.56649192426096));
#31802=CARTESIAN_POINT('Ctrl Pts',(76.3952622907919,14.7012372504299,8.52757133361821));
#31803=CARTESIAN_POINT('Ctrl Pts',(76.6392530801337,10.577484401339,13.3202749579265));
#31804=CARTESIAN_POINT('Ctrl Pts',(76.883439294177,4.98496285112783,16.2762918787137));
#31805=CARTESIAN_POINT('Ctrl Pts',(77.1278192754108,-1.30884007541534,16.9869922345478));
#31806=CARTESIAN_POINT('Ctrl Pts',(77.3723966666688,-7.42591453522203,15.3448479448429));
#31807=CARTESIAN_POINT('Ctrl Pts',(77.6443621377783,-13.1046908653612,11.1641662681244));
#31808=CARTESIAN_POINT('Ctrl Pts',(77.8893591794915,-16.1774889930477,5.51654176568881));
#31809=CARTESIAN_POINT('Ctrl Pts',(78.1754139623,-17.0906981982566,-1.7703111468904));
#31810=CARTESIAN_POINT('Ctrl Pts',(78.4753399201003,-14.9036520345214,-9.39974734360126));
#31811=CARTESIAN_POINT('Ctrl Pts',(78.8438648610653,-7.62177045923067,-15.9069310852974));
#31812=CARTESIAN_POINT('Ctrl Pts',(79.2128171384923,2.00889070682572,-17.5442570054289));
#31813=CARTESIAN_POINT('Ctrl Pts',(79.5821956018624,11.0487422668153,-13.8027572119352));
#31814=CARTESIAN_POINT('Ctrl Pts',(79.9519969108647,16.7170242555458,-5.81521116669086));
#31815=CARTESIAN_POINT('Ctrl Pts',(80.3222172565172,17.2685968035139,3.97281760370441));
#31816=CARTESIAN_POINT('Ctrl Pts',(80.6928547291618,12.5214581392903,12.5681324652044));
#31817=CARTESIAN_POINT('Ctrl Pts',(81.0226741018505,4.87690503480926,16.7877757436989));
#31818=CARTESIAN_POINT('Ctrl Pts',(81.3115367942124,-2.60480142711277,17.0607827981659));
#31819=CARTESIAN_POINT('Ctrl Pts',(81.5593120712615,-8.66362909419818,14.943484187758));
#31820=CARTESIAN_POINT('Ctrl Pts',(81.8072681247254,-13.5335698559155,10.7518132776484));
#31821=CARTESIAN_POINT('Ctrl Pts',(82.0554037496435,-16.5394462539352,5.06910782949574));
#31822=CARTESIAN_POINT('Ctrl Pts',(82.3037169758971,-17.2586053337516,-1.32463910810424));
#31823=CARTESIAN_POINT('Ctrl Pts',(82.5522036597656,-15.5929741482425,-7.54339860049728));
#31824=CARTESIAN_POINT('Ctrl Pts',(82.8008637977723,-11.7672571729509,-12.7274796411849));
#31825=CARTESIAN_POINT('Ctrl Pts',(83.0497030317913,-6.30918200043825,-16.1590093563318));
#31826=CARTESIAN_POINT('Ctrl Pts',(83.2987071571274,0.030423146966114,-17.3583257425452));
#31827=CARTESIAN_POINT('Ctrl Pts',(83.5478845422533,6.37414250483962,-16.1586487421449));
#31828=CARTESIAN_POINT('Ctrl Pts',(83.7972310681378,11.8445640374261,-12.7216220956902));
#31829=CARTESIAN_POINT('Ctrl Pts',(84.0467422766515,15.6845723764937,-7.52032796424948));
#31830=CARTESIAN_POINT('Ctrl Pts',(84.2964270384935,17.3581049205115,-1.27147299465656));
#31831=CARTESIAN_POINT('Ctrl Pts',(84.5462707233275,16.6338652686637,5.16156858897617));
#31832=CARTESIAN_POINT('Ctrl Pts',(84.7962779718032,13.6076521978334,10.8882602246653));
#31833=CARTESIAN_POINT('Ctrl Pts',(85.0464468759817,8.69445958734289,15.1178971036121));
#31834=CARTESIAN_POINT('Ctrl Pts',(85.2967753376485,2.57355346225438,17.2577590241979));
#31835=CARTESIAN_POINT('Ctrl Pts',(85.5890114258584,-4.99555256481923,16.982557096495));
#31836=CARTESIAN_POINT('Ctrl Pts',(85.9232482985609,-12.7437747387513,12.7085701664197));
#31837=CARTESIAN_POINT('Ctrl Pts',(86.2996124177631,-17.5666805845105,3.98182266229514));
#31838=CARTESIAN_POINT('Ctrl Pts',(86.6763192307827,-17.0088110427856,-5.97792722908082));
#31839=CARTESIAN_POINT('Ctrl Pts',(87.0533497486091,-11.2308662184509,-14.1231298760299));
#31840=CARTESIAN_POINT('Ctrl Pts',(87.4307284834426,-1.99915391505435,-17.9484835097794));
#31841=CARTESIAN_POINT('Ctrl Pts',(87.8083766725088,7.86516832083256,-16.2735894236369));
#31842=CARTESIAN_POINT('Ctrl Pts',(88.1234384738727,14.0802153362982,-10.7153937271007));
#31843=CARTESIAN_POINT('Ctrl Pts',(88.3754809575467,16.721833883369,-4.78406246384038));
#31844=CARTESIAN_POINT('Ctrl Pts',(88.50174380989,17.173221591803,-1.60746207645487));
#31845=CARTESIAN_POINT('Ctrl Pts',(88.5646803557127,17.1762437805005,0.0225049683035558));
#31846=CARTESIAN_POINT('Ctrl Pts',(68.5732254931795,15.6164607114294,0.00789028987868486));
#31847=CARTESIAN_POINT('Ctrl Pts',(68.6307543287869,15.613698198846,1.49780533901795));
#31848=CARTESIAN_POINT('Ctrl Pts',(68.7452888582432,15.2043138900613,4.37940633245871));
#31849=CARTESIAN_POINT('Ctrl Pts',(68.9749441538233,12.7983847167288,9.78409544822882));
#31850=CARTESIAN_POINT('Ctrl Pts',(69.2617618377016,7.13956805019415,14.844065966187));
#31851=CARTESIAN_POINT('Ctrl Pts',(69.6062737406281,-1.85807669057325,16.3750371655707));
#31852=CARTESIAN_POINT('Ctrl Pts',(69.9508498703511,-10.2875139219393,12.88262556287));
#31853=CARTESIAN_POINT('Ctrl Pts',(70.2956244517574,-15.5748451070192,5.43501177969178));
#31854=CARTESIAN_POINT('Ctrl Pts',(70.5830503952178,-15.9965254225249,-2.16296862263973));
#31855=CARTESIAN_POINT('Ctrl Pts',(70.8130992683074,-13.8799527336818,-7.68799620388367));
#31856=CARTESIAN_POINT('Ctrl Pts',(70.9856768912645,-11.2140225776427,-11.2340383430839));
#31857=CARTESIAN_POINT('Ctrl Pts',(71.1583013094849,-7.66647800099633,-13.9024562467762));
#31858=CARTESIAN_POINT('Ctrl Pts',(71.3501585789615,-3.05831667813383,-15.6630039154817));
#31859=CARTESIAN_POINT('Ctrl Pts',(71.5612650719921,2.40745597291645,-15.8686977749241));
#31860=CARTESIAN_POINT('Ctrl Pts',(71.79165252113,8.04240760846629,-13.896683013927));
#31861=CARTESIAN_POINT('Ctrl Pts',(72.0221311730022,12.5682094894439,-10.0018632134027));
#31862=CARTESIAN_POINT('Ctrl Pts',(72.2527081604281,15.3622886786739,-4.72008117234861));
#31863=CARTESIAN_POINT('Ctrl Pts',(72.4833799691409,16.0280497202866,1.21795506808586));
#31864=CARTESIAN_POINT('Ctrl Pts',(72.7526121354263,14.229337115007,7.95988872480797));
#31865=CARTESIAN_POINT('Ctrl Pts',(73.0604623958875,8.80304371259818,14.0415174266253));
#31866=CARTESIAN_POINT('Ctrl Pts',(73.4070369783453,-0.0197241229505961,
16.5828396759277));
#31867=CARTESIAN_POINT('Ctrl Pts',(73.7538537051601,-8.84521045017838,14.0413090669527));
#31868=CARTESIAN_POINT('Ctrl Pts',(74.1009242982494,-14.9712897991147,7.18743784651643));
#31869=CARTESIAN_POINT('Ctrl Pts',(74.4482544704108,-16.5135836921132,-1.88073950663067));
#31870=CARTESIAN_POINT('Ctrl Pts',(74.7958523761652,-12.9898701817829,-10.3880820430838));
#31871=CARTESIAN_POINT('Ctrl Pts',(75.1437249277752,-5.479968520301,-15.7170578917619));
#31872=CARTESIAN_POINT('Ctrl Pts',(75.5047745491095,4.07591305069949,-16.2622748769602));
#31873=CARTESIAN_POINT('Ctrl Pts',(75.775799333639,10.2958255109986,-12.5638294058234));
#31874=CARTESIAN_POINT('Ctrl Pts',(76.0082498170727,13.9291885586121,-7.8745029993023));
#31875=CARTESIAN_POINT('Ctrl Pts',(76.1891039657334,15.8069677171505,-3.58426467255911));
#31876=CARTESIAN_POINT('Ctrl Pts',(76.4217770053772,16.0318674553836,2.44227285229655));
#31877=CARTESIAN_POINT('Ctrl Pts',(76.6545783736397,14.040403264277,8.13460446657749));
#31878=CARTESIAN_POINT('Ctrl Pts',(76.8875232761733,10.1032200457297,12.7102945419314));
#31879=CARTESIAN_POINT('Ctrl Pts',(77.1206092391391,4.76480431332326,15.5318472041218));
#31880=CARTESIAN_POINT('Ctrl Pts',(77.3538369474926,-1.2418588919811,16.2099981882822));
#31881=CARTESIAN_POINT('Ctrl Pts',(77.5872162447358,-7.07885707968089,14.6429296330323));
#31882=CARTESIAN_POINT('Ctrl Pts',(77.846685398312,-12.4966715102306,10.6542004249985));
#31883=CARTESIAN_POINT('Ctrl Pts',(78.0803862302803,-15.4276682037717,5.26688438574245));
#31884=CARTESIAN_POINT('Ctrl Pts',(78.3532145233418,-16.2985957883637,-1.68306604566752));
#31885=CARTESIAN_POINT('Ctrl Pts',(78.639230520238,-14.2127530389122,-8.95864314282349));
#31886=CARTESIAN_POINT('Ctrl Pts',(78.9906062755114,-7.26956674749928,-15.1628401104227));
#31887=CARTESIAN_POINT('Ctrl Pts',(79.3423379425772,1.91162644513308,-16.7235371996257));
#31888=CARTESIAN_POINT('Ctrl Pts',(79.6944332129699,10.5284119075426,-13.1569449089522));
#31889=CARTESIAN_POINT('Ctrl Pts',(80.0468964689781,15.9307968428758,-5.54383713737964));
#31890=CARTESIAN_POINT('Ctrl Pts',(80.3997335729651,16.4563471991834,3.7845448884978));
#31891=CARTESIAN_POINT('Ctrl Pts',(80.7529499471889,11.9322974734141,11.9757512534284));
#31892=CARTESIAN_POINT('Ctrl Pts',(81.0672605152526,4.64727666760693,15.9968648754117));
#31893=CARTESIAN_POINT('Ctrl Pts',(81.3425355553074,-2.48245353398034,16.2570098744713));
#31894=CARTESIAN_POINT('Ctrl Pts',(81.578659307521,-8.25629043460913,14.2392789277651));
#31895=CARTESIAN_POINT('Ctrl Pts',(81.8149585891481,-12.8972496915939,10.2447011996574));
#31896=CARTESIAN_POINT('Ctrl Pts',(82.0514351845093,-15.7618455262871,4.82905942687374));
#31897=CARTESIAN_POINT('Ctrl Pts',(82.2880894843119,-16.4472559956533,-1.26442742198006));
#31898=CARTESIAN_POINT('Ctrl Pts',(82.5249231812786,-14.859753523671,-7.19146106306312));
#31899=CARTESIAN_POINT('Ctrl Pts',(82.7619370618063,-11.2133046829268,-12.1326712627875));
#31900=CARTESIAN_POINT('Ctrl Pts',(82.9991329362443,-6.01067514441112,-15.4036195228323));
#31901=CARTESIAN_POINT('Ctrl Pts',(83.2365115257908,0.0328026357451166,
-16.5469545639429));
#31902=CARTESIAN_POINT('Ctrl Pts',(83.4740741545337,6.08071192374398,-15.4032396381725));
#31903=CARTESIAN_POINT('Ctrl Pts',(83.7118214220829,11.2965930002099,-12.1262135570267));
#31904=CARTESIAN_POINT('Ctrl Pts',(83.9497552306074,14.9583526864088,-7.166418458723));
#31905=CARTESIAN_POINT('Ctrl Pts',(84.1878744720314,16.5544286075028,-1.20709720700542));
#31906=CARTESIAN_POINT('Ctrl Pts',(84.4261826539153,15.8636982242883,4.92878564118838));
#31907=CARTESIAN_POINT('Ctrl Pts',(84.6646792725393,12.9769490355419,10.3917177919627));
#31908=CARTESIAN_POINT('Ctrl Pts',(84.9033652615053,8.28944183209289,14.4271871126583));
#31909=CARTESIAN_POINT('Ctrl Pts',(85.1422415313731,2.44872748562762,16.4691811951198));
#31910=CARTESIAN_POINT('Ctrl Pts',(85.4211527257243,-4.77508597602963,16.2066560777324));
#31911=CARTESIAN_POINT('Ctrl Pts',(85.7402304059049,-12.1717760149211,12.1269180477954));
#31912=CARTESIAN_POINT('Ctrl Pts',(86.0996256302246,-16.7773770828534,3.79415904445876));
#31913=CARTESIAN_POINT('Ctrl Pts',(86.4594555284599,-16.2449490675834,-5.71927479188544));
#31914=CARTESIAN_POINT('Ctrl Pts',(86.8197255804431,-10.7244313897633,-13.50198698288));
#31915=CARTESIAN_POINT('Ctrl Pts',(87.1804283172508,-1.90077784239629,-17.1593109571835));
#31916=CARTESIAN_POINT('Ctrl Pts',(87.5415861772252,7.5319100185124,-15.5572454672215));
#31917=CARTESIAN_POINT('Ctrl Pts',(87.8428916470029,13.4767793834455,-10.2428656830246));
#31918=CARTESIAN_POINT('Ctrl Pts',(88.084202234992,16.0056354393952,-4.56413387924517));
#31919=CARTESIAN_POINT('Ctrl Pts',(88.2048947778817,16.4372214891323,-1.52778189497975));
#31920=CARTESIAN_POINT('Ctrl Pts',(88.265253815439,16.4401199068752,0.0354313507669335));
#31921=CARTESIAN_POINT('Ctrl Pts',(69.3554865621267,15.7586009948934,-0.0220509501548168));
#31922=CARTESIAN_POINT('Ctrl Pts',(69.4134811104057,15.7558161189664,1.47992539504222));
#31923=CARTESIAN_POINT('Ctrl Pts',(69.5290493343402,15.3425635750154,4.38734680893652));
#31924=CARTESIAN_POINT('Ctrl Pts',(69.7605748863597,12.916682078002,9.83583944427305));
#31925=CARTESIAN_POINT('Ctrl Pts',(70.0495466337453,7.21496031817409,14.9325634258652));
#31926=CARTESIAN_POINT('Ctrl Pts',(70.3962293867449,-1.83928108127539,16.4716096115821));
#31927=CARTESIAN_POINT('Ctrl Pts',(70.7426082400899,-10.31166028394,12.9599789925058));
#31928=CARTESIAN_POINT('Ctrl Pts',(71.0887904289397,-15.6191617372178,5.48152514440198));
#31929=CARTESIAN_POINT('Ctrl Pts',(71.3770873439344,-16.0409364055185,-2.13882427430054));
#31930=CARTESIAN_POINT('Ctrl Pts',(71.6076152300708,-13.9198137867518,-7.67505850180117));
#31931=CARTESIAN_POINT('Ctrl Pts',(71.7804597344815,-11.2497340227708,-11.2263471634346));
#31932=CARTESIAN_POINT('Ctrl Pts',(71.9532548218948,-7.69870714190467,-13.8971433806351));
#31933=CARTESIAN_POINT('Ctrl Pts',(72.1451937394336,-3.08867215696627,-15.6581893785022));
#31934=CARTESIAN_POINT('Ctrl Pts',(72.356261775191,2.37585195054601,-15.8634589022843));
#31935=CARTESIAN_POINT('Ctrl Pts',(72.5864337561947,8.00512203809534,-13.8929836091311));
#31936=CARTESIAN_POINT('Ctrl Pts',(72.816525322706,12.5229127584701,-10.0046290172406));
#31937=CARTESIAN_POINT('Ctrl Pts',(73.0465358476154,15.309660950597,-4.73576036816845));
#31938=CARTESIAN_POINT('Ctrl Pts',(73.276472152517,15.9729502769563,1.18315283570215));
#31939=CARTESIAN_POINT('Ctrl Pts',(73.5446463126725,14.1808529658398,7.89830187925463));
#31940=CARTESIAN_POINT('Ctrl Pts',(73.851023436174,8.78001534186335,13.9496872794977));
#31941=CARTESIAN_POINT('Ctrl Pts',(74.1955442149099,0.00951954523056671,
16.4744918719307));
#31942=CARTESIAN_POINT('Ctrl Pts',(74.5399278818977,-8.75322061768005,13.949641737885));
#31943=CARTESIAN_POINT('Ctrl Pts',(74.8841816357822,-14.8282967853525,7.15077110646269));
#31944=CARTESIAN_POINT('Ctrl Pts',(75.228316026177,-16.3549723822615,-1.83380979289747));
#31945=CARTESIAN_POINT('Ctrl Pts',(75.5723397010806,-12.8663512055993,-10.2527952448652));
#31946=CARTESIAN_POINT('Ctrl Pts',(75.9162626563545,-5.44121162363188,-15.5199611086518));
#31947=CARTESIAN_POINT('Ctrl Pts',(76.2728291254588,3.99577624336786,-16.0569242553695));
#31948=CARTESIAN_POINT('Ctrl Pts',(76.5401884256857,10.1306890549616,-12.4075975768256));
#31949=CARTESIAN_POINT('Ctrl Pts',(76.7693156308531,13.7120020373686,-7.78532179148715));
#31950=CARTESIAN_POINT('Ctrl Pts',(76.9475149829319,15.5619033942757,-3.55809108490052));
#31951=CARTESIAN_POINT('Ctrl Pts',(77.1765954339299,15.7828857769102,2.37536910232938));
#31952=CARTESIAN_POINT('Ctrl Pts',(77.4056552297485,13.8231696965287,7.97591454512957));
#31953=CARTESIAN_POINT('Ctrl Pts',(77.6346912714932,9.95182205786405,12.4744758684292));
#31954=CARTESIAN_POINT('Ctrl Pts',(77.8637085143845,4.70655604086376,15.2464176389137));
#31955=CARTESIAN_POINT('Ctrl Pts',(78.0927102070453,-1.19116127275504,15.9118920613635));
#31956=CARTESIAN_POINT('Ctrl Pts',(78.321696409481,-6.91812279056631,14.3740271026128));
#31957=CARTESIAN_POINT('Ctrl Pts',(78.5761156945386,-12.2301612837638,10.4626553659842));
#31958=CARTESIAN_POINT('Ctrl Pts',(78.8050826972065,-15.1012059510755,5.18423341933701));
#31959=CARTESIAN_POINT('Ctrl Pts',(79.0722068078515,-15.9537211944819,-1.62036410733684));
#31960=CARTESIAN_POINT('Ctrl Pts',(79.3520505918744,-13.9120232543956,-8.73854028938565));
#31961=CARTESIAN_POINT('Ctrl Pts',(79.6954998806611,-7.12472860195661,-14.8017620279139));
#31962=CARTESIAN_POINT('Ctrl Pts',(80.038964842755,1.8407196869181,-16.3245995393403));
#31963=CARTESIAN_POINT('Ctrl Pts',(80.3824543573656,10.2463570189986,-12.8441193957147));
#31964=CARTESIAN_POINT('Ctrl Pts',(80.7259783705505,15.510715150953,-5.42350262165804));
#31965=CARTESIAN_POINT('Ctrl Pts',(81.0695469282049,16.0213174103418,3.65983970761737));
#31966=CARTESIAN_POINT('Ctrl Pts',(81.4131701287784,11.6191576623806,11.6279814012209));
#31967=CARTESIAN_POINT('Ctrl Pts',(81.7186693781985,4.53794766693765,15.5355013496972));
#31968=CARTESIAN_POINT('Ctrl Pts',(81.9860293495058,-2.38675512585456,15.7877899821334));
#31969=CARTESIAN_POINT('Ctrl Pts',(82.215230127172,-7.99122526150496,13.8289386577737));
#31970=CARTESIAN_POINT('Ctrl Pts',(82.4444696685961,-12.4933309249039,9.95347113038892));
#31971=CARTESIAN_POINT('Ctrl Pts',(82.673750686035,-15.2705152113464,4.70245808038809));
#31972=CARTESIAN_POINT('Ctrl Pts',(82.9030760103164,-15.9344030721451,-1.20235742623294));
#31973=CARTESIAN_POINT('Ctrl Pts',(83.1324471253651,-14.396643605772,-6.9425988949701));
#31974=CARTESIAN_POINT('Ctrl Pts',(83.3618675312114,-10.8667692731275,-11.7253679559343));
#31975=CARTESIAN_POINT('Ctrl Pts',(83.5913426476898,-5.83330998696166,-14.889628493777));
#31976=CARTESIAN_POINT('Ctrl Pts',(83.8208701982859,0.0103976999952868,
-15.9948935423422));
#31977=CARTESIAN_POINT('Ctrl Pts',(84.0504569625436,5.85526780827805,-14.8893117845691));
#31978=CARTESIAN_POINT('Ctrl Pts',(84.2801046886058,10.8933554968448,-11.7236661989334));
#31979=CARTESIAN_POINT('Ctrl Pts',(84.5098145369384,14.4284025727732,-6.93508138626014));
#31980=CARTESIAN_POINT('Ctrl Pts',(84.7395942161118,15.9683236638494,-1.18436897605337));
#31981=CARTESIAN_POINT('Ctrl Pts',(84.9694401440822,15.3018668690941,4.73368770101318));
#31982=CARTESIAN_POINT('Ctrl Pts',(85.1993580490269,12.5186922290628,10.0000809026083));
#31983=CARTESIAN_POINT('Ctrl Pts',(85.4293506363143,8.00167975043132,13.8884351919084));
#31984=CARTESIAN_POINT('Ctrl Pts',(85.6594199151074,2.37613020638112,15.8549524353607));
#31985=CARTESIAN_POINT('Ctrl Pts',(85.9279288353029,-4.57837170569589,15.6019263798431));
#31986=CARTESIAN_POINT('Ctrl Pts',(86.2349268185622,-11.6949474665043,11.6758532799693));
#31987=CARTESIAN_POINT('Ctrl Pts',(86.5804999095392,-16.1227972318607,3.66306032098784));
#31988=CARTESIAN_POINT('Ctrl Pts',(86.9262673138911,-15.6104368586567,-5.47901881528954));
#31989=CARTESIAN_POINT('Ctrl Pts',(87.2722614297209,-10.308000965391,-12.952773643117));
#31990=CARTESIAN_POINT('Ctrl Pts',(87.6184399210169,-1.83881862598979,-16.4630114594182));
#31991=CARTESIAN_POINT('Ctrl Pts',(87.9649223234146,7.2099881294249,-14.9245647492593));
#31992=CARTESIAN_POINT('Ctrl Pts',(88.2537065209088,12.9084970264012,-9.83094298475437));
#31993=CARTESIAN_POINT('Ctrl Pts',(88.4851031381616,15.3329342416512,-4.3853617140389));
#31994=CARTESIAN_POINT('Ctrl Pts',(88.6005976121871,15.745854566904,-1.47969784819705));
#31995=CARTESIAN_POINT('Ctrl Pts',(88.6585631413514,15.7486380492955,0.0215269336002149));
#31996=CARTESIAN_POINT('Ctrl Pts',(69.6070021409208,16.2225732106956,-0.030902239567753));
#31997=CARTESIAN_POINT('Ctrl Pts',(69.6666095923113,16.2197108837808,1.51284600302981));
#31998=CARTESIAN_POINT('Ctrl Pts',(69.7856674073585,15.7940421807546,4.50812319888975));
#31999=CARTESIAN_POINT('Ctrl Pts',(70.0238631486952,13.2979406585872,10.1135870839616));
#32000=CARTESIAN_POINT('Ctrl Pts',(70.3212301672275,7.43083592330514,15.3586300203037));
#32001=CARTESIAN_POINT('Ctrl Pts',(70.6777768910567,-1.88174215475493,16.9404787438039));
#32002=CARTESIAN_POINT('Ctrl Pts',(71.0339167259705,-10.5926919897194,13.3297345456673));
#32003=CARTESIAN_POINT('Ctrl Pts',(71.3897046015357,-16.0471465206019,5.64301645195004));
#32004=CARTESIAN_POINT('Ctrl Pts',(71.6858849274608,-16.4799945267065,-2.18584392000218));
#32005=CARTESIAN_POINT('Ctrl Pts',(71.9226506457541,-14.3013440642795,-7.87192383812878));
#32006=CARTESIAN_POINT('Ctrl Pts',(72.1001347007795,-11.5594963624761,-11.5185330246076));
#32007=CARTESIAN_POINT('Ctrl Pts',(72.2775300867685,-7.91383757171182,-14.2604076269911));
#32008=CARTESIAN_POINT('Ctrl Pts',(72.4745372394819,-3.18199126478013,-16.0678915474459));
#32009=CARTESIAN_POINT('Ctrl Pts',(72.6911206000822,2.42541506478198,-16.278352413953));
#32010=CARTESIAN_POINT('Ctrl Pts',(72.9272379722367,8.20009129902322,-14.2567707145772));
#32011=CARTESIAN_POINT('Ctrl Pts',(73.1632010972874,12.8330823756507,-10.2689825602553));
#32012=CARTESIAN_POINT('Ctrl Pts',(73.3990107185643,15.6899365867221,-4.86715147392478));
#32013=CARTESIAN_POINT('Ctrl Pts',(73.6346690720767,16.3695278473878,1.19911655094387));
#32014=CARTESIAN_POINT('Ctrl Pts',(73.9094295079317,14.5331741821317,8.07916458355286));
#32015=CARTESIAN_POINT('Ctrl Pts',(74.2231998790054,9.00147961852772,14.2762190647474));
#32016=CARTESIAN_POINT('Ctrl Pts',(74.5758598201176,0.0235694186269233,
16.859981462138));
#32017=CARTESIAN_POINT('Ctrl Pts',(74.9281977685756,-8.94137318857348,14.276105227731));
#32018=CARTESIAN_POINT('Ctrl Pts',(75.2802179203447,-15.1529298525304,7.32337194121319));
#32019=CARTESIAN_POINT('Ctrl Pts',(75.6319267377427,-16.7124468093521,-1.85904424112892));
#32020=CARTESIAN_POINT('Ctrl Pts',(75.9833295246471,-13.1483029282851,-10.4582351450381));
#32021=CARTESIAN_POINT('Ctrl Pts',(76.3344329097446,-5.56776703481709,-15.8346725704608));
#32022=CARTESIAN_POINT('Ctrl Pts',(76.6982359590696,4.06068437376695,-16.3816517697198));
#32023=CARTESIAN_POINT('Ctrl Pts',(76.9708544639752,10.3157792069132,-12.6599643611329));
#32024=CARTESIAN_POINT('Ctrl Pts',(77.2043879176041,13.965893382995,-7.94880609169154));
#32025=CARTESIAN_POINT('Ctrl Pts',(77.3859744123835,15.8507322928185,-3.64123533389424));
#32026=CARTESIAN_POINT('Ctrl Pts',(77.6193054202522,16.0755335889672,2.40228153812341));
#32027=CARTESIAN_POINT('Ctrl Pts',(77.8525294367406,14.0799995000416,8.10441349915241));
#32028=CARTESIAN_POINT('Ctrl Pts',(78.0856299239375,10.1398119136579,12.6825221559361));
#32029=CARTESIAN_POINT('Ctrl Pts',(78.3186141911062,4.80368400525854,15.5022129275132));
#32030=CARTESIAN_POINT('Ctrl Pts',(78.5514889552242,-1.19363492880806,16.1786335212657));
#32031=CARTESIAN_POINT('Ctrl Pts',(78.7842389031178,-7.01459644633699,14.6153021683494));
#32032=CARTESIAN_POINT('Ctrl Pts',(79.0427392288324,-12.4115223173748,10.6410404315552));
#32033=CARTESIAN_POINT('Ctrl Pts',(79.2752536639931,-15.3266141779886,5.28072960093371));
#32034=CARTESIAN_POINT('Ctrl Pts',(79.5463978277233,-16.1917927772552,-1.62616608384562));
#32035=CARTESIAN_POINT('Ctrl Pts',(79.830336133723,-14.1196421847273,-8.84796354024379));
#32036=CARTESIAN_POINT('Ctrl Pts',(80.1785663678619,-7.2374943514207,-14.9946681804509));
#32037=CARTESIAN_POINT('Ctrl Pts',(80.5265809649815,1.84643761050977,-16.5367454191282));
#32038=CARTESIAN_POINT('Ctrl Pts',(80.8743817846602,10.3568459885564,-13.0118769647398));
#32039=CARTESIAN_POINT('Ctrl Pts',(81.2219788370638,15.6825995752614,-5.50309727131032));
#32040=CARTESIAN_POINT('Ctrl Pts',(81.5693820034866,16.197894141286,3.68117803479642));
#32041=CARTESIAN_POINT('Ctrl Pts',(81.9165951257598,11.7491068886896,11.7316901046367));
#32042=CARTESIAN_POINT('Ctrl Pts',(82.2250791599112,4.59879843509523,15.6763055088053));
#32043=CARTESIAN_POINT('Ctrl Pts',(82.494874661093,-2.38871229569965,15.9305201345378));
#32044=CARTESIAN_POINT('Ctrl Pts',(82.7260604745634,-8.04129839042069,13.9545033940471));
#32045=CARTESIAN_POINT('Ctrl Pts',(82.9571714599228,-12.5797889573595,10.0473605792937));
#32046=CARTESIAN_POINT('Ctrl Pts',(83.1882097228089,-15.3778215921963,4.75615357961634));
#32047=CARTESIAN_POINT('Ctrl Pts',(83.4191804497281,-16.0462077838481,-1.19082289641883));
#32048=CARTESIAN_POINT('Ctrl Pts',(83.6500940780417,-14.4978423341918,-6.96925130505314));
#32049=CARTESIAN_POINT('Ctrl Pts',(83.8809495762235,-10.9459258030931,-11.7814679381592));
#32050=CARTESIAN_POINT('Ctrl Pts',(84.1117286673162,-5.88383263291072,-14.963328438817));
#32051=CARTESIAN_POINT('Ctrl Pts',(84.3424712753825,-0.00960900109378653,
-16.0741042425561));
#32052=CARTESIAN_POINT('Ctrl Pts',(84.5731512945906,5.86267537367017,-14.9629860621253));
#32053=CARTESIAN_POINT('Ctrl Pts',(84.8037792961649,10.9218384506065,-11.7838260530281));
#32054=CARTESIAN_POINT('Ctrl Pts',(85.0343656809765,14.4698283252947,-6.97716202595678));
#32055=CARTESIAN_POINT('Ctrl Pts',(85.2648844583555,16.0144277219097,-1.2080918245963));
#32056=CARTESIAN_POINT('Ctrl Pts',(85.4953739959645,15.3458392252552,4.72610127787273));
#32057=CARTESIAN_POINT('Ctrl Pts',(85.7258198618693,12.5562210702063,10.00410823671));
#32058=CARTESIAN_POINT('Ctrl Pts',(85.9562252150393,8.0312146091608,13.8989981706252));
#32059=CARTESIAN_POINT('Ctrl Pts',(86.1865940423216,2.39864591071217,15.867693537978));
#32060=CARTESIAN_POINT('Ctrl Pts',(86.4553119485186,-4.56089462950754,15.6141613511442));
#32061=CARTESIAN_POINT('Ctrl Pts',(86.7623866182725,-11.6781310560641,11.6867952015708));
#32062=CARTESIAN_POINT('Ctrl Pts',(87.1077738505521,-16.1023612946132,3.67847646190086));
#32063=CARTESIAN_POINT('Ctrl Pts',(87.4531045042511,-15.5897167721347,-5.45112153800786));
#32064=CARTESIAN_POINT('Ctrl Pts',(87.7984014742918,-10.2975531213566,-12.908627927612));
#32065=CARTESIAN_POINT('Ctrl Pts',(88.1436343462562,-1.85181910129904,-16.4079507936403));
#32066=CARTESIAN_POINT('Ctrl Pts',(88.4889072862287,7.16466504256959,-14.8740297187205));
#32067=CARTESIAN_POINT('Ctrl Pts',(88.7764963641934,12.8387384302061,-9.80149223202101));
#32068=CARTESIAN_POINT('Ctrl Pts',(89.0067723369147,15.2512782914413,-4.38243329541124));
#32069=CARTESIAN_POINT('Ctrl Pts',(89.1216614258076,15.6621913514837,-1.49222289505446));
#32070=CARTESIAN_POINT('Ctrl Pts',(89.1793401389101,15.6649610610784,0.00157375857939028));
#32071=CARTESIAN_POINT('Ctrl Pts',(69.6184828603025,16.4616571598233,-0.030902239567753));
#32072=CARTESIAN_POINT('Ctrl Pts',(69.6789219655699,16.458754897209,1.53438465601481));
#32073=CARTESIAN_POINT('Ctrl Pts',(69.7997830801149,16.0266321943109,4.57501994136558));
#32074=CARTESIAN_POINT('Ctrl Pts',(70.0414349064678,13.4941722421641,10.2617903021912));
#32075=CARTESIAN_POINT('Ctrl Pts',(70.3432064666604,7.54051932200945,15.5847054098009));
#32076=CARTESIAN_POINT('Ctrl Pts',(70.7049768750637,-1.90873983484295,17.1894487135762));
#32077=CARTESIAN_POINT('Ctrl Pts',(71.0663492060979,-10.7475553396686,13.525924310196));
#32078=CARTESIAN_POINT('Ctrl Pts',(71.4273437518671,-16.2818464768058,5.72657424978343));
#32079=CARTESIAN_POINT('Ctrl Pts',(71.7278512234343,-16.7210289894503,-2.21659997283488));
#32080=CARTESIAN_POINT('Ctrl Pts',(71.9680675578449,-14.5106197428725,-7.98557322489482));
#32081=CARTESIAN_POINT('Ctrl Pts',(72.1481344157904,-11.7288725172833,-11.6852538002611));
#32082=CARTESIAN_POINT('Ctrl Pts',(72.328106524648,-8.03024824250695,-14.4669696417765));
#32083=CARTESIAN_POINT('Ctrl Pts',(72.5279702250768,-3.22977654241172,-16.300670274406));
#32084=CARTESIAN_POINT('Ctrl Pts',(72.7476856540044,2.4587525001183,-16.5141747132305));
#32085=CARTESIAN_POINT('Ctrl Pts',(72.9872078330289,8.31673840998305,-14.4634243432854));
#32086=CARTESIAN_POINT('Ctrl Pts',(73.2265632969346,13.0163496494046,-10.4182667032949));
#32087=CARTESIAN_POINT('Ctrl Pts',(73.4657526686465,15.9141590581627,-4.93897396144999));
#32088=CARTESIAN_POINT('Ctrl Pts',(73.7047766516472,16.6034312776959,1.21397241511146));
#32089=CARTESIAN_POINT('Ctrl Pts',(73.9834458021771,14.7409225736484,8.19195097348461));
#32090=CARTESIAN_POINT('Ctrl Pts',(74.301651818573,9.13086318160831,14.4766680019069));
#32091=CARTESIAN_POINT('Ctrl Pts',(74.6592672763964,0.0266353994119735,
17.0966775050227));
#32092=CARTESIAN_POINT('Ctrl Pts',(75.016519558125,-9.06348425632334,14.4765973593132));
#32093=CARTESIAN_POINT('Ctrl Pts',(75.3734117874807,-15.3610417662207,7.42742367726323));
#32094=CARTESIAN_POINT('Ctrl Pts',(75.7299471567895,-16.9418739975217,-1.88122771580553));
#32095=CARTESIAN_POINT('Ctrl Pts',(76.0861289312927,-13.3290621410899,-10.5975142741848));
#32096=CARTESIAN_POINT('Ctrl Pts',(76.4419606933661,-5.64617345782912,-16.0463992053949));
#32097=CARTESIAN_POINT('Ctrl Pts',(76.810612386967,4.11087115606672,-16.6005218369866));
#32098=CARTESIAN_POINT('Ctrl Pts',(77.0868204963524,10.4484384772329,-12.8295775485076));
#32099=CARTESIAN_POINT('Ctrl Pts',(77.3234199677928,14.1464940116618,-8.0565595801055));
#32100=CARTESIAN_POINT('Ctrl Pts',(77.5073642434964,16.0558684975652,-3.69288655028273));
#32101=CARTESIAN_POINT('Ctrl Pts',(77.743715642047,16.2835727900373,2.42892269363191));
#32102=CARTESIAN_POINT('Ctrl Pts',(77.9799198273595,14.2624210045081,8.20410639070391));
#32103=CARTESIAN_POINT('Ctrl Pts',(78.2159782861261,10.2721221270508,12.8404255794219));
#32104=CARTESIAN_POINT('Ctrl Pts',(78.451892297019,4.86870939460828,15.6955819848942));
#32105=CARTESIAN_POINT('Ctrl Pts',(78.687663274949,-1.20342672163651,16.3804065631851));
#32106=CARTESIAN_POINT('Ctrl Pts',(78.923292730736,-7.09646797598974,14.7976258939457));
#32107=CARTESIAN_POINT('Ctrl Pts',(79.1849474554113,-12.559397153018,10.7746599228106));
#32108=CARTESIAN_POINT('Ctrl Pts',(79.4202749429787,-15.5097121162534,5.34934186422077));
#32109=CARTESIAN_POINT('Ctrl Pts',(79.6946643695902,-16.3852200323318,-1.64037324259347));
#32110=CARTESIAN_POINT('Ctrl Pts',(79.9819403068823,-14.2884064522935,-8.94742064680176));
#32111=CARTESIAN_POINT('Ctrl Pts',(80.3342067288376,-7.3260467326971,-15.165426706738));
#32112=CARTESIAN_POINT('Ctrl Pts',(80.6861788812633,1.86167912032264,-16.7248261450382));
#32113=CARTESIAN_POINT('Ctrl Pts',(81.037862268153,10.4673895230379,-13.1602039003653));
#32114=CARTESIAN_POINT('Ctrl Pts',(81.3892625213115,15.8514527926196,-5.5687461546451));
#32115=CARTESIAN_POINT('Ctrl Pts',(81.7403859218982,16.3720606810702,3.71439472873355));
#32116=CARTESIAN_POINT('Ctrl Pts',(82.0912385240458,11.8761863054331,11.8495550298708));
#32117=CARTESIAN_POINT('Ctrl Pts',(82.4028723251709,4.65229996881944,15.8345467687591));
#32118=CARTESIAN_POINT('Ctrl Pts',(82.6753839687717,-2.4057965557233,16.0912478601411));
#32119=CARTESIAN_POINT('Ctrl Pts',(82.9088524431066,-8.11448174868296,14.0955831155642));
#32120=CARTESIAN_POINT('Ctrl Pts',(83.1422098352473,-12.6971950976412,10.1502287241044));
#32121=CARTESIAN_POINT('Ctrl Pts',(83.3754581634701,-15.522088392645,4.8081952387983));
#32122=CARTESIAN_POINT('Ctrl Pts',(83.6085992893649,-16.1966474690964,-1.19488542166675));
#32123=CARTESIAN_POINT('Ctrl Pts',(83.8416352233784,-14.6339538883274,-7.02670369688337));
#32124=CARTESIAN_POINT('Ctrl Pts',(84.0745679545012,-11.0497598473816,-11.8824317127295));
#32125=CARTESIAN_POINT('Ctrl Pts',(84.3073996737489,-5.94248428783527,-15.09263970399));
#32126=CARTESIAN_POINT('Ctrl Pts',(84.540132268385,-0.0171665032603614,
-16.2129461632812));
#32127=CARTESIAN_POINT('Ctrl Pts',(84.7727680106188,5.90520262635639,-15.0923025294507));
#32128=CARTESIAN_POINT('Ctrl Pts',(85.0053088744204,11.0065171159269,-11.8864785100097));
#32129=CARTESIAN_POINT('Ctrl Pts',(85.2377570340819,14.5833427924651,-7.04062680693156));
#32130=CARTESIAN_POINT('Ctrl Pts',(85.4701144791861,16.1401640578478,-1.22533588346504));
#32131=CARTESIAN_POINT('Ctrl Pts',(85.7023835299595,15.4662929248669,4.7550040735545));
#32132=CARTESIAN_POINT('Ctrl Pts',(85.9345662446591,12.6553888178413,10.0730373304554));
#32133=CARTESIAN_POINT('Ctrl Pts',(86.1666649327954,8.09679983295076,13.9966583914468));
#32134=CARTESIAN_POINT('Ctrl Pts',(86.3986815381799,2.42358552200963,15.9794357678464));
#32135=CARTESIAN_POINT('Ctrl Pts',(86.6692750541127,-4.58486198073758,15.7239726419428));
#32136=CARTESIAN_POINT('Ctrl Pts',(86.9783943834765,-11.7499252678846,11.7698005968098));
#32137=CARTESIAN_POINT('Ctrl Pts',(87.3259902517892,-16.2024151439095,3.70954956442589));
#32138=CARTESIAN_POINT('Ctrl Pts',(87.6734207471648,-15.6862303609498,-5.47622167055361));
#32139=CARTESIAN_POINT('Ctrl Pts',(88.0207132272952,-10.3628479251535,-12.9771513909202));
#32140=CARTESIAN_POINT('Ctrl Pts',(88.3678323138933,-1.8703041859877,-16.4954810466909));
#32141=CARTESIAN_POINT('Ctrl Pts',(88.7148821316246,7.193051660985,-14.9532751855446));
#32142=CARTESIAN_POINT('Ctrl Pts',(89.003856786706,12.8943942592402,-9.85553205895293));
#32143=CARTESIAN_POINT('Ctrl Pts',(89.2351907747089,15.3179503044652,-4.41141050395984));
#32144=CARTESIAN_POINT('Ctrl Pts',(89.3506074633962,15.7305922894428,-1.50774141983879));
#32145=CARTESIAN_POINT('Ctrl Pts',(89.4085387704217,15.7333741285005,-0.00740294277221285));
#32146=CARTESIAN_POINT('',(69.6184828603025,16.4616571598233,-0.0309022395677529));
#32147=CARTESIAN_POINT('Origin',(68.82,16.5,-1.31470342757595E-16));
#32148=CARTESIAN_POINT('',(89.4085387704217,15.7333741285004,-0.00740294277221266));
#32149=CARTESIAN_POINT('Ctrl Pts',(69.6184828603025,16.4616571598233,-0.030902239567753));
#32150=CARTESIAN_POINT('Ctrl Pts',(69.6789219655699,16.458754897209,1.53438465601481));
#32151=CARTESIAN_POINT('Ctrl Pts',(69.7997830801149,16.0266321943109,4.57501994136558));
#32152=CARTESIAN_POINT('Ctrl Pts',(70.0414349064678,13.4941722421641,10.2617903021912));
#32153=CARTESIAN_POINT('Ctrl Pts',(70.3432064666604,7.54051932200945,15.5847054098009));
#32154=CARTESIAN_POINT('Ctrl Pts',(70.7049768750637,-1.90873983484295,17.1894487135762));
#32155=CARTESIAN_POINT('Ctrl Pts',(71.0663492060979,-10.7475553396686,13.525924310196));
#32156=CARTESIAN_POINT('Ctrl Pts',(71.4273437518671,-16.2818464768058,5.72657424978343));
#32157=CARTESIAN_POINT('Ctrl Pts',(71.7278512234343,-16.7210289894503,-2.21659997283488));
#32158=CARTESIAN_POINT('Ctrl Pts',(71.9680675578449,-14.5106197428725,-7.98557322489482));
#32159=CARTESIAN_POINT('Ctrl Pts',(72.1481344157904,-11.7288725172833,-11.6852538002611));
#32160=CARTESIAN_POINT('Ctrl Pts',(72.328106524648,-8.03024824250695,-14.4669696417765));
#32161=CARTESIAN_POINT('Ctrl Pts',(72.5279702250768,-3.22977654241172,-16.300670274406));
#32162=CARTESIAN_POINT('Ctrl Pts',(72.7476856540044,2.4587525001183,-16.5141747132305));
#32163=CARTESIAN_POINT('Ctrl Pts',(72.9872078330289,8.31673840998305,-14.4634243432854));
#32164=CARTESIAN_POINT('Ctrl Pts',(73.2265632969346,13.0163496494046,-10.4182667032949));
#32165=CARTESIAN_POINT('Ctrl Pts',(73.4657526686465,15.9141590581627,-4.93897396144999));
#32166=CARTESIAN_POINT('Ctrl Pts',(73.7047766516472,16.6034312776959,1.21397241511146));
#32167=CARTESIAN_POINT('Ctrl Pts',(73.9834458021771,14.7409225736484,8.19195097348461));
#32168=CARTESIAN_POINT('Ctrl Pts',(74.301651818573,9.13086318160831,14.4766680019069));
#32169=CARTESIAN_POINT('Ctrl Pts',(74.6592672763964,0.0266353994119735,
17.0966775050227));
#32170=CARTESIAN_POINT('Ctrl Pts',(75.016519558125,-9.06348425632334,14.4765973593132));
#32171=CARTESIAN_POINT('Ctrl Pts',(75.3734117874807,-15.3610417662207,7.42742367726323));
#32172=CARTESIAN_POINT('Ctrl Pts',(75.7299471567895,-16.9418739975217,-1.88122771580553));
#32173=CARTESIAN_POINT('Ctrl Pts',(76.0861289312927,-13.3290621410899,-10.5975142741848));
#32174=CARTESIAN_POINT('Ctrl Pts',(76.4419606933661,-5.64617345782912,-16.0463992053949));
#32175=CARTESIAN_POINT('Ctrl Pts',(76.810612386967,4.11087115606672,-16.6005218369866));
#32176=CARTESIAN_POINT('Ctrl Pts',(77.0868204963524,10.4484384772329,-12.8295775485076));
#32177=CARTESIAN_POINT('Ctrl Pts',(77.3234199677928,14.1464940116618,-8.0565595801055));
#32178=CARTESIAN_POINT('Ctrl Pts',(77.5073642434964,16.0558684975652,-3.69288655028273));
#32179=CARTESIAN_POINT('Ctrl Pts',(77.743715642047,16.2835727900373,2.42892269363191));
#32180=CARTESIAN_POINT('Ctrl Pts',(77.9799198273595,14.2624210045081,8.20410639070391));
#32181=CARTESIAN_POINT('Ctrl Pts',(78.2159782861261,10.2721221270508,12.8404255794219));
#32182=CARTESIAN_POINT('Ctrl Pts',(78.451892297019,4.86870939460828,15.6955819848942));
#32183=CARTESIAN_POINT('Ctrl Pts',(78.687663274949,-1.20342672163651,16.3804065631851));
#32184=CARTESIAN_POINT('Ctrl Pts',(78.923292730736,-7.09646797598974,14.7976258939457));
#32185=CARTESIAN_POINT('Ctrl Pts',(79.1849474554113,-12.559397153018,10.7746599228106));
#32186=CARTESIAN_POINT('Ctrl Pts',(79.4202749429787,-15.5097121162534,5.34934186422077));
#32187=CARTESIAN_POINT('Ctrl Pts',(79.6946643695902,-16.3852200323318,-1.64037324259347));
#32188=CARTESIAN_POINT('Ctrl Pts',(79.9819403068823,-14.2884064522935,-8.94742064680176));
#32189=CARTESIAN_POINT('Ctrl Pts',(80.3342067288376,-7.3260467326971,-15.165426706738));
#32190=CARTESIAN_POINT('Ctrl Pts',(80.6861788812633,1.86167912032264,-16.7248261450382));
#32191=CARTESIAN_POINT('Ctrl Pts',(81.037862268153,10.4673895230379,-13.1602039003653));
#32192=CARTESIAN_POINT('Ctrl Pts',(81.3892625213115,15.8514527926196,-5.5687461546451));
#32193=CARTESIAN_POINT('Ctrl Pts',(81.7403859218982,16.3720606810702,3.71439472873355));
#32194=CARTESIAN_POINT('Ctrl Pts',(82.0912385240458,11.8761863054331,11.8495550298708));
#32195=CARTESIAN_POINT('Ctrl Pts',(82.4028723251709,4.65229996881944,15.8345467687591));
#32196=CARTESIAN_POINT('Ctrl Pts',(82.6753839687717,-2.4057965557233,16.0912478601411));
#32197=CARTESIAN_POINT('Ctrl Pts',(82.9088524431066,-8.11448174868296,14.0955831155642));
#32198=CARTESIAN_POINT('Ctrl Pts',(83.1422098352473,-12.6971950976412,10.1502287241044));
#32199=CARTESIAN_POINT('Ctrl Pts',(83.3754581634701,-15.522088392645,4.8081952387983));
#32200=CARTESIAN_POINT('Ctrl Pts',(83.6085992893649,-16.1966474690964,-1.19488542166675));
#32201=CARTESIAN_POINT('Ctrl Pts',(83.8416352233784,-14.6339538883274,-7.02670369688337));
#32202=CARTESIAN_POINT('Ctrl Pts',(84.0745679545012,-11.0497598473816,-11.8824317127295));
#32203=CARTESIAN_POINT('Ctrl Pts',(84.3073996737489,-5.94248428783527,-15.09263970399));
#32204=CARTESIAN_POINT('Ctrl Pts',(84.540132268385,-0.0171665032603614,
-16.2129461632812));
#32205=CARTESIAN_POINT('Ctrl Pts',(84.7727680106188,5.90520262635639,-15.0923025294507));
#32206=CARTESIAN_POINT('Ctrl Pts',(85.0053088744204,11.0065171159269,-11.8864785100097));
#32207=CARTESIAN_POINT('Ctrl Pts',(85.2377570340819,14.5833427924651,-7.04062680693156));
#32208=CARTESIAN_POINT('Ctrl Pts',(85.4701144791861,16.1401640578478,-1.22533588346504));
#32209=CARTESIAN_POINT('Ctrl Pts',(85.7023835299595,15.4662929248669,4.7550040735545));
#32210=CARTESIAN_POINT('Ctrl Pts',(85.9345662446591,12.6553888178413,10.0730373304554));
#32211=CARTESIAN_POINT('Ctrl Pts',(86.1666649327954,8.09679983295076,13.9966583914468));
#32212=CARTESIAN_POINT('Ctrl Pts',(86.3986815381799,2.42358552200963,15.9794357678464));
#32213=CARTESIAN_POINT('Ctrl Pts',(86.6692750541127,-4.58486198073758,15.7239726419428));
#32214=CARTESIAN_POINT('Ctrl Pts',(86.9783943834765,-11.7499252678846,11.7698005968098));
#32215=CARTESIAN_POINT('Ctrl Pts',(87.3259902517892,-16.2024151439095,3.70954956442589));
#32216=CARTESIAN_POINT('Ctrl Pts',(87.6734207471648,-15.6862303609498,-5.47622167055361));
#32217=CARTESIAN_POINT('Ctrl Pts',(88.0207132272952,-10.3628479251535,-12.9771513909202));
#32218=CARTESIAN_POINT('Ctrl Pts',(88.3678323138933,-1.8703041859877,-16.4954810466909));
#32219=CARTESIAN_POINT('Ctrl Pts',(88.7148821316246,7.193051660985,-14.9532751855446));
#32220=CARTESIAN_POINT('Ctrl Pts',(89.003856786706,12.8943942592402,-9.85553205895293));
#32221=CARTESIAN_POINT('Ctrl Pts',(89.2351907747089,15.3179503044652,-4.41141050395984));
#32222=CARTESIAN_POINT('Ctrl Pts',(89.3506074633962,15.7305922894428,-1.50774141983879));
#32223=CARTESIAN_POINT('Ctrl Pts',(89.4085387704217,15.7333741285005,-0.00740294277221285));
#32224=CARTESIAN_POINT('Origin',(89.18,16.5,-1.97064586870965E-14));
#32225=CARTESIAN_POINT('Origin',(89.18,16.5,-1.97064586870965E-14));
#32226=CARTESIAN_POINT('Origin',(68.82,16.5,-1.31470342757595E-16));
#32227=CARTESIAN_POINT('',(0.,0.,0.));
#32228=CARTESIAN_POINT('Origin',(0.,0.,0.));
#32229=CARTESIAN_POINT('',(1.79410756075087E-16,-1.84370575611634E-15,15.055));
#32230=CARTESIAN_POINT('Origin',(0.,-2.02311651219143E-15,16.52));
#32231=CARTESIAN_POINT('Origin',(-1.79410756075087E-16,0.,0.));
#32232=CARTESIAN_POINT('',(0.,0.,0.));
#32233=CARTESIAN_POINT('Origin',(0.99,0.,0.));
#32234=CARTESIAN_POINT('',(1.98,-15.06,-1.84431807951591E-15));
#32235=CARTESIAN_POINT('Origin',(1.98,0.,0.));
#32236=CARTESIAN_POINT('',(1.38777878078145E-16,-15.06,-1.84431807951591E-15));
#32237=CARTESIAN_POINT('',(0.99,-15.06,-1.84431807951591E-15));
#32238=CARTESIAN_POINT('Origin',(0.,0.,0.));
#32239=CARTESIAN_POINT('Origin',(0.,17.97,0.));
#32240=CARTESIAN_POINT('',(0.,-17.97,-2.20069029806779E-15));
#32241=CARTESIAN_POINT('Origin',(0.,0.,0.));
#32242=CARTESIAN_POINT('Origin',(0.99,0.,0.));
#32243=CARTESIAN_POINT('',(1.98,-17.97,-2.20069029806779E-15));
#32244=CARTESIAN_POINT('Origin',(1.98,0.,0.));
#32245=CARTESIAN_POINT('',(0.99,-17.97,-2.20069029806779E-15));
#32246=CARTESIAN_POINT('Origin',(1.98,15.06,0.));
#32247=CARTESIAN_POINT('',(0.,0.,0.));
#32248=CARTESIAN_POINT('Origin',(0.,2.8,0.));
#32249=CARTESIAN_POINT('',(1.73472347597681E-17,-2.8,-3.42901103761259E-16));
#32250=CARTESIAN_POINT('Origin',(0.,0.,0.));
#32251=CARTESIAN_POINT('Origin',(0.1,0.,0.));
#32252=CARTESIAN_POINT('',(0.2,-3.,-3.67394039744206E-16));
#32253=CARTESIAN_POINT('Origin',(0.2,0.,0.));
#32254=CARTESIAN_POINT('',(0.1,-2.9,-3.55147571752732E-16));
#32255=CARTESIAN_POINT('Origin',(2.5,0.,0.));
#32256=CARTESIAN_POINT('',(4.8,-3.,-3.67394039744206E-16));
#32257=CARTESIAN_POINT('Origin',(4.8,0.,0.));
#32258=CARTESIAN_POINT('',(2.5,-3.,-3.67394039744206E-16));
#32259=CARTESIAN_POINT('Origin',(4.9,0.,0.));
#32260=CARTESIAN_POINT('',(5.,-2.8,-3.42901103761259E-16));
#32261=CARTESIAN_POINT('Origin',(5.,0.,0.));
#32262=CARTESIAN_POINT('',(4.9,-2.9,-3.55147571752732E-16));
#32263=CARTESIAN_POINT('Origin',(5.,0.,0.));
#32264=CARTESIAN_POINT('',(0.,0.,0.));
#32265=CARTESIAN_POINT('Origin',(15.1767766952966,-15.,17.9267766952966));
#32266=CARTESIAN_POINT('',(15.,-14.5,17.5));
#32267=CARTESIAN_POINT('',(15.3535533905933,-14.8535533905933,18.3535533905933));
#32268=CARTESIAN_POINT('',(10.9776939607821,-10.4776939607822,7.78929420810503));
#32269=CARTESIAN_POINT('',(15.3535533905933,14.8535533905933,18.3535533905933));
#32270=CARTESIAN_POINT('',(15.3535533905933,-15.,18.3535533905933));
#32271=CARTESIAN_POINT('',(15.,14.5,17.5));
#32272=CARTESIAN_POINT('',(9.06160024732289,8.56160024732292,3.16343477829391));
#32273=CARTESIAN_POINT('',(15.,-15.,17.5));
#32274=CARTESIAN_POINT('Origin',(15.25,-14.75,-9.5));
#32275=CARTESIAN_POINT('',(15.,-14.5,-17.5));
#32276=CARTESIAN_POINT('',(15.,-14.5,-9.5));
#32277=CARTESIAN_POINT('',(15.3535533905933,-14.8535533905933,-18.3535533905933));
#32278=CARTESIAN_POINT('',(13.9074049329959,-13.4074049329959,-14.8622421710566));
#32279=CARTESIAN_POINT('',(15.5,-15.,-18.5));
#32280=CARTESIAN_POINT('',(13.9166666666667,-13.4166666666667,-16.9166666666667));
#32281=CARTESIAN_POINT('',(15.5,-15.,18.5));
#32282=CARTESIAN_POINT('',(15.5,-15.,-9.5));
#32283=CARTESIAN_POINT('',(10.75,-10.25,13.75));
#32284=CARTESIAN_POINT('Origin',(15.,-15.,-19.));
#32285=CARTESIAN_POINT('',(15.,14.5,-17.5));
#32286=CARTESIAN_POINT('',(15.,14.5,-9.5));
#32287=CARTESIAN_POINT('',(15.,-15.,-17.5));
#32288=CARTESIAN_POINT('Origin',(16.0732233047034,-15.,18.8232233047034));
#32289=CARTESIAN_POINT('',(16.5,14.5,19.));
#32290=CARTESIAN_POINT('',(15.6464466094067,14.8535533905933,18.6464466094067));
#32291=CARTESIAN_POINT('',(21.7161849536895,12.3393854483354,21.1606145516646));
#32292=CARTESIAN_POINT('',(15.6464466094067,-14.8535533905933,18.6464466094067));
#32293=CARTESIAN_POINT('',(15.6464466094067,-15.,18.6464466094067));
#32294=CARTESIAN_POINT('',(16.5,-14.5,19.));
#32295=CARTESIAN_POINT('',(17.0903255238784,-14.2554791617946,19.2445208382054));
#32296=CARTESIAN_POINT('',(16.5,-15.,19.));
#32297=CARTESIAN_POINT('Origin',(15.,-15.,19.));
#32298=CARTESIAN_POINT('',(29.5,-14.5,19.));
#32299=CARTESIAN_POINT('',(19.,-14.5,19.));
#32300=CARTESIAN_POINT('',(29.5,14.5,19.));
#32301=CARTESIAN_POINT('',(29.5,-15.,19.));
#32302=CARTESIAN_POINT('',(19.,14.5,19.));
#32303=CARTESIAN_POINT('Origin',(19.,-14.75,18.75));
#32304=CARTESIAN_POINT('',(16.1666666666667,-14.3333333333333,19.1666666666667));
#32305=CARTESIAN_POINT('',(30.5,-15.,18.5));
#32306=CARTESIAN_POINT('',(19.,-15.,18.5));
#32307=CARTESIAN_POINT('',(30.3535533905933,-14.8535533905933,18.6464466094067));
#32308=CARTESIAN_POINT('',(28.5,-13.,20.5));
#32309=CARTESIAN_POINT('',(25.9315911232999,-13.0219166471783,20.4780833528217));
#32310=CARTESIAN_POINT('Origin',(30.7834936490539,-15.,-3.58910161513776));
#32311=CARTESIAN_POINT('',(30.7834936490539,-14.7165063509461,-3.58910161513775));
#32312=CARTESIAN_POINT('',(31.,-14.5,-3.96410161513776));
#32313=CARTESIAN_POINT('',(28.4813466520527,-17.0186533479473,0.39833395016048));
#32314=CARTESIAN_POINT('',(31.,14.5,-3.96410161513776));
#32315=CARTESIAN_POINT('',(31.,-15.,-3.96410161513776));
#32316=CARTESIAN_POINT('',(30.7834936490539,14.7165063509461,-3.58910161513775));
#32317=CARTESIAN_POINT('',(31.4813466520527,14.0186533479473,-4.79781847254614));
#32318=CARTESIAN_POINT('',(30.5669872981078,14.5,-3.21410161513776));
#32319=CARTESIAN_POINT('',(27.0901923788647,11.0232050807569,2.80788383248868));
#32320=CARTESIAN_POINT('',(30.5669872981078,-14.5,-3.21410161513776));
#32321=CARTESIAN_POINT('',(30.5669872981078,-15.,-3.21410161513776));
#32322=CARTESIAN_POINT('',(30.0901923788647,-14.0232050807569,-2.38826859021799));
#32323=CARTESIAN_POINT('Origin',(31.,-15.,19.));
#32324=CARTESIAN_POINT('',(31.,-14.5,-17.5));
#32325=CARTESIAN_POINT('',(31.,-14.5,9.5));
#32326=CARTESIAN_POINT('',(31.,14.5,-17.5));
#32327=CARTESIAN_POINT('',(31.,-15.,-17.5));
#32328=CARTESIAN_POINT('',(31.,14.5,9.5));
#32329=CARTESIAN_POINT('Origin',(30.75,-14.75,9.5));
#32330=CARTESIAN_POINT('',(30.5,-15.,-3.75277674973256));
#32331=CARTESIAN_POINT('',(31.8538916194217,-13.6461083805783,-2.97110705880585));
#32332=CARTESIAN_POINT('',(30.5,-15.,-18.5));
#32333=CARTESIAN_POINT('',(30.5,-15.,9.5));
#32334=CARTESIAN_POINT('',(30.6464466094067,-14.8535533905933,-18.3535533905933));
#32335=CARTESIAN_POINT('',(35.25,-10.25,-13.75));
#32336=CARTESIAN_POINT('',(35.0223060392179,-10.4776939607821,-7.7892942081051));
#32337=CARTESIAN_POINT('Origin',(27.125,-14.75,-1.51554445662277));
#32338=CARTESIAN_POINT('',(28.,-14.5,-1.73205080756888));
#32339=CARTESIAN_POINT('',(27.25,-14.5,-1.29903810567666));
#32340=CARTESIAN_POINT('',(27.5,-15.,-2.02072594216369));
#32341=CARTESIAN_POINT('',(27.5,-15.,-2.02072594216369));
#32342=CARTESIAN_POINT('',(27.,-15.,-1.73205080756888));
#32343=CARTESIAN_POINT('Origin',(25.625,14.75,0.649519052838329));
#32344=CARTESIAN_POINT('',(27.5,15.,2.02072594216369));
#32345=CARTESIAN_POINT('',(30.5,15.,3.75277674973257));
#32346=CARTESIAN_POINT('',(25.5,15.,0.866025403784438));
#32347=CARTESIAN_POINT('',(30.7834936490539,14.7165063509461,3.58910161513776));
#32348=CARTESIAN_POINT('',(29.2889655234354,16.2110344765646,4.45196783077506));
#32349=CARTESIAN_POINT('',(30.5669872981078,14.5,3.21410161513775));
#32350=CARTESIAN_POINT('',(26.7901923788646,10.7232050807569,-3.32749907475928));
#32351=CARTESIAN_POINT('',(28.,14.5,1.73205080756888));
#32352=CARTESIAN_POINT('',(25.75,14.5,0.43301270189222));
#32353=CARTESIAN_POINT('',(28.,14.5,1.73205080756888));
#32354=CARTESIAN_POINT('Origin',(27.75,14.75,-0.866025403784439));
#32355=CARTESIAN_POINT('',(27.5,15.,-2.02072594216369));
#32356=CARTESIAN_POINT('',(27.5,15.,-0.866025403784439));
#32357=CARTESIAN_POINT('',(28.,14.5,-1.73205080756888));
#32358=CARTESIAN_POINT('',(28.,14.5,-0.866025403784439));
#32359=CARTESIAN_POINT('',(28.,14.5,-1.73205080756888));
#32360=CARTESIAN_POINT('Origin',(27.125,14.75,-1.51554445662277));
#32361=CARTESIAN_POINT('',(30.5,15.,-3.75277674973256));
#32362=CARTESIAN_POINT('',(31.8538916194217,13.6461083805783,-2.97110705880585));
#32363=CARTESIAN_POINT('',(27.,15.,-1.73205080756888));
#32364=CARTESIAN_POINT('',(27.25,14.5,-1.29903810567666));
#32365=CARTESIAN_POINT('Origin',(30.75,14.75,9.5));
#32366=CARTESIAN_POINT('',(30.5,15.,18.5));
#32367=CARTESIAN_POINT('',(30.5,15.,9.5));
#32368=CARTESIAN_POINT('',(30.6464466094067,14.8535533905933,18.3535533905933));
#32369=CARTESIAN_POINT('',(37.0833333333333,8.41666666666667,11.9166666666667));
#32370=CARTESIAN_POINT('',(31.,14.5,17.5));
#32371=CARTESIAN_POINT('',(34.0086887804634,11.4913112195366,10.2363827412455));
#32372=CARTESIAN_POINT('',(31.,14.5,3.96410161513775));
#32373=CARTESIAN_POINT('',(31.,14.5,9.5));
#32374=CARTESIAN_POINT('',(34.7722431864336,10.7277568135664,10.4978184725462));
#32375=CARTESIAN_POINT('Origin',(23.,15.,0.));
#32376=CARTESIAN_POINT('',(30.5,15.,-18.5));
#32377=CARTESIAN_POINT('',(30.5,15.,9.5));
#32378=CARTESIAN_POINT('',(15.5,15.,-18.5));
#32379=CARTESIAN_POINT('',(27.,15.,-18.5));
#32380=CARTESIAN_POINT('',(15.5,15.,18.5));
#32381=CARTESIAN_POINT('',(15.5,15.,-9.5));
#32382=CARTESIAN_POINT('',(19.,15.,18.5));
#32383=CARTESIAN_POINT('Origin',(30.75,14.75,9.5));
#32384=CARTESIAN_POINT('',(30.6464466094067,14.8535533905933,-18.3535533905933));
#32385=CARTESIAN_POINT('',(36.9383997526772,8.56160024732284,-3.16343477829394));
#32386=CARTESIAN_POINT('',(40.25,5.25000000000001,-8.74999999999999));
#32387=CARTESIAN_POINT('Origin',(16.0732233047034,-15.,-18.8232233047034));
#32388=CARTESIAN_POINT('',(16.5,-14.5,-19.));
#32389=CARTESIAN_POINT('',(15.6464466094067,-14.8535533905933,-18.6464466094067));
#32390=CARTESIAN_POINT('',(20.0684088767001,-13.0219166471783,-20.4780833528217));
#32391=CARTESIAN_POINT('',(15.6464466094067,14.8535533905933,-18.6464466094067));
#32392=CARTESIAN_POINT('',(15.6464466094067,-15.,-18.6464466094067));
#32393=CARTESIAN_POINT('',(16.5,14.5,-19.));
#32394=CARTESIAN_POINT('',(24.6942683065113,11.105822933719,-22.394177066281));
#32395=CARTESIAN_POINT('',(16.5,-15.,-19.));
#32396=CARTESIAN_POINT('Origin',(27.,-14.75,-18.75));
#32397=CARTESIAN_POINT('',(29.5,-14.5,-19.));
#32398=CARTESIAN_POINT('',(27.,-14.5,-19.));
#32399=CARTESIAN_POINT('',(30.3535533905933,-14.8535533905933,-18.6464466094067));
#32400=CARTESIAN_POINT('',(28.9096744761216,-14.2554791617946,-19.2445208382054));
#32401=CARTESIAN_POINT('',(29.8333333333333,-14.3333333333333,-19.1666666666667));
#32402=CARTESIAN_POINT('',(27.,-15.,-18.5));
#32403=CARTESIAN_POINT('',(17.5,-13.,-20.5));
#32404=CARTESIAN_POINT('Origin',(31.,-15.,-19.));
#32405=CARTESIAN_POINT('',(29.5,14.5,-19.));
#32406=CARTESIAN_POINT('',(27.,14.5,-19.));
#32407=CARTESIAN_POINT('',(29.5,-15.,-19.));
#32408=CARTESIAN_POINT('Origin',(15.1767766952966,-15.,-17.9267766952966));
#32409=CARTESIAN_POINT('',(15.3535533905933,14.8535533905933,-18.3535533905933));
#32410=CARTESIAN_POINT('',(11.9913112195367,11.4913112195367,-10.2363827412455));
#32411=CARTESIAN_POINT('',(15.3535533905933,-15.,-18.3535533905933));
#32412=CARTESIAN_POINT('Origin',(30.8232233047034,-15.,-17.9267766952966));
#32413=CARTESIAN_POINT('',(30.6464466094067,-15.,-18.3535533905933));
#32414=CARTESIAN_POINT('Origin',(30.5,-15.,-18.5));
#32415=CARTESIAN_POINT('',(30.3535533905933,14.8535533905933,-18.6464466094067));
#32416=CARTESIAN_POINT('',(30.3535533905933,-15.,-18.6464466094067));
#32417=CARTESIAN_POINT('',(24.8333333333333,9.33333333333336,-24.1666666666667));
#32418=CARTESIAN_POINT('Origin',(29.9267766952966,-15.,-18.8232233047034));
#32419=CARTESIAN_POINT('',(24.2838150463105,12.3393854483353,-21.1606145516647));
#32420=CARTESIAN_POINT('Origin',(25.625,-14.75,0.649519052838329));
#32421=CARTESIAN_POINT('',(28.,-14.5,1.73205080756888));
#32422=CARTESIAN_POINT('',(30.5669872981078,-14.5,3.21410161513775));
#32423=CARTESIAN_POINT('',(25.75,-14.5,0.43301270189222));
#32424=CARTESIAN_POINT('',(30.7834936490539,-14.7165063509461,3.58910161513775));
#32425=CARTESIAN_POINT('',(29.7901923788647,-13.7232050807569,1.86865334794731));
#32426=CARTESIAN_POINT('',(30.5,-15.,3.75277674973257));
#32427=CARTESIAN_POINT('',(29.2889655234354,-16.2110344765646,4.45196783077506));
#32428=CARTESIAN_POINT('',(27.5,-15.,2.02072594216369));
#32429=CARTESIAN_POINT('',(25.5,-15.,0.866025403784438));
#32430=CARTESIAN_POINT('',(27.5,-15.,2.02072594216369));
#32431=CARTESIAN_POINT('Origin',(27.75,-14.75,-0.866025403784439));
#32432=CARTESIAN_POINT('',(27.5,-15.,-0.866025403784439));
#32433=CARTESIAN_POINT('',(28.,-14.5,-0.866025403784439));
#32434=CARTESIAN_POINT('Origin',(23.,-15.,0.));
#32435=CARTESIAN_POINT('',(30.5,-15.,9.5));
#32436=CARTESIAN_POINT('',(22.1377898454666,-15.,-2.68587995320559));
#32437=CARTESIAN_POINT('',(21.7858117520809,-15.,-2.59788546711206));
#32438=CARTESIAN_POINT('Ctrl Pts',(22.1377898454666,-15.,-2.68587995320559));
#32439=CARTESIAN_POINT('Ctrl Pts',(21.9311050772667,-15.,-2.6388131454587));
#32440=CARTESIAN_POINT('Ctrl Pts',(21.7858117520809,-15.,-2.59788546711206));
#32441=CARTESIAN_POINT('',(19.5,-15.,-1.96145985275507));
#32442=CARTESIAN_POINT('',(22.0135911285113,-15.,-2.66130478825719));
#32443=CARTESIAN_POINT('',(19.5,-15.,-1.55627567321062));
#32444=CARTESIAN_POINT('',(19.5,-15.,-0.980729926377535));
#32445=CARTESIAN_POINT('',(22.5000001192093,-15.,-0.760232009924948));
#32446=CARTESIAN_POINT('',(21.3277838813459,-15.,-1.07127710028236));
#32447=CARTESIAN_POINT('',(22.5000001192093,-15.,-1.16746257990599));
#32448=CARTESIAN_POINT('',(22.5000001192093,-15.,-0.380116004962474));
#32449=CARTESIAN_POINT('',(20.5334244370461,-15.,-1.62380639463663));
#32450=CARTESIAN_POINT('',(22.8657597569362,-15.,-1.08258806942125));
#32451=CARTESIAN_POINT('',(19.9195088148117,-15.,-1.75068225711584));
#32452=CARTESIAN_POINT('Ctrl Pts',(20.5334244370461,-15.,-1.62380639463663));
#32453=CARTESIAN_POINT('Ctrl Pts',(20.2244202494621,-15.,-1.69747624546289));
#32454=CARTESIAN_POINT('Ctrl Pts',(19.9195088148117,-15.,-1.75068225711584));
#32455=CARTESIAN_POINT('',(20.4740790724754,-15.,-1.88574362546206));
#32456=CARTESIAN_POINT('Ctrl Pts',(19.9195088148117,-15.,-1.75068225711584));
#32457=CARTESIAN_POINT('Ctrl Pts',(20.4004092216492,-15.,-1.86527978628874));
#32458=CARTESIAN_POINT('Ctrl Pts',(20.4740790724754,-15.,-1.88574362546206));
#32459=CARTESIAN_POINT('',(22.5000001192093,-15.,-2.45668489485979));
#32460=CARTESIAN_POINT('',(21.3979462915622,-15.,-2.14610615225978));
#32461=CARTESIAN_POINT('',(22.5000001192093,-15.,-2.9355389252305));
#32462=CARTESIAN_POINT('',(22.5000001192093,-15.,-1.2283424474299));
#32463=CARTESIAN_POINT('',(20.9815825223923,-15.,-3.36527977138758));
#32464=CARTESIAN_POINT('',(23.1160603005779,-15.,-2.7611822632819));
#32465=CARTESIAN_POINT('',(19.9195088148117,-15.,-3.59856758266687));
#32466=CARTESIAN_POINT('Ctrl Pts',(20.9815825223923,-15.,-3.36527977138758));
#32467=CARTESIAN_POINT('Ctrl Pts',(20.4167805314064,-15.,-3.52694425731897));
#32468=CARTESIAN_POINT('Ctrl Pts',(19.9195088148117,-15.,-3.59856758266687));
#32469=CARTESIAN_POINT('',(20.5723057389259,-15.,-3.74795380979776));
#32470=CARTESIAN_POINT('Ctrl Pts',(19.9195088148117,-15.,-3.59856758266687));
#32471=CARTESIAN_POINT('Ctrl Pts',(20.2039561867714,-15.,-3.65586642175913));
#32472=CARTESIAN_POINT('Ctrl Pts',(20.5723057389259,-15.,-3.74795380979776));
#32473=CARTESIAN_POINT('',(22.5000001192093,-15.,-4.21862218528986));
#32474=CARTESIAN_POINT('',(21.2860505117679,-15.,-3.92222266495732));
#32475=CARTESIAN_POINT('',(22.5000001192093,-15.,-4.61766723543406));
#32476=CARTESIAN_POINT('',(22.5000001192093,-15.,-2.10931109264493));
#32477=CARTESIAN_POINT('',(19.5,-15.,-3.79502061754465));
#32478=CARTESIAN_POINT('',(22.1436755540772,-15.,-4.51995750652441));
#32479=CARTESIAN_POINT('',(19.5,-15.,-3.41234657913446));
#32480=CARTESIAN_POINT('',(19.5,-15.,-1.89751030877233));
#32481=CARTESIAN_POINT('',(21.7858117520809,-15.,-2.78001371771097));
#32482=CARTESIAN_POINT('',(21.5640325293677,-15.,-2.84136535367788));
#32483=CARTESIAN_POINT('Ctrl Pts',(21.7858117520809,-15.,-2.78001371771097));
#32484=CARTESIAN_POINT('Ctrl Pts',(22.0723055005074,-15.,-2.70020473748446));
#32485=CARTESIAN_POINT('Ctrl Pts',(22.1377898454666,-15.,-2.68587995320559));
#32486=CARTESIAN_POINT('',(20.4085947275162,-15.,0.0992497429251671));
#32487=CARTESIAN_POINT('',(20.4085947275162,-15.,1.3536836579442));
#32488=CARTESIAN_POINT('',(20.4085947275162,-15.,0.0496248714625835));
#32489=CARTESIAN_POINT('',(19.5,-15.,1.68315164744854));
#32490=CARTESIAN_POINT('',(21.7706366750829,-15.,0.859789946594888));
#32491=CARTESIAN_POINT('',(19.5,-15.,2.10470690100919));
#32492=CARTESIAN_POINT('',(19.5,-15.,0.84157582372427));
#32493=CARTESIAN_POINT('',(22.5000001192093,-15.,0.952592231333256));
#32494=CARTESIAN_POINT('',(21.3772735898822,-15.,1.38376211569081));
#32495=CARTESIAN_POINT('',(22.5000001192093,-15.,0.524897836148739));
#32496=CARTESIAN_POINT('',(22.5000001192093,-15.,0.476296115666628));
#32497=CARTESIAN_POINT('',(19.5,-15.,-0.702932812273502));
#32498=CARTESIAN_POINT('',(22.6221283822359,-15.,0.574882108956754));
#32499=CARTESIAN_POINT('',(19.5,-15.,-0.250681973993778));
#32500=CARTESIAN_POINT('',(19.5,-15.,-0.351466406136751));
#32501=CARTESIAN_POINT('',(21.0659912340793,-15.,0.352436209092567));
#32502=CARTESIAN_POINT('',(19.6258525252342,-15.,3.89631662517786));
#32503=CARTESIAN_POINT('',(19.4488404393196,-15.,4.44167826324701));
#32504=CARTESIAN_POINT('Ctrl Pts',(19.6258525252342,-15.,3.89631662517786));
#32505=CARTESIAN_POINT('Ctrl Pts',(19.4488404393196,-15.,4.11221016198397));
#32506=CARTESIAN_POINT('Ctrl Pts',(19.4488404393196,-15.,4.44167826324701));
#32507=CARTESIAN_POINT('',(19.7598908543587,-15.,5.12312430888414));
#32508=CARTESIAN_POINT('Ctrl Pts',(19.4488404393196,-15.,4.44167826324701));
#32509=CARTESIAN_POINT('Ctrl Pts',(19.4488404393196,-15.,4.87551178783178));
#32510=CARTESIAN_POINT('Ctrl Pts',(19.7598908543587,-15.,5.12312430888414));
#32511=CARTESIAN_POINT('',(20.9795362949371,-15.,5.41985012590885));
#32512=CARTESIAN_POINT('Ctrl Pts',(19.7598908543587,-15.,5.12312430888414));
#32513=CARTESIAN_POINT('Ctrl Pts',(20.1343790888786,-15.,5.41985012590885));
#32514=CARTESIAN_POINT('Ctrl Pts',(20.9795362949371,-15.,5.41985012590885));
#32515=CARTESIAN_POINT('',(21.8359481990337,-15.,5.31036853790283));
#32516=CARTESIAN_POINT('Ctrl Pts',(20.9795362949371,-15.,5.41985012590885));
#32517=CARTESIAN_POINT('Ctrl Pts',(21.511596262455,-15.,5.41985012590885));
#32518=CARTESIAN_POINT('Ctrl Pts',(21.8359481990337,-15.,5.31036853790283));
#32519=CARTESIAN_POINT('',(22.3362894058228,-15.,4.9849933758378));
#32520=CARTESIAN_POINT('Ctrl Pts',(21.8359481990337,-15.,5.31036853790283));
#32521=CARTESIAN_POINT('Ctrl Pts',(22.1603001356125,-15.,5.20088694989681));
#32522=CARTESIAN_POINT('Ctrl Pts',(22.3362894058228,-15.,4.9849933758378));
#32523=CARTESIAN_POINT('',(22.5122783780098,-15.,4.44167826324701));
#32524=CARTESIAN_POINT('Ctrl Pts',(22.3362894058228,-15.,4.9849933758378));
#32525=CARTESIAN_POINT('Ctrl Pts',(22.5122783780098,-15.,4.7690998390317));
#32526=CARTESIAN_POINT('Ctrl Pts',(22.5122783780098,-15.,4.44167826324701));
#32527=CARTESIAN_POINT('',(22.4150751233101,-15.,4.01807654649019));
#32528=CARTESIAN_POINT('Ctrl Pts',(22.5122783780098,-15.,4.44167826324701));
#32529=CARTESIAN_POINT('Ctrl Pts',(22.5122783780098,-15.,4.2002047970891));
#32530=CARTESIAN_POINT('Ctrl Pts',(22.4150751233101,-15.,4.01807654649019));
#32531=CARTESIAN_POINT('',(22.1347205042839,-15.,3.71725801378489));
#32532=CARTESIAN_POINT('Ctrl Pts',(22.4150751233101,-15.,4.01807654649019));
#32533=CARTESIAN_POINT('Ctrl Pts',(22.3178718686104,-15.,3.83594829589128));
#32534=CARTESIAN_POINT('Ctrl Pts',(22.1347205042839,-15.,3.71725801378489));
#32535=CARTESIAN_POINT('',(21.6886084973812,-15.,3.53103701025248));
#32536=CARTESIAN_POINT('Ctrl Pts',(22.1347205042839,-15.,3.71725801378489));
#32537=CARTESIAN_POINT('Ctrl Pts',(21.9515691399574,-15.,3.59856758266687));
#32538=CARTESIAN_POINT('Ctrl Pts',(21.6886084973812,-15.,3.53103701025248));
#32539=CARTESIAN_POINT('',(20.9795362949371,-15.,3.46350628882647));
#32540=CARTESIAN_POINT('Ctrl Pts',(21.6886084973812,-15.,3.53103701025248));
#32541=CARTESIAN_POINT('Ctrl Pts',(21.4256481528282,-15.,3.46350628882647));
#32542=CARTESIAN_POINT('Ctrl Pts',(20.9795362949371,-15.,3.46350628882647));
#32543=CARTESIAN_POINT('',(20.1272169947624,-15.,3.57196468859911));
#32544=CARTESIAN_POINT('Ctrl Pts',(20.9795362949371,-15.,3.46350628882647));
#32545=CARTESIAN_POINT('Ctrl Pts',(20.4515687823296,-15.,3.46350628882647));
#32546=CARTESIAN_POINT('Ctrl Pts',(20.1272169947624,-15.,3.57196468859911));
#32547=CARTESIAN_POINT('Ctrl Pts',(20.1272169947624,-15.,3.57196468859911));
#32548=CARTESIAN_POINT('Ctrl Pts',(19.8028649091721,-15.,3.68042308837175));
#32549=CARTESIAN_POINT('Ctrl Pts',(19.6258525252342,-15.,3.89631662517786));
#32550=CARTESIAN_POINT('',(22.1111871004105,-15.,6.9280356541276));
#32551=CARTESIAN_POINT('',(22.5122783780098,-15.,6.60061407834291));
#32552=CARTESIAN_POINT('Ctrl Pts',(22.1111871004105,-15.,6.9280356541276));
#32553=CARTESIAN_POINT('Ctrl Pts',(22.3178718686104,-15.,6.69679414480925));
#32554=CARTESIAN_POINT('Ctrl Pts',(22.5122783780098,-15.,6.60061407834291));
#32555=CARTESIAN_POINT('',(22.5122783780098,-15.,6.3632333651185));
#32556=CARTESIAN_POINT('',(22.5122783780098,-15.,3.30030703917146));
#32557=CARTESIAN_POINT('',(19.5,-15.,6.3632333651185));
#32558=CARTESIAN_POINT('',(22.7561391890049,-15.,6.3632333651185));
#32559=CARTESIAN_POINT('',(19.5,-15.,6.73158269375563));
#32560=CARTESIAN_POINT('',(19.5,-15.,3.18161668255925));
#32561=CARTESIAN_POINT('',(21.8472033441067,-15.,6.73158269375563));
#32562=CARTESIAN_POINT('',(21.25,-15.,6.73158269375563));
#32563=CARTESIAN_POINT('',(21.5934516191483,-15.,7.080491296947));
#32564=CARTESIAN_POINT('Ctrl Pts',(21.8472033441067,-15.,6.73158269375563));
#32565=CARTESIAN_POINT('Ctrl Pts',(21.7203274071217,-15.,6.86459768563509));
#32566=CARTESIAN_POINT('Ctrl Pts',(21.5934516191483,-15.,7.080491296947));
#32567=CARTESIAN_POINT('',(21.4031378626823,-15.,7.46828120201826));
#32568=CARTESIAN_POINT('Ctrl Pts',(21.5934516191483,-15.,7.080491296947));
#32569=CARTESIAN_POINT('Ctrl Pts',(21.4665756821632,-15.,7.29638490825891));
#32570=CARTESIAN_POINT('Ctrl Pts',(21.4031378626823,-15.,7.46828120201826));
#32571=CARTESIAN_POINT('',(21.7592087090015,-15.,7.46828120201826));
#32572=CARTESIAN_POINT('',(22.2015689313412,-15.,7.46828120201826));
#32573=CARTESIAN_POINT('Ctrl Pts',(21.7592087090015,-15.,7.46828120201826));
#32574=CARTESIAN_POINT('Ctrl Pts',(21.9045020341873,-15.,7.15927708894014));
#32575=CARTESIAN_POINT('Ctrl Pts',(22.1111871004105,-15.,6.9280356541276));
#32576=CARTESIAN_POINT('',(19.9062074422836,-15.,-6.90143261104822));
#32577=CARTESIAN_POINT('',(20.1180080771446,-15.,-7.27387461811304));
#32578=CARTESIAN_POINT('Ctrl Pts',(19.9062074422836,-15.,-6.90143261104822));
#32579=CARTESIAN_POINT('Ctrl Pts',(20.0054569244385,-15.,-7.14699868112802));
#32580=CARTESIAN_POINT('Ctrl Pts',(20.1180080771446,-15.,-7.27387461811304));
#32581=CARTESIAN_POINT('',(20.6766710877419,-15.,-7.27387461811304));
#32582=CARTESIAN_POINT('',(21.5590040385723,-15.,-7.27387461811304));
#32583=CARTESIAN_POINT('',(20.6766710877419,-15.,-6.39188278466463));
#32584=CARTESIAN_POINT('',(20.6766710877419,-15.,-3.63693730905652));
#32585=CARTESIAN_POINT('',(21.0286494791508,-15.,-6.39188278466463));
#32586=CARTESIAN_POINT('',(21.8383355438709,-15.,-6.39188278466463));
#32587=CARTESIAN_POINT('',(21.0306958556175,-15.,-7.66268793493509));
#32588=CARTESIAN_POINT('',(21.0235056266662,-15.,-3.19753690751813));
#32589=CARTESIAN_POINT('',(19.9174625873566,-15.,-7.66268793493509));
#32590=CARTESIAN_POINT('',(22.0153479278088,-15.,-7.66268793493509));
#32591=CARTESIAN_POINT('',(19.5665074586868,-15.,-7.0590041950345));
#32592=CARTESIAN_POINT('Ctrl Pts',(19.9174625873566,-15.,-7.66268793493509));
#32593=CARTESIAN_POINT('Ctrl Pts',(19.684174478054,-15.,-7.37005475908518));
#32594=CARTESIAN_POINT('Ctrl Pts',(19.5665074586868,-15.,-7.0590041950345));
#32595=CARTESIAN_POINT('',(19.4488404393196,-15.,-6.42053220421076));
#32596=CARTESIAN_POINT('Ctrl Pts',(19.5665074586868,-15.,-7.0590041950345));
#32597=CARTESIAN_POINT('Ctrl Pts',(19.4488404393196,-15.,-6.74795377999544));
#32598=CARTESIAN_POINT('Ctrl Pts',(19.4488404393196,-15.,-6.42053220421076));
#32599=CARTESIAN_POINT('',(19.638131082058,-15.,-5.61732616275549));
#32600=CARTESIAN_POINT('Ctrl Pts',(19.4488404393196,-15.,-6.42053220421076));
#32601=CARTESIAN_POINT('Ctrl Pts',(19.4488404393196,-15.,-5.97851309925318));
#32602=CARTESIAN_POINT('Ctrl Pts',(19.638131082058,-15.,-5.61732616275549));
#32603=CARTESIAN_POINT('',(20.1855389475822,-15.,-5.07196459919214));
#32604=CARTESIAN_POINT('Ctrl Pts',(19.638131082058,-15.,-5.61732616275549));
#32605=CARTESIAN_POINT('Ctrl Pts',(19.8274214267731,-15.,-5.2561392262578));
#32606=CARTESIAN_POINT('Ctrl Pts',(20.1855389475822,-15.,-5.07196459919214));
#32607=CARTESIAN_POINT('',(20.9856754243374,-15.,-4.88778999075293));
#32608=CARTESIAN_POINT('Ctrl Pts',(20.1855389475822,-15.,-5.07196459919214));
#32609=CARTESIAN_POINT('Ctrl Pts',(20.5436561703682,-15.,-4.88778999075293));
#32610=CARTESIAN_POINT('Ctrl Pts',(20.9856754243374,-15.,-4.88778999075293));
#32611=CARTESIAN_POINT('',(21.8032061755657,-15.,-5.07094141095877));
#32612=CARTESIAN_POINT('Ctrl Pts',(20.9856754243374,-15.,-4.88778999075293));
#32613=CARTESIAN_POINT('Ctrl Pts',(21.4236017763615,-15.,-4.88778999075293));
#32614=CARTESIAN_POINT('Ctrl Pts',(21.8032061755657,-15.,-5.07094141095877));
#32615=CARTESIAN_POINT('',(22.3669852018356,-15.,-5.59788551181555));
#32616=CARTESIAN_POINT('Ctrl Pts',(21.8032061755657,-15.,-5.07094141095877));
#32617=CARTESIAN_POINT('Ctrl Pts',(22.1828104257584,-15.,-5.25409284979105));
#32618=CARTESIAN_POINT('Ctrl Pts',(22.3669852018356,-15.,-5.59788551181555));
#32619=CARTESIAN_POINT('',(22.5511596798897,-15.,-6.38983640819788));
#32620=CARTESIAN_POINT('Ctrl Pts',(22.3669852018356,-15.,-5.59788551181555));
#32621=CARTESIAN_POINT('Ctrl Pts',(22.5511596798897,-15.,-5.94167817384004));
#32622=CARTESIAN_POINT('Ctrl Pts',(22.5511596798897,-15.,-6.38983640819788));
#32623=CARTESIAN_POINT('',(22.445770919323,-15.,-6.9781719520688));
#32624=CARTESIAN_POINT('Ctrl Pts',(22.5511596798897,-15.,-6.38983640819788));
#32625=CARTESIAN_POINT('Ctrl Pts',(22.5511596798897,-15.,-6.71521160751581));
#32626=CARTESIAN_POINT('Ctrl Pts',(22.445770919323,-15.,-6.9781719520688));
#32627=CARTESIAN_POINT('',(22.1521146297455,-15.,-7.39051882177591));
#32628=CARTESIAN_POINT('Ctrl Pts',(22.445770919323,-15.,-6.9781719520688));
#32629=CARTESIAN_POINT('Ctrl Pts',(22.3403821587563,-15.,-7.24113259464502));
#32630=CARTESIAN_POINT('Ctrl Pts',(22.1521146297455,-15.,-7.39051882177591));
#32631=CARTESIAN_POINT('',(21.6609823405743,-15.,-7.61766735464334));
#32632=CARTESIAN_POINT('Ctrl Pts',(22.1521146297455,-15.,-7.39051882177591));
#32633=CARTESIAN_POINT('Ctrl Pts',(21.9638473987579,-15.,-7.53990475088358));
#32634=CARTESIAN_POINT('Ctrl Pts',(21.6609823405743,-15.,-7.61766735464334));
#32635=CARTESIAN_POINT('',(21.562755972147,-15.,-7.25955013185739));
#32636=CARTESIAN_POINT('',(20.7362158118188,-15.,-4.2461203219493));
#32637=CARTESIAN_POINT('',(21.9229195713997,-15.,-7.09174636751413));
#32638=CARTESIAN_POINT('Ctrl Pts',(21.562755972147,-15.,-7.25955013185739));
#32639=CARTESIAN_POINT('Ctrl Pts',(21.7919510304928,-15.,-7.19201926141977));
#32640=CARTESIAN_POINT('Ctrl Pts',(21.9229195713997,-15.,-7.09174636751413));
#32641=CARTESIAN_POINT('',(22.1326739788055,-15.,-6.80525247007608));
#32642=CARTESIAN_POINT('Ctrl Pts',(21.9229195713997,-15.,-7.09174636751413));
#32643=CARTESIAN_POINT('Ctrl Pts',(22.0538882613182,-15.,-6.99147347360849));
#32644=CARTESIAN_POINT('Ctrl Pts',(22.1326739788055,-15.,-6.80525247007608));
#32645=CARTESIAN_POINT('',(22.2114599943161,-15.,-6.39188278466463));
#32646=CARTESIAN_POINT('Ctrl Pts',(22.1326739788055,-15.,-6.80525247007608));
#32647=CARTESIAN_POINT('Ctrl Pts',(22.2114599943161,-15.,-6.61903146654367));
#32648=CARTESIAN_POINT('Ctrl Pts',(22.2114599943161,-15.,-6.39188278466463));
#32649=CARTESIAN_POINT('',(22.128581225872,-15.,-5.92121426016092));
#32650=CARTESIAN_POINT('Ctrl Pts',(22.2114599943161,-15.,-6.39188278466463));
#32651=CARTESIAN_POINT('Ctrl Pts',(22.2114599943161,-15.,-6.11971367150545));
#32652=CARTESIAN_POINT('Ctrl Pts',(22.128581225872,-15.,-5.92121426016092));
#32653=CARTESIAN_POINT('',(21.9106413125992,-15.,-5.60095507651567));
#32654=CARTESIAN_POINT('Ctrl Pts',(22.128581225872,-15.,-5.92121426016092));
#32655=CARTESIAN_POINT('Ctrl Pts',(22.0457027554512,-15.,-5.7227149233222));
#32656=CARTESIAN_POINT('Ctrl Pts',(21.9106413125992,-15.,-5.60095507651567));
#32657=CARTESIAN_POINT('',(21.6139155328274,-15.,-5.41166450828314));
#32658=CARTESIAN_POINT('Ctrl Pts',(21.9106413125992,-15.,-5.60095507651567));
#32659=CARTESIAN_POINT('Ctrl Pts',(21.7755798697472,-15.,-5.47919515520334));
#32660=CARTESIAN_POINT('Ctrl Pts',(21.6139155328274,-15.,-5.41166450828314));
#32661=CARTESIAN_POINT('',(21.0102319419384,-15.,-5.29706697911024));
#32662=CARTESIAN_POINT('Ctrl Pts',(21.6139155328274,-15.,-5.41166450828314));
#32663=CARTESIAN_POINT('Ctrl Pts',(21.3356071412563,-15.,-5.29706697911024));
#32664=CARTESIAN_POINT('Ctrl Pts',(21.0102319419384,-15.,-5.29706697911024));
#32665=CARTESIAN_POINT('',(20.3390176296234,-15.,-5.43519791215658));
#32666=CARTESIAN_POINT('Ctrl Pts',(21.0102319419384,-15.,-5.29706697911024));
#32667=CARTESIAN_POINT('Ctrl Pts',(20.6091405153275,-15.,-5.29706697911024));
#32668=CARTESIAN_POINT('Ctrl Pts',(20.3390176296234,-15.,-5.43519791215658));
#32669=CARTESIAN_POINT('',(19.9379263520241,-15.,-5.8373125270009));
#32670=CARTESIAN_POINT('Ctrl Pts',(20.3390176296234,-15.,-5.43519791215658));
#32671=CARTESIAN_POINT('Ctrl Pts',(20.0688950419426,-15.,-5.57332884520292));
#32672=CARTESIAN_POINT('Ctrl Pts',(19.9379263520241,-15.,-5.8373125270009));
#32673=CARTESIAN_POINT('',(19.8069576621056,-15.,-6.39802191406488));
#32674=CARTESIAN_POINT('Ctrl Pts',(19.9379263520241,-15.,-5.8373125270009));
#32675=CARTESIAN_POINT('Ctrl Pts',(19.8069576621056,-15.,-6.10129613429308));
#32676=CARTESIAN_POINT('Ctrl Pts',(19.8069576621056,-15.,-6.39802191406488));
#32677=CARTESIAN_POINT('Ctrl Pts',(19.8069576621056,-15.,-6.39802191406488));
#32678=CARTESIAN_POINT('Ctrl Pts',(19.8069576621056,-15.,-6.6558663919568));
#32679=CARTESIAN_POINT('Ctrl Pts',(19.9062074422836,-15.,-6.90143261104822));
#32680=CARTESIAN_POINT('Origin',(30.75,-14.75,9.5));
#32681=CARTESIAN_POINT('',(31.,-14.5,3.96410161513775));
#32682=CARTESIAN_POINT('',(31.7722431864335,-13.7277568135665,5.30166604983953));
#32683=CARTESIAN_POINT('',(31.,-14.5,17.5));
#32684=CARTESIAN_POINT('',(31.,-14.5,9.5));
#32685=CARTESIAN_POINT('',(30.6464466094067,-14.8535533905933,18.3535533905933));
#32686=CARTESIAN_POINT('',(32.0925950670041,-13.4074049329959,14.8622421710567));
#32687=CARTESIAN_POINT('',(32.0833333333333,-13.4166666666667,16.9166666666667));
#32688=CARTESIAN_POINT('Origin',(30.7834936490539,-15.,3.58910161513775));
#32689=CARTESIAN_POINT('',(31.,-15.,3.96410161513775));
#32690=CARTESIAN_POINT('',(30.5669872981078,-15.,3.21410161513775));
#32691=CARTESIAN_POINT('Origin',(31.,-15.,19.));
#32692=CARTESIAN_POINT('',(31.,-15.,17.5));
#32693=CARTESIAN_POINT('Origin',(29.9267766952966,-15.,18.8232233047034));
#32694=CARTESIAN_POINT('',(30.3535533905933,14.8535533905933,18.6464466094067));
#32695=CARTESIAN_POINT('',(30.3535533905933,-15.,18.6464466094067));
#32696=CARTESIAN_POINT('',(21.3057316934887,11.105822933719,22.394177066281));
#32697=CARTESIAN_POINT('Origin',(19.,14.75,18.75));
#32698=CARTESIAN_POINT('',(23.5,8.00000000000003,25.5));
#32699=CARTESIAN_POINT('',(21.1666666666667,9.33333333333336,24.1666666666667));
#32700=CARTESIAN_POINT('Origin',(30.5,-15.,18.5));
#32701=CARTESIAN_POINT('',(30.6464466094067,-15.,18.3535533905933));
#32702=CARTESIAN_POINT('Origin',(30.8232233047034,-15.,17.9267766952966));
#32703=CARTESIAN_POINT('Ctrl Pts',(22.1377898454666,-15.,-2.68587995320559));
#32704=CARTESIAN_POINT('Ctrl Pts',(22.1377898454666,-14.75,-2.68587995320559));
#32705=CARTESIAN_POINT('Ctrl Pts',(21.9311050772667,-15.,-2.6388131454587));
#32706=CARTESIAN_POINT('Ctrl Pts',(21.9311050772667,-14.75,-2.6388131454587));
#32707=CARTESIAN_POINT('Ctrl Pts',(21.7858117520809,-15.,-2.59788546711206));
#32708=CARTESIAN_POINT('Ctrl Pts',(21.7858117520809,-14.75,-2.59788546711206));
#32709=CARTESIAN_POINT('',(22.1377898454666,-14.75,-2.68587995320559));
#32710=CARTESIAN_POINT('',(22.1377898454666,-15.,-2.68587995320559));
#32711=CARTESIAN_POINT('',(21.7858117520809,-14.75,-2.59788546711206));
#32712=CARTESIAN_POINT('Ctrl Pts',(22.1377898454666,-14.75,-2.68587995320559));
#32713=CARTESIAN_POINT('Ctrl Pts',(21.9311050772667,-14.75,-2.6388131454587));
#32714=CARTESIAN_POINT('Ctrl Pts',(21.7858117520809,-14.75,-2.59788546711206));
#32715=CARTESIAN_POINT('',(21.7858117520809,-15.,-2.59788546711206));
#32716=CARTESIAN_POINT('Ctrl Pts',(21.7858117520809,-15.,-2.78001371771097));
#32717=CARTESIAN_POINT('Ctrl Pts',(21.7858117520809,-14.75,-2.78001371771097));
#32718=CARTESIAN_POINT('Ctrl Pts',(22.0723055005074,-15.,-2.70020473748446));
#32719=CARTESIAN_POINT('Ctrl Pts',(22.0723055005074,-14.75,-2.70020473748446));
#32720=CARTESIAN_POINT('Ctrl Pts',(22.1377898454666,-15.,-2.68587995320559));
#32721=CARTESIAN_POINT('Ctrl Pts',(22.1377898454666,-14.75,-2.68587995320559));
#32722=CARTESIAN_POINT('',(21.7858117520809,-14.75,-2.78001371771097));
#32723=CARTESIAN_POINT('',(21.7858117520809,-15.,-2.78001371771097));
#32724=CARTESIAN_POINT('Ctrl Pts',(21.7858117520809,-14.75,-2.78001371771097));
#32725=CARTESIAN_POINT('Ctrl Pts',(22.0723055005074,-14.75,-2.70020473748446));
#32726=CARTESIAN_POINT('Ctrl Pts',(22.1377898454666,-14.75,-2.68587995320559));
#32727=CARTESIAN_POINT('Origin',(19.5,-15.,-3.41234657913446));
#32728=CARTESIAN_POINT('',(19.5,-14.75,-3.41234657913446));
#32729=CARTESIAN_POINT('',(19.5,-15.,-3.41234657913446));
#32730=CARTESIAN_POINT('',(19.5,-14.75,-3.41234657913446));
#32731=CARTESIAN_POINT('Origin',(19.5,-15.,-3.79502061754465));
#32732=CARTESIAN_POINT('',(19.5,-14.75,-3.79502061754465));
#32733=CARTESIAN_POINT('',(19.5,-15.,-3.79502061754465));
#32734=CARTESIAN_POINT('',(19.5,-14.75,-3.79502061754465));
#32735=CARTESIAN_POINT('Origin',(22.5000001192093,-15.,-4.61766723543406));
#32736=CARTESIAN_POINT('',(22.5000001192093,-14.75,-4.61766723543406));
#32737=CARTESIAN_POINT('',(22.5000001192093,-15.,-4.61766723543406));
#32738=CARTESIAN_POINT('',(22.5000001192093,-14.75,-4.61766723543406));
#32739=CARTESIAN_POINT('Origin',(22.5000001192093,-15.,-4.21862218528986));
#32740=CARTESIAN_POINT('',(22.5000001192093,-14.75,-4.21862218528986));
#32741=CARTESIAN_POINT('',(22.5000001192093,-15.,-4.21862218528986));
#32742=CARTESIAN_POINT('',(22.5000001192093,-14.75,-4.21862218528986));
#32743=CARTESIAN_POINT('Origin',(20.5723057389259,-15.,-3.74795380979776));
#32744=CARTESIAN_POINT('',(20.5723057389259,-14.75,-3.74795380979776));
#32745=CARTESIAN_POINT('',(20.5723057389259,-15.,-3.74795380979776));
#32746=CARTESIAN_POINT('',(20.5723057389259,-14.75,-3.74795380979776));
#32747=CARTESIAN_POINT('Ctrl Pts',(19.9195088148117,-15.,-3.59856758266687));
#32748=CARTESIAN_POINT('Ctrl Pts',(19.9195088148117,-14.75,-3.59856758266687));
#32749=CARTESIAN_POINT('Ctrl Pts',(20.2039561867714,-15.,-3.65586642175913));
#32750=CARTESIAN_POINT('Ctrl Pts',(20.2039561867714,-14.75,-3.65586642175913));
#32751=CARTESIAN_POINT('Ctrl Pts',(20.5723057389259,-15.,-3.74795380979776));
#32752=CARTESIAN_POINT('Ctrl Pts',(20.5723057389259,-14.75,-3.74795380979776));
#32753=CARTESIAN_POINT('',(19.9195088148117,-14.75,-3.59856758266687));
#32754=CARTESIAN_POINT('',(19.9195088148117,-15.,-3.59856758266687));
#32755=CARTESIAN_POINT('Ctrl Pts',(19.9195088148117,-14.75,-3.59856758266687));
#32756=CARTESIAN_POINT('Ctrl Pts',(20.2039561867714,-14.75,-3.65586642175913));
#32757=CARTESIAN_POINT('Ctrl Pts',(20.5723057389259,-14.75,-3.74795380979776));
#32758=CARTESIAN_POINT('Ctrl Pts',(20.9815825223923,-15.,-3.36527977138758));
#32759=CARTESIAN_POINT('Ctrl Pts',(20.9815825223923,-14.75,-3.36527977138758));
#32760=CARTESIAN_POINT('Ctrl Pts',(20.4167805314064,-15.,-3.52694425731897));
#32761=CARTESIAN_POINT('Ctrl Pts',(20.4167805314064,-14.75,-3.52694425731897));
#32762=CARTESIAN_POINT('Ctrl Pts',(19.9195088148117,-15.,-3.59856758266687));
#32763=CARTESIAN_POINT('Ctrl Pts',(19.9195088148117,-14.75,-3.59856758266687));
#32764=CARTESIAN_POINT('',(20.9815825223923,-14.75,-3.36527977138758));
#32765=CARTESIAN_POINT('',(20.9815825223923,-15.,-3.36527977138758));
#32766=CARTESIAN_POINT('Ctrl Pts',(20.9815825223923,-14.75,-3.36527977138758));
#32767=CARTESIAN_POINT('Ctrl Pts',(20.4167805314064,-14.75,-3.52694425731897));
#32768=CARTESIAN_POINT('Ctrl Pts',(19.9195088148117,-14.75,-3.59856758266687));
#32769=CARTESIAN_POINT('Origin',(22.5000001192093,-15.,-2.9355389252305));
#32770=CARTESIAN_POINT('',(22.5000001192093,-14.75,-2.9355389252305));
#32771=CARTESIAN_POINT('',(22.5000001192093,-15.,-2.9355389252305));
#32772=CARTESIAN_POINT('',(22.5000001192093,-14.75,-2.9355389252305));
#32773=CARTESIAN_POINT('Origin',(22.5000001192093,-15.,-2.45668489485979));
#32774=CARTESIAN_POINT('',(22.5000001192093,-14.75,-2.45668489485979));
#32775=CARTESIAN_POINT('',(22.5000001192093,-15.,-2.45668489485979));
#32776=CARTESIAN_POINT('',(22.5000001192093,-14.75,-2.45668489485979));
#32777=CARTESIAN_POINT('Origin',(20.4740790724754,-15.,-1.88574362546206));
#32778=CARTESIAN_POINT('',(20.4740790724754,-14.75,-1.88574362546206));
#32779=CARTESIAN_POINT('',(20.4740790724754,-15.,-1.88574362546206));
#32780=CARTESIAN_POINT('',(20.4740790724754,-14.75,-1.88574362546206));
#32781=CARTESIAN_POINT('Ctrl Pts',(19.9195088148117,-15.,-1.75068225711584));
#32782=CARTESIAN_POINT('Ctrl Pts',(19.9195088148117,-14.75,-1.75068225711584));
#32783=CARTESIAN_POINT('Ctrl Pts',(20.4004092216492,-15.,-1.86527978628874));
#32784=CARTESIAN_POINT('Ctrl Pts',(20.4004092216492,-14.75,-1.86527978628874));
#32785=CARTESIAN_POINT('Ctrl Pts',(20.4740790724754,-15.,-1.88574362546206));
#32786=CARTESIAN_POINT('Ctrl Pts',(20.4740790724754,-14.75,-1.88574362546206));
#32787=CARTESIAN_POINT('',(19.9195088148117,-14.75,-1.75068225711584));
#32788=CARTESIAN_POINT('',(19.9195088148117,-15.,-1.75068225711584));
#32789=CARTESIAN_POINT('Ctrl Pts',(19.9195088148117,-14.75,-1.75068225711584));
#32790=CARTESIAN_POINT('Ctrl Pts',(20.4004092216492,-14.75,-1.86527978628874));
#32791=CARTESIAN_POINT('Ctrl Pts',(20.4740790724754,-14.75,-1.88574362546206));
#32792=CARTESIAN_POINT('Ctrl Pts',(20.5334244370461,-15.,-1.62380639463663));
#32793=CARTESIAN_POINT('Ctrl Pts',(20.5334244370461,-14.75,-1.62380639463663));
#32794=CARTESIAN_POINT('Ctrl Pts',(20.2244202494621,-15.,-1.69747624546289));
#32795=CARTESIAN_POINT('Ctrl Pts',(20.2244202494621,-14.75,-1.69747624546289));
#32796=CARTESIAN_POINT('Ctrl Pts',(19.9195088148117,-15.,-1.75068225711584));
#32797=CARTESIAN_POINT('Ctrl Pts',(19.9195088148117,-14.75,-1.75068225711584));
#32798=CARTESIAN_POINT('',(20.5334244370461,-14.75,-1.62380639463663));
#32799=CARTESIAN_POINT('',(20.5334244370461,-15.,-1.62380639463663));
#32800=CARTESIAN_POINT('Ctrl Pts',(20.5334244370461,-14.75,-1.62380639463663));
#32801=CARTESIAN_POINT('Ctrl Pts',(20.2244202494621,-14.75,-1.69747624546289));
#32802=CARTESIAN_POINT('Ctrl Pts',(19.9195088148117,-14.75,-1.75068225711584));
#32803=CARTESIAN_POINT('Origin',(22.5000001192093,-15.,-1.16746257990599));
#32804=CARTESIAN_POINT('',(22.5000001192093,-14.75,-1.16746257990599));
#32805=CARTESIAN_POINT('',(22.5000001192093,-15.,-1.16746257990599));
#32806=CARTESIAN_POINT('',(22.5000001192093,-14.75,-1.16746257990599));
#32807=CARTESIAN_POINT('Origin',(22.5000001192093,-15.,-0.760232009924948));
#32808=CARTESIAN_POINT('',(22.5000001192093,-14.75,-0.760232009924948));
#32809=CARTESIAN_POINT('',(22.5000001192093,-15.,-0.760232009924948));
#32810=CARTESIAN_POINT('',(22.5000001192093,-14.75,-0.760232009924948));
#32811=CARTESIAN_POINT('Origin',(19.5,-15.,-1.55627567321062));
#32812=CARTESIAN_POINT('',(19.5,-14.75,-1.55627567321062));
#32813=CARTESIAN_POINT('',(19.5,-15.,-1.55627567321062));
#32814=CARTESIAN_POINT('',(19.5,-14.75,-1.55627567321062));
#32815=CARTESIAN_POINT('Origin',(19.5,-15.,-1.96145985275507));
#32816=CARTESIAN_POINT('',(19.5,-14.75,-1.96145985275507));
#32817=CARTESIAN_POINT('',(19.5,-15.,-1.96145985275507));
#32818=CARTESIAN_POINT('',(19.5,-14.75,-1.96145985275507));
#32819=CARTESIAN_POINT('Origin',(21.7858117520809,-15.,-2.59788546711206));
#32820=CARTESIAN_POINT('',(21.7858117520809,-14.75,-2.59788546711206));
#32821=CARTESIAN_POINT('Origin',(21.0000000596046,-14.75,-2.6889496226795));
#32822=CARTESIAN_POINT('Origin',(20.4085947275162,-15.,0.0992497429251671));
#32823=CARTESIAN_POINT('',(20.4085947275162,-14.75,0.0992497429251671));
#32824=CARTESIAN_POINT('',(20.4085947275162,-15.,0.0992497429251671));
#32825=CARTESIAN_POINT('',(20.4085947275162,-14.75,1.3536836579442));
#32826=CARTESIAN_POINT('',(20.4085947275162,-14.75,0.0992497429251671));
#32827=CARTESIAN_POINT('',(20.4085947275162,-15.,1.3536836579442));
#32828=CARTESIAN_POINT('Origin',(19.5,-15.,-0.250681973993778));
#32829=CARTESIAN_POINT('',(19.5,-14.75,-0.250681973993778));
#32830=CARTESIAN_POINT('',(19.5,-15.,-0.250681973993778));
#32831=CARTESIAN_POINT('',(19.5,-14.75,-0.250681973993778));
#32832=CARTESIAN_POINT('Origin',(19.5,-15.,-0.702932812273502));
#32833=CARTESIAN_POINT('',(19.5,-14.75,-0.702932812273502));
#32834=CARTESIAN_POINT('',(19.5,-15.,-0.702932812273502));
#32835=CARTESIAN_POINT('',(19.5,-14.75,-0.702932812273502));
#32836=CARTESIAN_POINT('Origin',(22.5000001192093,-15.,0.524897836148739));
#32837=CARTESIAN_POINT('',(22.5000001192093,-14.75,0.524897836148739));
#32838=CARTESIAN_POINT('',(22.5000001192093,-15.,0.524897836148739));
#32839=CARTESIAN_POINT('',(22.5000001192093,-14.75,0.524897836148739));
#32840=CARTESIAN_POINT('Origin',(22.5000001192093,-15.,0.952592231333256));
#32841=CARTESIAN_POINT('',(22.5000001192093,-14.75,0.952592231333256));
#32842=CARTESIAN_POINT('',(22.5000001192093,-15.,0.952592231333256));
#32843=CARTESIAN_POINT('',(22.5000001192093,-14.75,0.952592231333256));
#32844=CARTESIAN_POINT('Origin',(19.5,-15.,2.10470690100919));
#32845=CARTESIAN_POINT('',(19.5,-14.75,2.10470690100919));
#32846=CARTESIAN_POINT('',(19.5,-15.,2.10470690100919));
#32847=CARTESIAN_POINT('',(19.5,-14.75,2.10470690100919));
#32848=CARTESIAN_POINT('Origin',(19.5,-15.,1.68315164744854));
#32849=CARTESIAN_POINT('',(19.5,-14.75,1.68315164744854));
#32850=CARTESIAN_POINT('',(19.5,-15.,1.68315164744854));
#32851=CARTESIAN_POINT('',(19.5,-14.75,1.68315164744854));
#32852=CARTESIAN_POINT('Origin',(20.4085947275162,-15.,1.3536836579442));
#32853=CARTESIAN_POINT('',(20.4085947275162,-14.75,1.3536836579442));
#32854=CARTESIAN_POINT('Origin',(21.0000000596046,-14.75,0.700887044367846));
#32855=CARTESIAN_POINT('Ctrl Pts',(19.6258525252342,-15.,3.89631662517786));
#32856=CARTESIAN_POINT('Ctrl Pts',(19.6258525252342,-14.75,3.89631662517786));
#32857=CARTESIAN_POINT('Ctrl Pts',(19.4488404393196,-15.,4.11221016198397));
#32858=CARTESIAN_POINT('Ctrl Pts',(19.4488404393196,-14.75,4.11221016198397));
#32859=CARTESIAN_POINT('Ctrl Pts',(19.4488404393196,-15.,4.44167826324701));
#32860=CARTESIAN_POINT('Ctrl Pts',(19.4488404393196,-14.75,4.44167826324701));
#32861=CARTESIAN_POINT('',(19.6258525252342,-14.75,3.89631662517786));
#32862=CARTESIAN_POINT('',(19.6258525252342,-15.,3.89631662517786));
#32863=CARTESIAN_POINT('',(19.4488404393196,-14.75,4.44167826324701));
#32864=CARTESIAN_POINT('Ctrl Pts',(19.6258525252342,-14.75,3.89631662517786));
#32865=CARTESIAN_POINT('Ctrl Pts',(19.4488404393196,-14.75,4.11221016198397));
#32866=CARTESIAN_POINT('Ctrl Pts',(19.4488404393196,-14.75,4.44167826324701));
#32867=CARTESIAN_POINT('',(19.4488404393196,-15.,4.44167826324701));
#32868=CARTESIAN_POINT('Ctrl Pts',(20.1272169947624,-15.,3.57196468859911));
#32869=CARTESIAN_POINT('Ctrl Pts',(20.1272169947624,-14.75,3.57196468859911));
#32870=CARTESIAN_POINT('Ctrl Pts',(19.8028649091721,-15.,3.68042308837175));
#32871=CARTESIAN_POINT('Ctrl Pts',(19.8028649091721,-14.75,3.68042308837175));
#32872=CARTESIAN_POINT('Ctrl Pts',(19.6258525252342,-15.,3.89631662517786));
#32873=CARTESIAN_POINT('Ctrl Pts',(19.6258525252342,-14.75,3.89631662517786));
#32874=CARTESIAN_POINT('',(20.1272169947624,-14.75,3.57196468859911));
#32875=CARTESIAN_POINT('',(20.1272169947624,-15.,3.57196468859911));
#32876=CARTESIAN_POINT('Ctrl Pts',(20.1272169947624,-14.75,3.57196468859911));
#32877=CARTESIAN_POINT('Ctrl Pts',(19.8028649091721,-14.75,3.68042308837175));
#32878=CARTESIAN_POINT('Ctrl Pts',(19.6258525252342,-14.75,3.89631662517786));
#32879=CARTESIAN_POINT('Ctrl Pts',(20.9795362949371,-15.,3.46350628882647));
#32880=CARTESIAN_POINT('Ctrl Pts',(20.9795362949371,-14.75,3.46350628882647));
#32881=CARTESIAN_POINT('Ctrl Pts',(20.4515687823296,-15.,3.46350628882647));
#32882=CARTESIAN_POINT('Ctrl Pts',(20.4515687823296,-14.75,3.46350628882647));
#32883=CARTESIAN_POINT('Ctrl Pts',(20.1272169947624,-15.,3.57196468859911));
#32884=CARTESIAN_POINT('Ctrl Pts',(20.1272169947624,-14.75,3.57196468859911));
#32885=CARTESIAN_POINT('',(20.9795362949371,-14.75,3.46350628882647));
#32886=CARTESIAN_POINT('',(20.9795362949371,-15.,3.46350628882647));
#32887=CARTESIAN_POINT('Ctrl Pts',(20.9795362949371,-14.75,3.46350628882647));
#32888=CARTESIAN_POINT('Ctrl Pts',(20.4515687823296,-14.75,3.46350628882647));
#32889=CARTESIAN_POINT('Ctrl Pts',(20.1272169947624,-14.75,3.57196468859911));
#32890=CARTESIAN_POINT('Ctrl Pts',(21.6886084973812,-15.,3.53103701025248));
#32891=CARTESIAN_POINT('Ctrl Pts',(21.6886084973812,-14.75,3.53103701025248));
#32892=CARTESIAN_POINT('Ctrl Pts',(21.4256481528282,-15.,3.46350628882647));
#32893=CARTESIAN_POINT('Ctrl Pts',(21.4256481528282,-14.75,3.46350628882647));
#32894=CARTESIAN_POINT('Ctrl Pts',(20.9795362949371,-15.,3.46350628882647));
#32895=CARTESIAN_POINT('Ctrl Pts',(20.9795362949371,-14.75,3.46350628882647));
#32896=CARTESIAN_POINT('',(21.6886084973812,-14.75,3.53103701025248));
#32897=CARTESIAN_POINT('',(21.6886084973812,-15.,3.53103701025248));
#32898=CARTESIAN_POINT('Ctrl Pts',(21.6886084973812,-14.75,3.53103701025248));
#32899=CARTESIAN_POINT('Ctrl Pts',(21.4256481528282,-14.75,3.46350628882647));
#32900=CARTESIAN_POINT('Ctrl Pts',(20.9795362949371,-14.75,3.46350628882647));
#32901=CARTESIAN_POINT('Ctrl Pts',(22.1347205042839,-15.,3.71725801378489));
#32902=CARTESIAN_POINT('Ctrl Pts',(22.1347205042839,-14.75,3.71725801378489));
#32903=CARTESIAN_POINT('Ctrl Pts',(21.9515691399574,-15.,3.59856758266687));
#32904=CARTESIAN_POINT('Ctrl Pts',(21.9515691399574,-14.75,3.59856758266687));
#32905=CARTESIAN_POINT('Ctrl Pts',(21.6886084973812,-15.,3.53103701025248));
#32906=CARTESIAN_POINT('Ctrl Pts',(21.6886084973812,-14.75,3.53103701025248));
#32907=CARTESIAN_POINT('',(22.1347205042839,-14.75,3.71725801378489));
#32908=CARTESIAN_POINT('',(22.1347205042839,-15.,3.71725801378489));
#32909=CARTESIAN_POINT('Ctrl Pts',(22.1347205042839,-14.75,3.71725801378489));
#32910=CARTESIAN_POINT('Ctrl Pts',(21.9515691399574,-14.75,3.59856758266687));
#32911=CARTESIAN_POINT('Ctrl Pts',(21.6886084973812,-14.75,3.53103701025248));
#32912=CARTESIAN_POINT('Ctrl Pts',(22.4150751233101,-15.,4.01807654649019));
#32913=CARTESIAN_POINT('Ctrl Pts',(22.4150751233101,-14.75,4.01807654649019));
#32914=CARTESIAN_POINT('Ctrl Pts',(22.3178718686104,-15.,3.83594829589128));
#32915=CARTESIAN_POINT('Ctrl Pts',(22.3178718686104,-14.75,3.83594829589128));
#32916=CARTESIAN_POINT('Ctrl Pts',(22.1347205042839,-15.,3.71725801378489));
#32917=CARTESIAN_POINT('Ctrl Pts',(22.1347205042839,-14.75,3.71725801378489));
#32918=CARTESIAN_POINT('',(22.4150751233101,-14.75,4.01807654649019));
#32919=CARTESIAN_POINT('',(22.4150751233101,-15.,4.01807654649019));
#32920=CARTESIAN_POINT('Ctrl Pts',(22.4150751233101,-14.75,4.01807654649019));
#32921=CARTESIAN_POINT('Ctrl Pts',(22.3178718686104,-14.75,3.83594829589128));
#32922=CARTESIAN_POINT('Ctrl Pts',(22.1347205042839,-14.75,3.71725801378489));
#32923=CARTESIAN_POINT('Ctrl Pts',(22.5122783780098,-15.,4.44167826324701));
#32924=CARTESIAN_POINT('Ctrl Pts',(22.5122783780098,-14.75,4.44167826324701));
#32925=CARTESIAN_POINT('Ctrl Pts',(22.5122783780098,-15.,4.2002047970891));
#32926=CARTESIAN_POINT('Ctrl Pts',(22.5122783780098,-14.75,4.2002047970891));
#32927=CARTESIAN_POINT('Ctrl Pts',(22.4150751233101,-15.,4.01807654649019));
#32928=CARTESIAN_POINT('Ctrl Pts',(22.4150751233101,-14.75,4.01807654649019));
#32929=CARTESIAN_POINT('',(22.5122783780098,-14.75,4.44167826324701));
#32930=CARTESIAN_POINT('',(22.5122783780098,-15.,4.44167826324701));
#32931=CARTESIAN_POINT('Ctrl Pts',(22.5122783780098,-14.75,4.44167826324701));
#32932=CARTESIAN_POINT('Ctrl Pts',(22.5122783780098,-14.75,4.2002047970891));
#32933=CARTESIAN_POINT('Ctrl Pts',(22.4150751233101,-14.75,4.01807654649019));
#32934=CARTESIAN_POINT('Ctrl Pts',(22.3362894058228,-15.,4.9849933758378));
#32935=CARTESIAN_POINT('Ctrl Pts',(22.3362894058228,-14.75,4.9849933758378));
#32936=CARTESIAN_POINT('Ctrl Pts',(22.5122783780098,-15.,4.7690998390317));
#32937=CARTESIAN_POINT('Ctrl Pts',(22.5122783780098,-14.75,4.7690998390317));
#32938=CARTESIAN_POINT('Ctrl Pts',(22.5122783780098,-15.,4.44167826324701));
#32939=CARTESIAN_POINT('Ctrl Pts',(22.5122783780098,-14.75,4.44167826324701));
#32940=CARTESIAN_POINT('',(22.3362894058228,-14.75,4.9849933758378));
#32941=CARTESIAN_POINT('',(22.3362894058228,-15.,4.9849933758378));
#32942=CARTESIAN_POINT('Ctrl Pts',(22.3362894058228,-14.75,4.9849933758378));
#32943=CARTESIAN_POINT('Ctrl Pts',(22.5122783780098,-14.75,4.7690998390317));
#32944=CARTESIAN_POINT('Ctrl Pts',(22.5122783780098,-14.75,4.44167826324701));
#32945=CARTESIAN_POINT('Ctrl Pts',(21.8359481990337,-15.,5.31036853790283));
#32946=CARTESIAN_POINT('Ctrl Pts',(21.8359481990337,-14.75,5.31036853790283));
#32947=CARTESIAN_POINT('Ctrl Pts',(22.1603001356125,-15.,5.20088694989681));
#32948=CARTESIAN_POINT('Ctrl Pts',(22.1603001356125,-14.75,5.20088694989681));
#32949=CARTESIAN_POINT('Ctrl Pts',(22.3362894058228,-15.,4.9849933758378));
#32950=CARTESIAN_POINT('Ctrl Pts',(22.3362894058228,-14.75,4.9849933758378));
#32951=CARTESIAN_POINT('',(21.8359481990337,-14.75,5.31036853790283));
#32952=CARTESIAN_POINT('',(21.8359481990337,-15.,5.31036853790283));
#32953=CARTESIAN_POINT('Ctrl Pts',(21.8359481990337,-14.75,5.31036853790283));
#32954=CARTESIAN_POINT('Ctrl Pts',(22.1603001356125,-14.75,5.20088694989681));
#32955=CARTESIAN_POINT('Ctrl Pts',(22.3362894058228,-14.75,4.9849933758378));
#32956=CARTESIAN_POINT('Ctrl Pts',(20.9795362949371,-15.,5.41985012590885));
#32957=CARTESIAN_POINT('Ctrl Pts',(20.9795362949371,-14.75,5.41985012590885));
#32958=CARTESIAN_POINT('Ctrl Pts',(21.511596262455,-15.,5.41985012590885));
#32959=CARTESIAN_POINT('Ctrl Pts',(21.511596262455,-14.75,5.41985012590885));
#32960=CARTESIAN_POINT('Ctrl Pts',(21.8359481990337,-15.,5.31036853790283));
#32961=CARTESIAN_POINT('Ctrl Pts',(21.8359481990337,-14.75,5.31036853790283));
#32962=CARTESIAN_POINT('',(20.9795362949371,-14.75,5.41985012590885));
#32963=CARTESIAN_POINT('',(20.9795362949371,-15.,5.41985012590885));
#32964=CARTESIAN_POINT('Ctrl Pts',(20.9795362949371,-14.75,5.41985012590885));
#32965=CARTESIAN_POINT('Ctrl Pts',(21.511596262455,-14.75,5.41985012590885));
#32966=CARTESIAN_POINT('Ctrl Pts',(21.8359481990337,-14.75,5.31036853790283));
#32967=CARTESIAN_POINT('Ctrl Pts',(19.7598908543587,-15.,5.12312430888414));
#32968=CARTESIAN_POINT('Ctrl Pts',(19.7598908543587,-14.75,5.12312430888414));
#32969=CARTESIAN_POINT('Ctrl Pts',(20.1343790888786,-15.,5.41985012590885));
#32970=CARTESIAN_POINT('Ctrl Pts',(20.1343790888786,-14.75,5.41985012590885));
#32971=CARTESIAN_POINT('Ctrl Pts',(20.9795362949371,-15.,5.41985012590885));
#32972=CARTESIAN_POINT('Ctrl Pts',(20.9795362949371,-14.75,5.41985012590885));
#32973=CARTESIAN_POINT('',(19.7598908543587,-14.75,5.12312430888414));
#32974=CARTESIAN_POINT('',(19.7598908543587,-15.,5.12312430888414));
#32975=CARTESIAN_POINT('Ctrl Pts',(19.7598908543587,-14.75,5.12312430888414));
#32976=CARTESIAN_POINT('Ctrl Pts',(20.1343790888786,-14.75,5.41985012590885));
#32977=CARTESIAN_POINT('Ctrl Pts',(20.9795362949371,-14.75,5.41985012590885));
#32978=CARTESIAN_POINT('Ctrl Pts',(19.4488404393196,-15.,4.44167826324701));
#32979=CARTESIAN_POINT('Ctrl Pts',(19.4488404393196,-14.75,4.44167826324701));
#32980=CARTESIAN_POINT('Ctrl Pts',(19.4488404393196,-15.,4.87551178783178));
#32981=CARTESIAN_POINT('Ctrl Pts',(19.4488404393196,-14.75,4.87551178783178));
#32982=CARTESIAN_POINT('Ctrl Pts',(19.7598908543587,-15.,5.12312430888414));
#32983=CARTESIAN_POINT('Ctrl Pts',(19.7598908543587,-14.75,5.12312430888414));
#32984=CARTESIAN_POINT('Ctrl Pts',(19.4488404393196,-14.75,4.44167826324701));
#32985=CARTESIAN_POINT('Ctrl Pts',(19.4488404393196,-14.75,4.87551178783178));
#32986=CARTESIAN_POINT('Ctrl Pts',(19.7598908543587,-14.75,5.12312430888414));
#32987=CARTESIAN_POINT('Origin',(20.9805594086647,-14.75,4.44167820736766));
#32988=CARTESIAN_POINT('Ctrl Pts',(22.1111871004105,-15.,6.9280356541276));
#32989=CARTESIAN_POINT('Ctrl Pts',(22.1111871004105,-14.75,6.9280356541276));
#32990=CARTESIAN_POINT('Ctrl Pts',(22.3178718686104,-15.,6.69679414480925));
#32991=CARTESIAN_POINT('Ctrl Pts',(22.3178718686104,-14.75,6.69679414480925));
#32992=CARTESIAN_POINT('Ctrl Pts',(22.5122783780098,-15.,6.60061407834291));
#32993=CARTESIAN_POINT('Ctrl Pts',(22.5122783780098,-14.75,6.60061407834291));
#32994=CARTESIAN_POINT('',(22.1111871004105,-14.75,6.9280356541276));
#32995=CARTESIAN_POINT('',(22.1111871004105,-15.,6.9280356541276));
#32996=CARTESIAN_POINT('',(22.5122783780098,-14.75,6.60061407834291));
#32997=CARTESIAN_POINT('Ctrl Pts',(22.1111871004105,-14.75,6.9280356541276));
#32998=CARTESIAN_POINT('Ctrl Pts',(22.3178718686104,-14.75,6.69679414480925));
#32999=CARTESIAN_POINT('Ctrl Pts',(22.5122783780098,-14.75,6.60061407834291));
#33000=CARTESIAN_POINT('',(22.5122783780098,-15.,6.60061407834291));
#33001=CARTESIAN_POINT('Ctrl Pts',(21.7592087090015,-15.,7.46828120201826));
#33002=CARTESIAN_POINT('Ctrl Pts',(21.7592087090015,-14.75,7.46828120201826));
#33003=CARTESIAN_POINT('Ctrl Pts',(21.9045020341873,-15.,7.15927708894014));
#33004=CARTESIAN_POINT('Ctrl Pts',(21.9045020341873,-14.75,7.15927708894014));
#33005=CARTESIAN_POINT('Ctrl Pts',(22.1111871004105,-15.,6.9280356541276));
#33006=CARTESIAN_POINT('Ctrl Pts',(22.1111871004105,-14.75,6.9280356541276));
#33007=CARTESIAN_POINT('',(21.7592087090015,-14.75,7.46828120201826));
#33008=CARTESIAN_POINT('',(21.7592087090015,-15.,7.46828120201826));
#33009=CARTESIAN_POINT('Ctrl Pts',(21.7592087090015,-14.75,7.46828120201826));
#33010=CARTESIAN_POINT('Ctrl Pts',(21.9045020341873,-14.75,7.15927708894014));
#33011=CARTESIAN_POINT('Ctrl Pts',(22.1111871004105,-14.75,6.9280356541276));
#33012=CARTESIAN_POINT('Origin',(21.4031378626823,-15.,7.46828120201826));
#33013=CARTESIAN_POINT('',(21.4031378626823,-14.75,7.46828120201826));
#33014=CARTESIAN_POINT('',(21.4031378626823,-15.,7.46828120201826));
#33015=CARTESIAN_POINT('',(21.4031378626823,-14.75,7.46828120201826));
#33016=CARTESIAN_POINT('Ctrl Pts',(21.5934516191483,-15.,7.080491296947));
#33017=CARTESIAN_POINT('Ctrl Pts',(21.5934516191483,-14.75,7.080491296947));
#33018=CARTESIAN_POINT('Ctrl Pts',(21.4665756821632,-15.,7.29638490825891));
#33019=CARTESIAN_POINT('Ctrl Pts',(21.4665756821632,-14.75,7.29638490825891));
#33020=CARTESIAN_POINT('Ctrl Pts',(21.4031378626823,-15.,7.46828120201826));
#33021=CARTESIAN_POINT('Ctrl Pts',(21.4031378626823,-14.75,7.46828120201826));
#33022=CARTESIAN_POINT('',(21.5934516191483,-14.75,7.080491296947));
#33023=CARTESIAN_POINT('',(21.5934516191483,-15.,7.080491296947));
#33024=CARTESIAN_POINT('Ctrl Pts',(21.5934516191483,-14.75,7.080491296947));
#33025=CARTESIAN_POINT('Ctrl Pts',(21.4665756821632,-14.75,7.29638490825891));
#33026=CARTESIAN_POINT('Ctrl Pts',(21.4031378626823,-14.75,7.46828120201826));
#33027=CARTESIAN_POINT('Ctrl Pts',(21.8472033441067,-15.,6.73158269375563));
#33028=CARTESIAN_POINT('Ctrl Pts',(21.8472033441067,-14.75,6.73158269375563));
#33029=CARTESIAN_POINT('Ctrl Pts',(21.7203274071217,-15.,6.86459768563509));
#33030=CARTESIAN_POINT('Ctrl Pts',(21.7203274071217,-14.75,6.86459768563509));
#33031=CARTESIAN_POINT('Ctrl Pts',(21.5934516191483,-15.,7.080491296947));
#33032=CARTESIAN_POINT('Ctrl Pts',(21.5934516191483,-14.75,7.080491296947));
#33033=CARTESIAN_POINT('',(21.8472033441067,-14.75,6.73158269375563));
#33034=CARTESIAN_POINT('',(21.8472033441067,-15.,6.73158269375563));
#33035=CARTESIAN_POINT('Ctrl Pts',(21.8472033441067,-14.75,6.73158269375563));
#33036=CARTESIAN_POINT('Ctrl Pts',(21.7203274071217,-14.75,6.86459768563509));
#33037=CARTESIAN_POINT('Ctrl Pts',(21.5934516191483,-14.75,7.080491296947));
#33038=CARTESIAN_POINT('Origin',(19.5,-15.,6.73158269375563));
#33039=CARTESIAN_POINT('',(19.5,-14.75,6.73158269375563));
#33040=CARTESIAN_POINT('',(19.5,-15.,6.73158269375563));
#33041=CARTESIAN_POINT('',(19.5,-14.75,6.73158269375563));
#33042=CARTESIAN_POINT('Origin',(19.5,-15.,6.3632333651185));
#33043=CARTESIAN_POINT('',(19.5,-14.75,6.3632333651185));
#33044=CARTESIAN_POINT('',(19.5,-15.,6.3632333651185));
#33045=CARTESIAN_POINT('',(19.5,-14.75,6.3632333651185));
#33046=CARTESIAN_POINT('Origin',(22.5122783780098,-15.,6.3632333651185));
#33047=CARTESIAN_POINT('',(22.5122783780098,-14.75,6.3632333651185));
#33048=CARTESIAN_POINT('',(22.5122783780098,-15.,6.3632333651185));
#33049=CARTESIAN_POINT('',(22.5122783780098,-14.75,6.3632333651185));
#33050=CARTESIAN_POINT('Origin',(22.5122783780098,-15.,6.60061407834291));
#33051=CARTESIAN_POINT('',(22.5122783780098,-14.75,6.60061407834291));
#33052=CARTESIAN_POINT('Origin',(21.0061391890049,-14.75,6.91575728356838));
#33053=CARTESIAN_POINT('Ctrl Pts',(19.9062074422836,-15.,-6.90143261104822));
#33054=CARTESIAN_POINT('Ctrl Pts',(19.9062074422836,-14.75,-6.90143261104822));
#33055=CARTESIAN_POINT('Ctrl Pts',(20.0054569244385,-15.,-7.14699868112802));
#33056=CARTESIAN_POINT('Ctrl Pts',(20.0054569244385,-14.75,-7.14699868112802));
#33057=CARTESIAN_POINT('Ctrl Pts',(20.1180080771446,-15.,-7.27387461811304));
#33058=CARTESIAN_POINT('Ctrl Pts',(20.1180080771446,-14.75,-7.27387461811304));
#33059=CARTESIAN_POINT('',(19.9062074422836,-14.75,-6.90143261104822));
#33060=CARTESIAN_POINT('',(19.9062074422836,-15.,-6.90143261104822));
#33061=CARTESIAN_POINT('',(20.1180080771446,-14.75,-7.27387461811304));
#33062=CARTESIAN_POINT('Ctrl Pts',(19.9062074422836,-14.75,-6.90143261104822));
#33063=CARTESIAN_POINT('Ctrl Pts',(20.0054569244385,-14.75,-7.14699868112802));
#33064=CARTESIAN_POINT('Ctrl Pts',(20.1180080771446,-14.75,-7.27387461811304));
#33065=CARTESIAN_POINT('',(20.1180080771446,-15.,-7.27387461811304));
#33066=CARTESIAN_POINT('Ctrl Pts',(19.8069576621056,-15.,-6.39802191406488));
#33067=CARTESIAN_POINT('Ctrl Pts',(19.8069576621056,-14.75,-6.39802191406488));
#33068=CARTESIAN_POINT('Ctrl Pts',(19.8069576621056,-15.,-6.6558663919568));
#33069=CARTESIAN_POINT('Ctrl Pts',(19.8069576621056,-14.75,-6.6558663919568));
#33070=CARTESIAN_POINT('Ctrl Pts',(19.9062074422836,-15.,-6.90143261104822));
#33071=CARTESIAN_POINT('Ctrl Pts',(19.9062074422836,-14.75,-6.90143261104822));
#33072=CARTESIAN_POINT('',(19.8069576621056,-14.75,-6.39802191406488));
#33073=CARTESIAN_POINT('',(19.8069576621056,-15.,-6.39802191406488));
#33074=CARTESIAN_POINT('Ctrl Pts',(19.8069576621056,-14.75,-6.39802191406488));
#33075=CARTESIAN_POINT('Ctrl Pts',(19.8069576621056,-14.75,-6.6558663919568));
#33076=CARTESIAN_POINT('Ctrl Pts',(19.9062074422836,-14.75,-6.90143261104822));
#33077=CARTESIAN_POINT('Ctrl Pts',(19.9379263520241,-15.,-5.8373125270009));
#33078=CARTESIAN_POINT('Ctrl Pts',(19.9379263520241,-14.75,-5.8373125270009));
#33079=CARTESIAN_POINT('Ctrl Pts',(19.8069576621056,-15.,-6.10129613429308));
#33080=CARTESIAN_POINT('Ctrl Pts',(19.8069576621056,-14.75,-6.10129613429308));
#33081=CARTESIAN_POINT('Ctrl Pts',(19.8069576621056,-15.,-6.39802191406488));
#33082=CARTESIAN_POINT('Ctrl Pts',(19.8069576621056,-14.75,-6.39802191406488));
#33083=CARTESIAN_POINT('',(19.9379263520241,-14.75,-5.8373125270009));
#33084=CARTESIAN_POINT('',(19.9379263520241,-15.,-5.8373125270009));
#33085=CARTESIAN_POINT('Ctrl Pts',(19.9379263520241,-14.75,-5.8373125270009));
#33086=CARTESIAN_POINT('Ctrl Pts',(19.8069576621056,-14.75,-6.10129613429308));
#33087=CARTESIAN_POINT('Ctrl Pts',(19.8069576621056,-14.75,-6.39802191406488));
#33088=CARTESIAN_POINT('Ctrl Pts',(20.3390176296234,-15.,-5.43519791215658));
#33089=CARTESIAN_POINT('Ctrl Pts',(20.3390176296234,-14.75,-5.43519791215658));
#33090=CARTESIAN_POINT('Ctrl Pts',(20.0688950419426,-15.,-5.57332884520292));
#33091=CARTESIAN_POINT('Ctrl Pts',(20.0688950419426,-14.75,-5.57332884520292));
#33092=CARTESIAN_POINT('Ctrl Pts',(19.9379263520241,-15.,-5.8373125270009));
#33093=CARTESIAN_POINT('Ctrl Pts',(19.9379263520241,-14.75,-5.8373125270009));
#33094=CARTESIAN_POINT('',(20.3390176296234,-14.75,-5.43519791215658));
#33095=CARTESIAN_POINT('',(20.3390176296234,-15.,-5.43519791215658));
#33096=CARTESIAN_POINT('Ctrl Pts',(20.3390176296234,-14.75,-5.43519791215658));
#33097=CARTESIAN_POINT('Ctrl Pts',(20.0688950419426,-14.75,-5.57332884520292));
#33098=CARTESIAN_POINT('Ctrl Pts',(19.9379263520241,-14.75,-5.8373125270009));
#33099=CARTESIAN_POINT('Ctrl Pts',(21.0102319419384,-15.,-5.29706697911024));
#33100=CARTESIAN_POINT('Ctrl Pts',(21.0102319419384,-14.75,-5.29706697911024));
#33101=CARTESIAN_POINT('Ctrl Pts',(20.6091405153275,-15.,-5.29706697911024));
#33102=CARTESIAN_POINT('Ctrl Pts',(20.6091405153275,-14.75,-5.29706697911024));
#33103=CARTESIAN_POINT('Ctrl Pts',(20.3390176296234,-15.,-5.43519791215658));
#33104=CARTESIAN_POINT('Ctrl Pts',(20.3390176296234,-14.75,-5.43519791215658));
#33105=CARTESIAN_POINT('',(21.0102319419384,-14.75,-5.29706697911024));
#33106=CARTESIAN_POINT('',(21.0102319419384,-15.,-5.29706697911024));
#33107=CARTESIAN_POINT('Ctrl Pts',(21.0102319419384,-14.75,-5.29706697911024));
#33108=CARTESIAN_POINT('Ctrl Pts',(20.6091405153275,-14.75,-5.29706697911024));
#33109=CARTESIAN_POINT('Ctrl Pts',(20.3390176296234,-14.75,-5.43519791215658));
#33110=CARTESIAN_POINT('Ctrl Pts',(21.6139155328274,-15.,-5.41166450828314));
#33111=CARTESIAN_POINT('Ctrl Pts',(21.6139155328274,-14.75,-5.41166450828314));
#33112=CARTESIAN_POINT('Ctrl Pts',(21.3356071412563,-15.,-5.29706697911024));
#33113=CARTESIAN_POINT('Ctrl Pts',(21.3356071412563,-14.75,-5.29706697911024));
#33114=CARTESIAN_POINT('Ctrl Pts',(21.0102319419384,-15.,-5.29706697911024));
#33115=CARTESIAN_POINT('Ctrl Pts',(21.0102319419384,-14.75,-5.29706697911024));
#33116=CARTESIAN_POINT('',(21.6139155328274,-14.75,-5.41166450828314));
#33117=CARTESIAN_POINT('',(21.6139155328274,-15.,-5.41166450828314));
#33118=CARTESIAN_POINT('Ctrl Pts',(21.6139155328274,-14.75,-5.41166450828314));
#33119=CARTESIAN_POINT('Ctrl Pts',(21.3356071412563,-14.75,-5.29706697911024));
#33120=CARTESIAN_POINT('Ctrl Pts',(21.0102319419384,-14.75,-5.29706697911024));
#33121=CARTESIAN_POINT('Ctrl Pts',(21.9106413125992,-15.,-5.60095507651567));
#33122=CARTESIAN_POINT('Ctrl Pts',(21.9106413125992,-14.75,-5.60095507651567));
#33123=CARTESIAN_POINT('Ctrl Pts',(21.7755798697472,-15.,-5.47919515520334));
#33124=CARTESIAN_POINT('Ctrl Pts',(21.7755798697472,-14.75,-5.47919515520334));
#33125=CARTESIAN_POINT('Ctrl Pts',(21.6139155328274,-15.,-5.41166450828314));
#33126=CARTESIAN_POINT('Ctrl Pts',(21.6139155328274,-14.75,-5.41166450828314));
#33127=CARTESIAN_POINT('',(21.9106413125992,-14.75,-5.60095507651567));
#33128=CARTESIAN_POINT('',(21.9106413125992,-15.,-5.60095507651567));
#33129=CARTESIAN_POINT('Ctrl Pts',(21.9106413125992,-14.75,-5.60095507651567));
#33130=CARTESIAN_POINT('Ctrl Pts',(21.7755798697472,-14.75,-5.47919515520334));
#33131=CARTESIAN_POINT('Ctrl Pts',(21.6139155328274,-14.75,-5.41166450828314));
#33132=CARTESIAN_POINT('Ctrl Pts',(22.128581225872,-15.,-5.92121426016092));
#33133=CARTESIAN_POINT('Ctrl Pts',(22.128581225872,-14.75,-5.92121426016092));
#33134=CARTESIAN_POINT('Ctrl Pts',(22.0457027554512,-15.,-5.7227149233222));
#33135=CARTESIAN_POINT('Ctrl Pts',(22.0457027554512,-14.75,-5.7227149233222));
#33136=CARTESIAN_POINT('Ctrl Pts',(21.9106413125992,-15.,-5.60095507651567));
#33137=CARTESIAN_POINT('Ctrl Pts',(21.9106413125992,-14.75,-5.60095507651567));
#33138=CARTESIAN_POINT('',(22.128581225872,-14.75,-5.92121426016092));
#33139=CARTESIAN_POINT('',(22.128581225872,-15.,-5.92121426016092));
#33140=CARTESIAN_POINT('Ctrl Pts',(22.128581225872,-14.75,-5.92121426016092));
#33141=CARTESIAN_POINT('Ctrl Pts',(22.0457027554512,-14.75,-5.7227149233222));
#33142=CARTESIAN_POINT('Ctrl Pts',(21.9106413125992,-14.75,-5.60095507651567));
#33143=CARTESIAN_POINT('Ctrl Pts',(22.2114599943161,-15.,-6.39188278466463));
#33144=CARTESIAN_POINT('Ctrl Pts',(22.2114599943161,-14.75,-6.39188278466463));
#33145=CARTESIAN_POINT('Ctrl Pts',(22.2114599943161,-15.,-6.11971367150545));
#33146=CARTESIAN_POINT('Ctrl Pts',(22.2114599943161,-14.75,-6.11971367150545));
#33147=CARTESIAN_POINT('Ctrl Pts',(22.128581225872,-15.,-5.92121426016092));
#33148=CARTESIAN_POINT('Ctrl Pts',(22.128581225872,-14.75,-5.92121426016092));
#33149=CARTESIAN_POINT('',(22.2114599943161,-14.75,-6.39188278466463));
#33150=CARTESIAN_POINT('',(22.2114599943161,-15.,-6.39188278466463));
#33151=CARTESIAN_POINT('Ctrl Pts',(22.2114599943161,-14.75,-6.39188278466463));
#33152=CARTESIAN_POINT('Ctrl Pts',(22.2114599943161,-14.75,-6.11971367150545));
#33153=CARTESIAN_POINT('Ctrl Pts',(22.128581225872,-14.75,-5.92121426016092));
#33154=CARTESIAN_POINT('Ctrl Pts',(22.1326739788055,-15.,-6.80525247007608));
#33155=CARTESIAN_POINT('Ctrl Pts',(22.1326739788055,-14.75,-6.80525247007608));
#33156=CARTESIAN_POINT('Ctrl Pts',(22.2114599943161,-15.,-6.61903146654367));
#33157=CARTESIAN_POINT('Ctrl Pts',(22.2114599943161,-14.75,-6.61903146654367));
#33158=CARTESIAN_POINT('Ctrl Pts',(22.2114599943161,-15.,-6.39188278466463));
#33159=CARTESIAN_POINT('Ctrl Pts',(22.2114599943161,-14.75,-6.39188278466463));
#33160=CARTESIAN_POINT('',(22.1326739788055,-14.75,-6.80525247007608));
#33161=CARTESIAN_POINT('',(22.1326739788055,-15.,-6.80525247007608));
#33162=CARTESIAN_POINT('Ctrl Pts',(22.1326739788055,-14.75,-6.80525247007608));
#33163=CARTESIAN_POINT('Ctrl Pts',(22.2114599943161,-14.75,-6.61903146654367));
#33164=CARTESIAN_POINT('Ctrl Pts',(22.2114599943161,-14.75,-6.39188278466463));
#33165=CARTESIAN_POINT('Ctrl Pts',(21.9229195713997,-15.,-7.09174636751413));
#33166=CARTESIAN_POINT('Ctrl Pts',(21.9229195713997,-14.75,-7.09174636751413));
#33167=CARTESIAN_POINT('Ctrl Pts',(22.0538882613182,-15.,-6.99147347360849));
#33168=CARTESIAN_POINT('Ctrl Pts',(22.0538882613182,-14.75,-6.99147347360849));
#33169=CARTESIAN_POINT('Ctrl Pts',(22.1326739788055,-15.,-6.80525247007608));
#33170=CARTESIAN_POINT('Ctrl Pts',(22.1326739788055,-14.75,-6.80525247007608));
#33171=CARTESIAN_POINT('',(21.9229195713997,-14.75,-7.09174636751413));
#33172=CARTESIAN_POINT('',(21.9229195713997,-15.,-7.09174636751413));
#33173=CARTESIAN_POINT('Ctrl Pts',(21.9229195713997,-14.75,-7.09174636751413));
#33174=CARTESIAN_POINT('Ctrl Pts',(22.0538882613182,-14.75,-6.99147347360849));
#33175=CARTESIAN_POINT('Ctrl Pts',(22.1326739788055,-14.75,-6.80525247007608));
#33176=CARTESIAN_POINT('Ctrl Pts',(21.562755972147,-15.,-7.25955013185739));
#33177=CARTESIAN_POINT('Ctrl Pts',(21.562755972147,-14.75,-7.25955013185739));
#33178=CARTESIAN_POINT('Ctrl Pts',(21.7919510304928,-15.,-7.19201926141977));
#33179=CARTESIAN_POINT('Ctrl Pts',(21.7919510304928,-14.75,-7.19201926141977));
#33180=CARTESIAN_POINT('Ctrl Pts',(21.9229195713997,-15.,-7.09174636751413));
#33181=CARTESIAN_POINT('Ctrl Pts',(21.9229195713997,-14.75,-7.09174636751413));
#33182=CARTESIAN_POINT('',(21.562755972147,-14.75,-7.25955013185739));
#33183=CARTESIAN_POINT('',(21.562755972147,-15.,-7.25955013185739));
#33184=CARTESIAN_POINT('Ctrl Pts',(21.562755972147,-14.75,-7.25955013185739));
#33185=CARTESIAN_POINT('Ctrl Pts',(21.7919510304928,-14.75,-7.19201926141977));
#33186=CARTESIAN_POINT('Ctrl Pts',(21.9229195713997,-14.75,-7.09174636751413));
#33187=CARTESIAN_POINT('Origin',(21.6609823405743,-15.,-7.61766735464334));
#33188=CARTESIAN_POINT('',(21.6609823405743,-14.75,-7.61766735464334));
#33189=CARTESIAN_POINT('',(21.6609823405743,-15.,-7.61766735464334));
#33190=CARTESIAN_POINT('',(21.6609823405743,-14.75,-7.61766735464334));
#33191=CARTESIAN_POINT('Ctrl Pts',(22.1521146297455,-15.,-7.39051882177591));
#33192=CARTESIAN_POINT('Ctrl Pts',(22.1521146297455,-14.75,-7.39051882177591));
#33193=CARTESIAN_POINT('Ctrl Pts',(21.9638473987579,-15.,-7.53990475088358));
#33194=CARTESIAN_POINT('Ctrl Pts',(21.9638473987579,-14.75,-7.53990475088358));
#33195=CARTESIAN_POINT('Ctrl Pts',(21.6609823405743,-15.,-7.61766735464334));
#33196=CARTESIAN_POINT('Ctrl Pts',(21.6609823405743,-14.75,-7.61766735464334));
#33197=CARTESIAN_POINT('',(22.1521146297455,-14.75,-7.39051882177591));
#33198=CARTESIAN_POINT('',(22.1521146297455,-15.,-7.39051882177591));
#33199=CARTESIAN_POINT('Ctrl Pts',(22.1521146297455,-14.75,-7.39051882177591));
#33200=CARTESIAN_POINT('Ctrl Pts',(21.9638473987579,-14.75,-7.53990475088358));
#33201=CARTESIAN_POINT('Ctrl Pts',(21.6609823405743,-14.75,-7.61766735464334));
#33202=CARTESIAN_POINT('Ctrl Pts',(22.445770919323,-15.,-6.9781719520688));
#33203=CARTESIAN_POINT('Ctrl Pts',(22.445770919323,-14.75,-6.9781719520688));
#33204=CARTESIAN_POINT('Ctrl Pts',(22.3403821587563,-15.,-7.24113259464502));
#33205=CARTESIAN_POINT('Ctrl Pts',(22.3403821587563,-14.75,-7.24113259464502));
#33206=CARTESIAN_POINT('Ctrl Pts',(22.1521146297455,-15.,-7.39051882177591));
#33207=CARTESIAN_POINT('Ctrl Pts',(22.1521146297455,-14.75,-7.39051882177591));
#33208=CARTESIAN_POINT('',(22.445770919323,-14.75,-6.9781719520688));
#33209=CARTESIAN_POINT('',(22.445770919323,-15.,-6.9781719520688));
#33210=CARTESIAN_POINT('Ctrl Pts',(22.445770919323,-14.75,-6.9781719520688));
#33211=CARTESIAN_POINT('Ctrl Pts',(22.3403821587563,-14.75,-7.24113259464502));
#33212=CARTESIAN_POINT('Ctrl Pts',(22.1521146297455,-14.75,-7.39051882177591));
#33213=CARTESIAN_POINT('Ctrl Pts',(22.5511596798897,-15.,-6.38983640819788));
#33214=CARTESIAN_POINT('Ctrl Pts',(22.5511596798897,-14.75,-6.38983640819788));
#33215=CARTESIAN_POINT('Ctrl Pts',(22.5511596798897,-15.,-6.71521160751581));
#33216=CARTESIAN_POINT('Ctrl Pts',(22.5511596798897,-14.75,-6.71521160751581));
#33217=CARTESIAN_POINT('Ctrl Pts',(22.445770919323,-15.,-6.9781719520688));
#33218=CARTESIAN_POINT('Ctrl Pts',(22.445770919323,-14.75,-6.9781719520688));
#33219=CARTESIAN_POINT('',(22.5511596798897,-14.75,-6.38983640819788));
#33220=CARTESIAN_POINT('',(22.5511596798897,-15.,-6.38983640819788));
#33221=CARTESIAN_POINT('Ctrl Pts',(22.5511596798897,-14.75,-6.38983640819788));
#33222=CARTESIAN_POINT('Ctrl Pts',(22.5511596798897,-14.75,-6.71521160751581));
#33223=CARTESIAN_POINT('Ctrl Pts',(22.445770919323,-14.75,-6.9781719520688));
#33224=CARTESIAN_POINT('Ctrl Pts',(22.3669852018356,-15.,-5.59788551181555));
#33225=CARTESIAN_POINT('Ctrl Pts',(22.3669852018356,-14.75,-5.59788551181555));
#33226=CARTESIAN_POINT('Ctrl Pts',(22.5511596798897,-15.,-5.94167817384004));
#33227=CARTESIAN_POINT('Ctrl Pts',(22.5511596798897,-14.75,-5.94167817384004));
#33228=CARTESIAN_POINT('Ctrl Pts',(22.5511596798897,-15.,-6.38983640819788));
#33229=CARTESIAN_POINT('Ctrl Pts',(22.5511596798897,-14.75,-6.38983640819788));
#33230=CARTESIAN_POINT('',(22.3669852018356,-14.75,-5.59788551181555));
#33231=CARTESIAN_POINT('',(22.3669852018356,-15.,-5.59788551181555));
#33232=CARTESIAN_POINT('Ctrl Pts',(22.3669852018356,-14.75,-5.59788551181555));
#33233=CARTESIAN_POINT('Ctrl Pts',(22.5511596798897,-14.75,-5.94167817384004));
#33234=CARTESIAN_POINT('Ctrl Pts',(22.5511596798897,-14.75,-6.38983640819788));
#33235=CARTESIAN_POINT('Ctrl Pts',(21.8032061755657,-15.,-5.07094141095877));
#33236=CARTESIAN_POINT('Ctrl Pts',(21.8032061755657,-14.75,-5.07094141095877));
#33237=CARTESIAN_POINT('Ctrl Pts',(22.1828104257584,-15.,-5.25409284979105));
#33238=CARTESIAN_POINT('Ctrl Pts',(22.1828104257584,-14.75,-5.25409284979105));
#33239=CARTESIAN_POINT('Ctrl Pts',(22.3669852018356,-15.,-5.59788551181555));
#33240=CARTESIAN_POINT('Ctrl Pts',(22.3669852018356,-14.75,-5.59788551181555));
#33241=CARTESIAN_POINT('',(21.8032061755657,-14.75,-5.07094141095877));
#33242=CARTESIAN_POINT('',(21.8032061755657,-15.,-5.07094141095877));
#33243=CARTESIAN_POINT('Ctrl Pts',(21.8032061755657,-14.75,-5.07094141095877));
#33244=CARTESIAN_POINT('Ctrl Pts',(22.1828104257584,-14.75,-5.25409284979105));
#33245=CARTESIAN_POINT('Ctrl Pts',(22.3669852018356,-14.75,-5.59788551181555));
#33246=CARTESIAN_POINT('Ctrl Pts',(20.9856754243374,-15.,-4.88778999075293));
#33247=CARTESIAN_POINT('Ctrl Pts',(20.9856754243374,-14.75,-4.88778999075293));
#33248=CARTESIAN_POINT('Ctrl Pts',(21.4236017763615,-15.,-4.88778999075293));
#33249=CARTESIAN_POINT('Ctrl Pts',(21.4236017763615,-14.75,-4.88778999075293));
#33250=CARTESIAN_POINT('Ctrl Pts',(21.8032061755657,-15.,-5.07094141095877));
#33251=CARTESIAN_POINT('Ctrl Pts',(21.8032061755657,-14.75,-5.07094141095877));
#33252=CARTESIAN_POINT('',(20.9856754243374,-14.75,-4.88778999075293));
#33253=CARTESIAN_POINT('',(20.9856754243374,-15.,-4.88778999075293));
#33254=CARTESIAN_POINT('Ctrl Pts',(20.9856754243374,-14.75,-4.88778999075293));
#33255=CARTESIAN_POINT('Ctrl Pts',(21.4236017763615,-14.75,-4.88778999075293));
#33256=CARTESIAN_POINT('Ctrl Pts',(21.8032061755657,-14.75,-5.07094141095877));
#33257=CARTESIAN_POINT('Ctrl Pts',(20.1855389475822,-15.,-5.07196459919214));
#33258=CARTESIAN_POINT('Ctrl Pts',(20.1855389475822,-14.75,-5.07196459919214));
#33259=CARTESIAN_POINT('Ctrl Pts',(20.5436561703682,-15.,-4.88778999075293));
#33260=CARTESIAN_POINT('Ctrl Pts',(20.5436561703682,-14.75,-4.88778999075293));
#33261=CARTESIAN_POINT('Ctrl Pts',(20.9856754243374,-15.,-4.88778999075293));
#33262=CARTESIAN_POINT('Ctrl Pts',(20.9856754243374,-14.75,-4.88778999075293));
#33263=CARTESIAN_POINT('',(20.1855389475822,-14.75,-5.07196459919214));
#33264=CARTESIAN_POINT('',(20.1855389475822,-15.,-5.07196459919214));
#33265=CARTESIAN_POINT('Ctrl Pts',(20.1855389475822,-14.75,-5.07196459919214));
#33266=CARTESIAN_POINT('Ctrl Pts',(20.5436561703682,-14.75,-4.88778999075293));
#33267=CARTESIAN_POINT('Ctrl Pts',(20.9856754243374,-14.75,-4.88778999075293));
#33268=CARTESIAN_POINT('Ctrl Pts',(19.638131082058,-15.,-5.61732616275549));
#33269=CARTESIAN_POINT('Ctrl Pts',(19.638131082058,-14.75,-5.61732616275549));
#33270=CARTESIAN_POINT('Ctrl Pts',(19.8274214267731,-15.,-5.2561392262578));
#33271=CARTESIAN_POINT('Ctrl Pts',(19.8274214267731,-14.75,-5.2561392262578));
#33272=CARTESIAN_POINT('Ctrl Pts',(20.1855389475822,-15.,-5.07196459919214));
#33273=CARTESIAN_POINT('Ctrl Pts',(20.1855389475822,-14.75,-5.07196459919214));
#33274=CARTESIAN_POINT('',(19.638131082058,-14.75,-5.61732616275549));
#33275=CARTESIAN_POINT('',(19.638131082058,-15.,-5.61732616275549));
#33276=CARTESIAN_POINT('Ctrl Pts',(19.638131082058,-14.75,-5.61732616275549));
#33277=CARTESIAN_POINT('Ctrl Pts',(19.8274214267731,-14.75,-5.2561392262578));
#33278=CARTESIAN_POINT('Ctrl Pts',(20.1855389475822,-14.75,-5.07196459919214));
#33279=CARTESIAN_POINT('Ctrl Pts',(19.4488404393196,-15.,-6.42053220421076));
#33280=CARTESIAN_POINT('Ctrl Pts',(19.4488404393196,-14.75,-6.42053220421076));
#33281=CARTESIAN_POINT('Ctrl Pts',(19.4488404393196,-15.,-5.97851309925318));
#33282=CARTESIAN_POINT('Ctrl Pts',(19.4488404393196,-14.75,-5.97851309925318));
#33283=CARTESIAN_POINT('Ctrl Pts',(19.638131082058,-15.,-5.61732616275549));
#33284=CARTESIAN_POINT('Ctrl Pts',(19.638131082058,-14.75,-5.61732616275549));
#33285=CARTESIAN_POINT('',(19.4488404393196,-14.75,-6.42053220421076));
#33286=CARTESIAN_POINT('',(19.4488404393196,-15.,-6.42053220421076));
#33287=CARTESIAN_POINT('Ctrl Pts',(19.4488404393196,-14.75,-6.42053220421076));
#33288=CARTESIAN_POINT('Ctrl Pts',(19.4488404393196,-14.75,-5.97851309925318));
#33289=CARTESIAN_POINT('Ctrl Pts',(19.638131082058,-14.75,-5.61732616275549));
#33290=CARTESIAN_POINT('Ctrl Pts',(19.5665074586868,-15.,-7.0590041950345));
#33291=CARTESIAN_POINT('Ctrl Pts',(19.5665074586868,-14.75,-7.0590041950345));
#33292=CARTESIAN_POINT('Ctrl Pts',(19.4488404393196,-15.,-6.74795377999544));
#33293=CARTESIAN_POINT('Ctrl Pts',(19.4488404393196,-14.75,-6.74795377999544));
#33294=CARTESIAN_POINT('Ctrl Pts',(19.4488404393196,-15.,-6.42053220421076));
#33295=CARTESIAN_POINT('Ctrl Pts',(19.4488404393196,-14.75,-6.42053220421076));
#33296=CARTESIAN_POINT('',(19.5665074586868,-14.75,-7.0590041950345));
#33297=CARTESIAN_POINT('',(19.5665074586868,-15.,-7.0590041950345));
#33298=CARTESIAN_POINT('Ctrl Pts',(19.5665074586868,-14.75,-7.0590041950345));
#33299=CARTESIAN_POINT('Ctrl Pts',(19.4488404393196,-14.75,-6.74795377999544));
#33300=CARTESIAN_POINT('Ctrl Pts',(19.4488404393196,-14.75,-6.42053220421076));
#33301=CARTESIAN_POINT('Ctrl Pts',(19.9174625873566,-15.,-7.66268793493509));
#33302=CARTESIAN_POINT('Ctrl Pts',(19.9174625873566,-14.75,-7.66268793493509));
#33303=CARTESIAN_POINT('Ctrl Pts',(19.684174478054,-15.,-7.37005475908518));
#33304=CARTESIAN_POINT('Ctrl Pts',(19.684174478054,-14.75,-7.37005475908518));
#33305=CARTESIAN_POINT('Ctrl Pts',(19.5665074586868,-15.,-7.0590041950345));
#33306=CARTESIAN_POINT('Ctrl Pts',(19.5665074586868,-14.75,-7.0590041950345));
#33307=CARTESIAN_POINT('',(19.9174625873566,-14.75,-7.66268793493509));
#33308=CARTESIAN_POINT('',(19.9174625873566,-15.,-7.66268793493509));
#33309=CARTESIAN_POINT('Ctrl Pts',(19.9174625873566,-14.75,-7.66268793493509));
#33310=CARTESIAN_POINT('Ctrl Pts',(19.684174478054,-14.75,-7.37005475908518));
#33311=CARTESIAN_POINT('Ctrl Pts',(19.5665074586868,-14.75,-7.0590041950345));
#33312=CARTESIAN_POINT('Origin',(21.0306958556175,-15.,-7.66268793493509));
#33313=CARTESIAN_POINT('',(21.0306958556175,-14.75,-7.66268793493509));
#33314=CARTESIAN_POINT('',(21.0306958556175,-15.,-7.66268793493509));
#33315=CARTESIAN_POINT('',(21.0306958556175,-14.75,-7.66268793493509));
#33316=CARTESIAN_POINT('Origin',(21.0286494791508,-15.,-6.39188278466463));
#33317=CARTESIAN_POINT('',(21.0286494791508,-14.75,-6.39188278466463));
#33318=CARTESIAN_POINT('',(21.0286494791508,-15.,-6.39188278466463));
#33319=CARTESIAN_POINT('',(21.0286494791508,-14.75,-6.39188278466463));
#33320=CARTESIAN_POINT('Origin',(20.6766710877419,-15.,-6.39188278466463));
#33321=CARTESIAN_POINT('',(20.6766710877419,-14.75,-6.39188278466463));
#33322=CARTESIAN_POINT('',(20.6766710877419,-15.,-6.39188278466463));
#33323=CARTESIAN_POINT('',(20.6766710877419,-14.75,-6.39188278466463));
#33324=CARTESIAN_POINT('Origin',(20.6766710877419,-15.,-7.27387461811304));
#33325=CARTESIAN_POINT('',(20.6766710877419,-14.75,-7.27387461811304));
#33326=CARTESIAN_POINT('',(20.6766710877419,-15.,-7.27387461811304));
#33327=CARTESIAN_POINT('',(20.6766710877419,-14.75,-7.27387461811304));
#33328=CARTESIAN_POINT('Origin',(20.1180080771446,-15.,-7.27387461811304));
#33329=CARTESIAN_POINT('',(20.1180080771446,-14.75,-7.27387461811304));
#33330=CARTESIAN_POINT('Origin',(21.0000000596046,-14.75,-6.27523896284401));
#33331=CARTESIAN_POINT('Origin',(15.5,-15.,-18.5));
#33332=CARTESIAN_POINT('',(8.91666666666667,8.4166666666667,-11.9166666666667));
#33333=CARTESIAN_POINT('',(22.5,8.00000000000003,-25.5));
#33334=CARTESIAN_POINT('Origin',(15.25,14.75,-9.5));
#33335=CARTESIAN_POINT('',(5.74999999999999,5.25000000000004,8.74999999999999));
#33336=CARTESIAN_POINT('Origin',(27.,14.75,-18.75));
#33337=CARTESIAN_POINT('Origin',(31.,-15.,-3.46410161513775));
#33338=CARTESIAN_POINT('',(28.,-15.,-1.73205080756888));
#33339=CARTESIAN_POINT('Origin',(15.5,-15.,18.5));
#33340=CARTESIAN_POINT('Origin',(28.,-15.,1.73205080756888));
#33341=CARTESIAN_POINT('',(28.,-15.,1.73205080756888));
#33342=CARTESIAN_POINT('Origin',(28.,-15.,-1.73205080756888));
#33343=CARTESIAN_POINT('',(0.,0.,0.));
#33344=CARTESIAN_POINT('Origin',(-11.,2.6,0.));
#33345=CARTESIAN_POINT('',(-11.,-2.6,-3.18408167778312E-16));
#33346=CARTESIAN_POINT('Origin',(-11.,0.,0.));
#33347=CARTESIAN_POINT('Origin',(-10.8,0.,0.));
#33348=CARTESIAN_POINT('',(-10.6,-3.,-3.67394039744206E-16));
#33349=CARTESIAN_POINT('Origin',(-10.6,0.,0.));
#33350=CARTESIAN_POINT('',(-10.8,-2.8,-3.42901103761259E-16));
#33351=CARTESIAN_POINT('Origin',(-9.695,0.,0.));
#33352=CARTESIAN_POINT('',(-8.79,-3.,-3.67394039744206E-16));
#33353=CARTESIAN_POINT('Origin',(-8.79,0.,0.));
#33354=CARTESIAN_POINT('',(-9.695,-3.,-3.67394039744206E-16));
#33355=CARTESIAN_POINT('Origin',(-8.79,2.5,0.));
#33356=CARTESIAN_POINT('',(-8.79,-2.5,-3.06161699786838E-16));
#33357=CARTESIAN_POINT('Origin',(-8.79,0.,0.));
#33358=CARTESIAN_POINT('Origin',(-8.42,0.,0.));
#33359=CARTESIAN_POINT('',(-8.05,-2.5,-3.06161699786838E-16));
#33360=CARTESIAN_POINT('Origin',(-8.05,0.,0.));
#33361=CARTESIAN_POINT('',(-8.42,-2.5,-3.06161699786838E-16));
#33362=CARTESIAN_POINT('Origin',(-8.05,3.,0.));
#33363=CARTESIAN_POINT('',(-8.05,-3.,-3.67394039744206E-16));
#33364=CARTESIAN_POINT('Origin',(-8.05,0.,0.));
#33365=CARTESIAN_POINT('Origin',(0.,0.,0.));
#33366=CARTESIAN_POINT('',(8.05,-3.,-3.67394039744206E-16));
#33367=CARTESIAN_POINT('Origin',(8.05,0.,0.));
#33368=CARTESIAN_POINT('',(0.,-3.,-3.67394039744206E-16));
#33369=CARTESIAN_POINT('Origin',(8.05,2.5,0.));
#33370=CARTESIAN_POINT('',(8.05,-2.5,-3.06161699786838E-16));
#33371=CARTESIAN_POINT('Origin',(8.05,0.,0.));
#33372=CARTESIAN_POINT('Origin',(8.42,0.,0.));
#33373=CARTESIAN_POINT('',(8.79,-2.5,-3.06161699786838E-16));
#33374=CARTESIAN_POINT('Origin',(8.79,0.,0.));
#33375=CARTESIAN_POINT('',(8.42,-2.5,-3.06161699786838E-16));
#33376=CARTESIAN_POINT('Origin',(8.79,3.,0.));
#33377=CARTESIAN_POINT('',(8.79,-3.,-3.67394039744206E-16));
#33378=CARTESIAN_POINT('Origin',(8.79,0.,0.));
#33379=CARTESIAN_POINT('Origin',(9.695,0.,0.));
#33380=CARTESIAN_POINT('',(10.6,-3.,-3.67394039744206E-16));
#33381=CARTESIAN_POINT('Origin',(10.6,0.,0.));
#33382=CARTESIAN_POINT('',(9.695,-3.,-3.67394039744206E-16));
#33383=CARTESIAN_POINT('Origin',(10.8,0.,0.));
#33384=CARTESIAN_POINT('',(11.,-2.6,-3.18408167778312E-16));
#33385=CARTESIAN_POINT('Origin',(11.,0.,0.));
#33386=CARTESIAN_POINT('',(10.8,-2.8,-3.42901103761259E-16));
#33387=CARTESIAN_POINT('Origin',(11.,0.,0.));
#33388=CARTESIAN_POINT('',(0.,0.,0.));
#33389=CARTESIAN_POINT('Origin',(212.6,0.,0.));
#33390=CARTESIAN_POINT('',(204.481156847152,-11.9249052711737,0.000302535951811622));
#33391=CARTESIAN_POINT('',(204.268843152848,-11.9248035800407,0.000218476360169007));
#33392=CARTESIAN_POINT('',(212.6,-11.925,-1.46039130798322E-15));
#33393=CARTESIAN_POINT('',(204.,5.12964461189265,10.7653319110783));
#33394=CARTESIAN_POINT('Ctrl Pts',(204.481156847152,-11.9249052711737,0.000302535951811622));
#33395=CARTESIAN_POINT('Ctrl Pts',(204.471375386274,-11.9253914263212,0.488902467455807));
#33396=CARTESIAN_POINT('Ctrl Pts',(204.461593925397,-11.8959222415045,0.977444055122396));
#33397=CARTESIAN_POINT('Ctrl Pts',(204.451812464519,-11.8360320098832,1.46222727880249));
#33398=CARTESIAN_POINT('Ctrl Pts',(204.412321413966,-11.5942349824066,3.41946035810522));
#33399=CARTESIAN_POINT('Ctrl Pts',(204.372830363414,-10.8565722369881,5.31543177641324));
#33400=CARTESIAN_POINT('Ctrl Pts',(204.333339312861,-9.71202673712791,6.92143673402461));
#33401=CARTESIAN_POINT('Ctrl Pts',(204.293848262308,-8.56748123726774,8.52744169163597));
#33402=CARTESIAN_POINT('Ctrl Pts',(204.254357211755,-7.01605298296593,9.84348018855067));
#33403=CARTESIAN_POINT('Ctrl Pts',(204.214866161202,-5.24489388990008,10.7107847596565));
#33404=CARTESIAN_POINT('Ctrl Pts',(204.17537511065,-3.47373479683424,11.5780893307624));
#33405=CARTESIAN_POINT('Ctrl Pts',(204.135884060097,-1.48284486500436,11.9966599760593));
#33406=CARTESIAN_POINT('Ctrl Pts',(204.096393009544,0.487620662860904,11.9160328022271));
#33407=CARTESIAN_POINT('Ctrl Pts',(204.064262006363,2.09084552668397,11.850432319519));
#33408=CARTESIAN_POINT('Ctrl Pts',(204.032131003181,3.68054964658133,11.4543680498425));
#33409=CARTESIAN_POINT('Ctrl Pts',(204.,5.1300262208937,10.7654810839693));
#33410=CARTESIAN_POINT('',(204.,-5.12964461189138,10.7653319110789));
#33411=CARTESIAN_POINT('Origin',(204.,0.,0.));
#33412=CARTESIAN_POINT('Ctrl Pts',(204.,-5.12964461189138,10.7653319110789));
#33413=CARTESIAN_POINT('Ctrl Pts',(204.039491050553,-6.91044286403787,9.91678750627631));
#33414=CARTESIAN_POINT('Ctrl Pts',(204.078982101106,-8.47572680110246,8.61820334451372));
#33415=CARTESIAN_POINT('Ctrl Pts',(204.118473151658,-9.63736634999488,7.02480970362073));
#33416=CARTESIAN_POINT('Ctrl Pts',(204.157964202211,-10.7990058988873,5.43141606272772));
#33417=CARTESIAN_POINT('Ctrl Pts',(204.197455252764,-11.5570010596076,3.54321294270431));
#33418=CARTESIAN_POINT('Ctrl Pts',(204.236946303317,-11.8197391311641,1.58862178928765));
#33419=CARTESIAN_POINT('Ctrl Pts',(204.247578586494,-11.8904768182884,1.06238188561764));
#33420=CARTESIAN_POINT('Ctrl Pts',(204.258210869671,-11.9253151710161,0.531329761662712));
#33421=CARTESIAN_POINT('Ctrl Pts',(204.268843152848,-11.9248035800407,0.000218476360169007));
#33422=CARTESIAN_POINT('Origin',(212.6,0.,0.));
#33423=CARTESIAN_POINT('',(205.981156847152,-11.9257948710858,-0.00017386328305502));
#33424=CARTESIAN_POINT('',(205.768843152848,-11.925879493633,-0.000136868446097685));
#33425=CARTESIAN_POINT('',(212.6,-11.925,-1.46039130798322E-15));
#33426=CARTESIAN_POINT('Ctrl Pts',(205.981156847152,-11.9257948710858,-0.00017386328305502));
#33427=CARTESIAN_POINT('Ctrl Pts',(205.945267992908,-11.9245188658506,1.79214687948621));
#33428=CARTESIAN_POINT('Ctrl Pts',(205.909379138663,-11.5147464964249,3.58503144351514));
#33429=CARTESIAN_POINT('Ctrl Pts',(205.873490284419,-10.7335884774596,5.19806139375664));
#33430=CARTESIAN_POINT('Ctrl Pts',(205.833999233866,-9.87402493144417,6.97299259870679));
#33431=CARTESIAN_POINT('Ctrl Pts',(205.794508183313,-8.56478166178296,8.53015294168481));
#33432=CARTESIAN_POINT('Ctrl Pts',(205.755017132761,-6.96379286278294,9.68170195869235));
#33433=CARTESIAN_POINT('Ctrl Pts',(205.715526082208,-5.36280406378292,10.8332509756999));
#33434=CARTESIAN_POINT('Ctrl Pts',(205.676035031655,-3.47006973544408,11.579188666737));
#33435=CARTESIAN_POINT('Ctrl Pts',(205.636543981102,-1.51391067883033,11.8295324642507));
#33436=CARTESIAN_POINT('Ctrl Pts',(205.59705293055,0.442248377783413,12.0798762617644));
#33437=CARTESIAN_POINT('Ctrl Pts',(205.557561879997,2.46183216267207,11.8346261657547));
#33438=CARTESIAN_POINT('Ctrl Pts',(205.518070829444,4.30121800879738,11.1233667329109));
#33439=CARTESIAN_POINT('Ctrl Pts',(205.478579778891,6.14060385492269,10.4121073000672));
#33440=CARTESIAN_POINT('Ctrl Pts',(205.439088728338,7.79979176228466,9.23483853038924));
#33441=CARTESIAN_POINT('Ctrl Pts',(205.399597677786,9.07863366507509,7.73357450785956));
#33442=CARTESIAN_POINT('Ctrl Pts',(205.360106627233,10.3574755678655,6.23231048532987));
#33443=CARTESIAN_POINT('Ctrl Pts',(205.32061557668,11.2559714660844,4.40705120994843));
#33444=CARTESIAN_POINT('Ctrl Pts',(205.281124526127,11.6657356806046,2.47797797538542));
#33445=CARTESIAN_POINT('Ctrl Pts',(205.241633475575,12.0754998951248,0.548904740822421));
#33446=CARTESIAN_POINT('Ctrl Pts',(205.202142425022,11.9965324259463,-1.48398245292214));
#33447=CARTESIAN_POINT('Ctrl Pts',(205.162651374469,11.43835912164,-3.37545618326797));
#33448=CARTESIAN_POINT('Ctrl Pts',(205.123160323916,10.8801858173337,-5.2669299136138));
#33449=CARTESIAN_POINT('Ctrl Pts',(205.083669273363,9.84280667789951,-7.01699018056091));
#33450=CARTESIAN_POINT('Ctrl Pts',(205.044178222811,8.45136090743825,-8.41452689692128));
#33451=CARTESIAN_POINT('Ctrl Pts',(205.004687172258,7.059915136977,-9.81206361328165));
#33452=CARTESIAN_POINT('Ctrl Pts',(204.965196121705,5.31440273548863,-10.8570767790553));
#33453=CARTESIAN_POINT('Ctrl Pts',(204.925705071152,3.42538506743283,-11.4235064763634));
#33454=CARTESIAN_POINT('Ctrl Pts',(204.8862140206,1.53636739937703,-11.9899361736716));
#33455=CARTESIAN_POINT('Ctrl Pts',(204.846722970047,-0.496155535246199,
-12.0777824025142));
#33456=CARTESIAN_POINT('Ctrl Pts',(204.807231919494,-2.42700014393072,-11.6764479195652));
#33457=CARTESIAN_POINT('Ctrl Pts',(204.767740868941,-4.35784475261525,-11.2751134366161));
#33458=CARTESIAN_POINT('Ctrl Pts',(204.728249818389,-6.18701103536108,-10.3845982418754));
#33459=CARTESIAN_POINT('Ctrl Pts',(204.688758767836,-7.69384656645438,-9.11232601683176));
#33460=CARTESIAN_POINT('Ctrl Pts',(204.649267717283,-9.20068209754767,-7.84005379178813));
#33461=CARTESIAN_POINT('Ctrl Pts',(204.60977666673,-10.3851868769884,-6.18602453644161));
#33462=CARTESIAN_POINT('Ctrl Pts',(204.570285616177,-11.1044736119415,-4.34976253861964));
#33463=CARTESIAN_POINT('Ctrl Pts',(204.540576026502,-11.6456016258877,-2.96832067450525));
#33464=CARTESIAN_POINT('Ctrl Pts',(204.510866436827,-11.9234286543235,-1.48373994625058));
#33465=CARTESIAN_POINT('Ctrl Pts',(204.481156847152,-11.9249052711737,0.000302535951811622));
#33466=CARTESIAN_POINT('Ctrl Pts',(204.268843152848,-11.9248035800407,0.000218476360169007));
#33467=CARTESIAN_POINT('Ctrl Pts',(204.297701920224,-11.9234149897725,-1.44135496348323));
#33468=CARTESIAN_POINT('Ctrl Pts',(204.326560687599,-11.6615962792732,-2.88336425683184));
#33469=CARTESIAN_POINT('Ctrl Pts',(204.355419454975,-11.1503333329718,-4.23076491755909));
#33470=CARTESIAN_POINT('Ctrl Pts',(204.394910505528,-10.4507084808302,-6.07458128417927));
#33471=CARTESIAN_POINT('Ctrl Pts',(204.43440155608,-9.28397779415416,-7.7412348306097));
#33472=CARTESIAN_POINT('Ctrl Pts',(204.473892606633,-7.7908367643509,-9.02955893682934));
#33473=CARTESIAN_POINT('Ctrl Pts',(204.513383657186,-6.29769573454765,-10.317883043049));
#33474=CARTESIAN_POINT('Ctrl Pts',(204.552874707739,-4.47814436161721,-11.2278777090578));
#33475=CARTESIAN_POINT('Ctrl Pts',(204.592365758292,-2.55169822806604,-11.6498261182712));
#33476=CARTESIAN_POINT('Ctrl Pts',(204.631856808844,-0.625252094514863,
-12.0717745274846));
#33477=CARTESIAN_POINT('Ctrl Pts',(204.671347859397,1.40808879965704,-12.0056766799026));
#33478=CARTESIAN_POINT('Ctrl Pts',(204.71083890995,3.30305318516678,-11.4594791445967));
#33479=CARTESIAN_POINT('Ctrl Pts',(204.750329960503,5.19801757067652,-10.9132816092908));
#33480=CARTESIAN_POINT('Ctrl Pts',(204.789821011055,6.9546054475241,-9.886984386261));
#33481=CARTESIAN_POINT('Ctrl Pts',(204.829312061608,8.36091415185001,-8.50440268311452));
#33482=CARTESIAN_POINT('Ctrl Pts',(204.868803112161,9.76722285617592,-7.12182097996805));
#33483=CARTESIAN_POINT('Ctrl Pts',(204.908294162714,10.8232523879802,-5.38295479670486));
#33484=CARTESIAN_POINT('Ctrl Pts',(204.947785213267,11.401616262652,-3.49755765611992));
#33485=CARTESIAN_POINT('Ctrl Pts',(204.987276263819,11.9799801373238,-1.61216051553499));
#33486=CARTESIAN_POINT('Ctrl Pts',(205.026767314372,12.0806783548632,0.419767582371721));
#33487=CARTESIAN_POINT('Ctrl Pts',(205.066258364925,11.6915624780006,2.3531119337468));
#33488=CARTESIAN_POINT('Ctrl Pts',(205.105749415478,11.3024466011381,4.28645628512189));
#33489=CARTESIAN_POINT('Ctrl Pts',(205.14524046603,10.4235166298735,6.12121688996534));
#33490=CARTESIAN_POINT('Ctrl Pts',(205.184731516583,9.16079857987295,7.63606773280669));
#33491=CARTESIAN_POINT('Ctrl Pts',(205.224222567136,7.89808052987239,9.15091857564802));
#33492=CARTESIAN_POINT('Ctrl Pts',(205.263713617689,6.25157440113582,10.3458596564872));
#33493=CARTESIAN_POINT('Ctrl Pts',(205.303204668241,4.41989817863815,11.0767443960842));
#33494=CARTESIAN_POINT('Ctrl Pts',(205.342695718794,2.58822195614046,11.8076291356812));
#33495=CARTESIAN_POINT('Ctrl Pts',(205.382186769347,0.571375639881673,12.0744575340359));
#33496=CARTESIAN_POINT('Ctrl Pts',(205.4216778199,-1.38734819215102,11.8450423672815));
#33497=CARTESIAN_POINT('Ctrl Pts',(205.461168870453,-3.34607202418372,11.615627200527));
#33498=CARTESIAN_POINT('Ctrl Pts',(205.500659921005,-5.24667337199031,10.8899684686634));
#33499=CARTESIAN_POINT('Ctrl Pts',(205.540150971558,-6.85988249812762,9.75560232941972));
#33500=CARTESIAN_POINT('Ctrl Pts',(205.579642022111,-8.47309162426492,8.62123619017606));
#33501=CARTESIAN_POINT('Ctrl Pts',(205.619133072664,-9.79890852873291,7.07816264355239));
#33502=CARTESIAN_POINT('Ctrl Pts',(205.658624123216,-10.6773997071198,5.31252293613964));
#33503=CARTESIAN_POINT('Ctrl Pts',(205.69536379976,-11.4946856817605,3.66989680096673));
#33504=CARTESIAN_POINT('Ctrl Pts',(205.732103476304,-11.9248057040004,1.83463689896584));
#33505=CARTESIAN_POINT('Ctrl Pts',(205.768843152848,-11.925879493633,-0.000136868446097685));
#33506=CARTESIAN_POINT('Origin',(212.6,0.,0.));
#33507=CARTESIAN_POINT('',(207.481156847152,-11.9240882605208,-0.000122447896127587));
#33508=CARTESIAN_POINT('',(207.268843152848,-11.9241429677904,-0.000156968565329557));
#33509=CARTESIAN_POINT('',(212.6,-11.925,-1.46039130798322E-15));
#33510=CARTESIAN_POINT('Ctrl Pts',(207.481156847152,-11.9240882605208,-0.000122447896127587));
#33511=CARTESIAN_POINT('Ctrl Pts',(207.458651650094,-11.9236789998492,1.12426988415646));
#33512=CARTESIAN_POINT('Ctrl Pts',(207.436146453035,-11.7658768963148,2.24877473613482));
#33513=CARTESIAN_POINT('Ctrl Pts',(207.413641255977,-11.4522567635277,3.32799923052405));
#33514=CARTESIAN_POINT('Ctrl Pts',(207.374150205424,-10.9019310549283,5.22177109821098));
#33515=CARTESIAN_POINT('Ctrl Pts',(207.334659154872,-9.87181728028402,6.97611766767221));
#33516=CARTESIAN_POINT('Ctrl Pts',(207.295168104319,-8.48617820498044,8.37941187252719));
#33517=CARTESIAN_POINT('Ctrl Pts',(207.255677053766,-7.10053912967688,9.78270607738215));
#33518=CARTESIAN_POINT('Ctrl Pts',(207.216186003213,-5.35937475371405,10.8349479176309));
#33519=CARTESIAN_POINT('Ctrl Pts',(207.17669495266,-3.47272197366958,11.4092053163104));
#33520=CARTESIAN_POINT('Ctrl Pts',(207.137203902108,-1.5860691936251,11.98346271499));
#33521=CARTESIAN_POINT('Ctrl Pts',(207.097712851555,0.446071990500981,12.0797356721004));
#33522=CARTESIAN_POINT('Ctrl Pts',(207.058221801002,2.3785641100045,11.6864107676709));
#33523=CARTESIAN_POINT('Ctrl Pts',(207.018730750449,4.31105622950802,11.2930858632414));
#33524=CARTESIAN_POINT('Ctrl Pts',(206.979239699897,6.14389928438897,10.4101630972718));
#33525=CARTESIAN_POINT('Ctrl Pts',(206.939748649344,7.65599716650529,9.14414956366061));
#33526=CARTESIAN_POINT('Ctrl Pts',(206.900257598791,9.16809504862161,7.87813603004939));
#33527=CARTESIAN_POINT('Ctrl Pts',(206.860766548238,10.3594477579733,6.22903172879648));
#33528=CARTESIAN_POINT('Ctrl Pts',(206.821275497686,11.0863422544498,4.39576833708731));
#33529=CARTESIAN_POINT('Ctrl Pts',(206.781784447133,11.8132367509262,2.56250494537814));
#33530=CARTESIAN_POINT('Ctrl Pts',(206.74229339658,12.0756730345274,0.545082463212723));
#33531=CARTESIAN_POINT('Ctrl Pts',(206.702802346027,11.8419933805049,-1.41313715973078));
#33532=CARTESIAN_POINT('Ctrl Pts',(206.663311295474,11.6083137264823,-3.37135678267428));
#33533=CARTESIAN_POINT('Ctrl Pts',(206.623820244922,10.8785181348361,-5.27037354639587));
#33534=CARTESIAN_POINT('Ctrl Pts',(206.584329194369,9.74064194750141,-6.8811087992197));
#33535=CARTESIAN_POINT('Ctrl Pts',(206.544838143816,8.60276576016673,-8.49184405204354));
#33536=CARTESIAN_POINT('Ctrl Pts',(206.505347093263,7.05680897714361,-9.8142977939696));
#33537=CARTESIAN_POINT('Ctrl Pts',(206.465856042711,5.28926057640347,-10.6889422494037));
#33538=CARTESIAN_POINT('Ctrl Pts',(206.426364992158,3.52171217566333,-11.5635867048377));
#33539=CARTESIAN_POINT('Ctrl Pts',(206.386873941605,1.53257215720617,-11.9904218737798));
#33540=CARTESIAN_POINT('Ctrl Pts',(206.347382891052,-0.438209246759027,
-11.917958571503));
#33541=CARTESIAN_POINT('Ctrl Pts',(206.307891840499,-2.40899065072422,-11.8454952692263));
#33542=CARTESIAN_POINT('Ctrl Pts',(206.268400789947,-4.36141344019744,-11.2737334957307));
#33543=CARTESIAN_POINT('Ctrl Pts',(206.228909739394,-6.05995658730328,-10.2716449518268));
#33544=CARTESIAN_POINT('Ctrl Pts',(206.189418688841,-7.75849973440911,-9.26955640792297));
#33545=CARTESIAN_POINT('Ctrl Pts',(206.149927638288,-9.20316323914755,-7.83714109361087));
#33546=CARTESIAN_POINT('Ctrl Pts',(206.110436587736,-10.2196771455715,-6.14719146407803));
#33547=CARTESIAN_POINT('Ctrl Pts',(206.070945537183,-11.2361910519954,-4.45724183454519));
#33548=CARTESIAN_POINT('Ctrl Pts',(206.03145448663,-11.8245553601048,-2.50975788979161));
#33549=CARTESIAN_POINT('Ctrl Pts',(205.991963436077,-11.9137956029747,-0.539664883953685));
#33550=CARTESIAN_POINT('Ctrl Pts',(205.988361239769,-11.9219356972222,-0.359961846084769));
#33551=CARTESIAN_POINT('Ctrl Pts',(205.98475904346,-11.9259229448693,-0.180070694740662));
#33552=CARTESIAN_POINT('Ctrl Pts',(205.981156847152,-11.9257948710858,-0.00017386328305502));
#33553=CARTESIAN_POINT('Ctrl Pts',(205.768843152848,-11.925879493633,-0.000136868446097685));
#33554=CARTESIAN_POINT('Ctrl Pts',(205.771594526857,-11.9259599079742,-0.137540061143698));
#33555=CARTESIAN_POINT('Ctrl Pts',(205.774345900866,-11.923634116918,-0.274940527469211));
#33556=CARTESIAN_POINT('Ctrl Pts',(205.777097274875,-11.9188845310052,-0.412257158256467));
#33557=CARTESIAN_POINT('Ctrl Pts',(205.816588325427,-11.8507127241981,-2.38319167703802));
#33558=CARTESIAN_POINT('Ctrl Pts',(205.85607937598,-11.2832036582781,-4.33685484639931));
#33559=CARTESIAN_POINT('Ctrl Pts',(205.895570426533,-10.2848160225208,-6.03757599437023));
#33560=CARTESIAN_POINT('Ctrl Pts',(205.935061477086,-9.28642838676358,-7.73829714234115));
#33561=CARTESIAN_POINT('Ctrl Pts',(205.974552527639,-7.85716218116911,-9.18607626892171));
#33562=CARTESIAN_POINT('Ctrl Pts',(206.014043578191,-6.16942998670385,-10.2062675883473));
#33563=CARTESIAN_POINT('Ctrl Pts',(206.053534628744,-4.48169779223858,-11.2264589077728));
#33564=CARTESIAN_POINT('Ctrl Pts',(206.093025679297,-2.53549960890252,-11.8190624200434));
#33565=CARTESIAN_POINT('Ctrl Pts',(206.13251672985,-0.565605587893831,-11.9125922786295));
#33566=CARTESIAN_POINT('Ctrl Pts',(206.172007780402,1.40428843311484,-12.0061221372157));
#33567=CARTESIAN_POINT('Ctrl Pts',(206.211498830955,3.39787829179614,-11.6005783421175));
#33568=CARTESIAN_POINT('Ctrl Pts',(206.250989881508,5.17467697034661,-10.7448816986032));
#33569=CARTESIAN_POINT('Ctrl Pts',(206.290480932061,6.95147564889709,-9.88918505508886));
#33570=CARTESIAN_POINT('Ctrl Pts',(206.329971982613,8.51148314731673,-8.58333556315843));
#33571=CARTESIAN_POINT('Ctrl Pts',(206.369463033166,9.66651554827986,-6.98485802456189));
#33572=CARTESIAN_POINT('Ctrl Pts',(206.408954083719,10.821547949243,-5.38638048596536));
#33573=CARTESIAN_POINT('Ctrl Pts',(206.448445134272,11.5716052527496,-3.49527490070271));
#33574=CARTESIAN_POINT('Ctrl Pts',(206.487936184825,11.8262079436201,-1.5396655943414));
#33575=CARTESIAN_POINT('Ctrl Pts',(206.527427235377,12.0808106344906,0.415943712019895));
#33576=CARTESIAN_POINT('Ctrl Pts',(206.56691828593,11.839958712725,2.43605673947986));
#33577=CARTESIAN_POINT('Ctrl Pts',(206.606409336483,11.1327061786376,4.27698697771965));
#33578=CARTESIAN_POINT('Ctrl Pts',(206.645900387036,10.4254536445503,6.11791721595947));
#33579=CARTESIAN_POINT('Ctrl Pts',(206.685391437588,9.25180049814112,7.77966466497909));
#33580=CARTESIAN_POINT('Ctrl Pts',(206.724882488141,7.75332467878485,9.06177250285198));
#33581=CARTESIAN_POINT('Ctrl Pts',(206.764373538694,6.25484885942861,10.3438803407248));
#33582=CARTESIAN_POINT('Ctrl Pts',(206.803864589247,4.43155036712525,11.246348567451));
#33583=CARTESIAN_POINT('Ctrl Pts',(206.8433556398,2.50337394814799,11.6603123175776));
#33584=CARTESIAN_POINT('Ctrl Pts',(206.882846690352,0.575197529170728,12.0742760677042));
#33585=CARTESIAN_POINT('Ctrl Pts',(206.922337740905,-1.45785681648046,11.9997353412312));
#33586=CARTESIAN_POINT('Ctrl Pts',(206.961828791458,-3.35054146531087,11.4456819961558));
#33587=CARTESIAN_POINT('Ctrl Pts',(207.001319842011,-5.24322611414129,10.8916286510803));
#33588=CARTESIAN_POINT('Ctrl Pts',(207.040810892563,-6.99554106615095,9.85806268740243));
#33589=CARTESIAN_POINT('Ctrl Pts',(207.080301943116,-8.39610432924578,8.46966330855321));
#33590=CARTESIAN_POINT('Ctrl Pts',(207.119792993669,-9.79666759234061,7.08126392970398));
#33591=CARTESIAN_POINT('Ctrl Pts',(207.159284044222,-10.8454791665206,5.33803113568344));
#33592=CARTESIAN_POINT('Ctrl Pts',(207.198775094774,-11.4160207682894,3.45025133661703));
#33593=CARTESIAN_POINT('Ctrl Pts',(207.222131114132,-11.7534536931892,2.33376998417775));
#33594=CARTESIAN_POINT('Ctrl Pts',(207.24548713349,-11.9235953034982,1.16672836266624));
#33595=CARTESIAN_POINT('Ctrl Pts',(207.268843152848,-11.9241429677904,-0.000156968565329558));
#33596=CARTESIAN_POINT('Origin',(212.6,0.,0.));
#33597=CARTESIAN_POINT('',(208.981156847152,-11.9250072207259,0.000301374860750547));
#33598=CARTESIAN_POINT('',(208.768843152848,-11.9248763938011,0.000301080366776068));
#33599=CARTESIAN_POINT('',(212.6,-11.925,-1.46039130798322E-15));
#33600=CARTESIAN_POINT('Ctrl Pts',(208.981156847152,-11.9250072207259,0.000301374860750547));
#33601=CARTESIAN_POINT('Ctrl Pts',(208.97203530728,-11.925467717682,0.455925961038745));
#33602=CARTESIAN_POINT('Ctrl Pts',(208.962913767407,-11.8998498269624,0.91149906648302));
#33603=CARTESIAN_POINT('Ctrl Pts',(208.953792227535,-11.8477510063931,1.36402344065116));
#33604=CARTESIAN_POINT('Ctrl Pts',(208.914301176982,-11.6221929114159,3.3231951580302));
#33605=CARTESIAN_POINT('Ctrl Pts',(208.87481012643,-10.9002776652053,5.2252216173048));
#33606=CARTESIAN_POINT('Ctrl Pts',(208.835319075877,-9.76909000255087,6.84066110680794));
#33607=CARTESIAN_POINT('Ctrl Pts',(208.795828025324,-8.63790233989649,8.45610059631109));
#33608=CARTESIAN_POINT('Ctrl Pts',(208.756336974771,-7.0974422607984,9.78495311604276));
#33609=CARTESIAN_POINT('Ctrl Pts',(208.716845924218,-5.33353567508007,10.666919004979));
#33610=CARTESIAN_POINT('Ctrl Pts',(208.677354873666,-3.5696290893617,11.5488848939153));
#33611=CARTESIAN_POINT('Ctrl Pts',(208.637863823113,-1.58227599702309,11.9839641520561));
#33612=CARTESIAN_POINT('Ctrl Pts',(208.59837277256,0.388788926863556,11.9196731090447));
#33613=CARTESIAN_POINT('Ctrl Pts',(208.558881722007,2.3598538507502,11.8553820660332));
#33614=CARTESIAN_POINT('Ctrl Pts',(208.519390671455,4.31463060618487,11.2917207218694));
#33615=CARTESIAN_POINT('Ctrl Pts',(208.479899620902,6.01731420606716,10.296683621516));
#33616=CARTESIAN_POINT('Ctrl Pts',(208.440408570349,7.71999780594943,9.30164652116268));
#33617=CARTESIAN_POINT('Ctrl Pts',(208.400917519796,9.17058825027933,7.87523366461978));
#33618=CARTESIAN_POINT('Ctrl Pts',(208.361426469244,10.1941006155549,6.18951342967102));
#33619=CARTESIAN_POINT('Ctrl Pts',(208.321935418691,11.2176129808304,4.50379319472225));
#33620=CARTESIAN_POINT('Ctrl Pts',(208.282444368138,11.8140472670516,2.55876558136763));
#33621=CARTESIAN_POINT('Ctrl Pts',(208.242953317585,11.9114555247774,0.589059536366358));
#33622=CARTESIAN_POINT('Ctrl Pts',(208.203462267032,12.0088637825032,-1.38064650863491));
#33623=CARTESIAN_POINT('Ctrl Pts',(208.16397121648,11.6072460117335,-3.37503098528282));
#33624=CARTESIAN_POINT('Ctrl Pts',(208.124480165927,10.7550494190316,-5.1535110216552));
#33625=CARTESIAN_POINT('Ctrl Pts',(208.084989115374,9.9028528263298,-6.93199105802757));
#33626=CARTESIAN_POINT('Ctrl Pts',(208.045498064821,8.60007741169578,-8.4945666541244));
#33627=CARTESIAN_POINT('Ctrl Pts',(208.006007014269,7.00387715140256,-9.65274410228489));
#33628=CARTESIAN_POINT('Ctrl Pts',(207.966515963716,5.40767689110933,-10.8109215504454));
#33629=CARTESIAN_POINT('Ctrl Pts',(207.927024913163,3.51805178515689,-11.5647008506695));
#33630=CARTESIAN_POINT('Ctrl Pts',(207.88753386261,1.56294756826656,-11.8231535029781));
#33631=CARTESIAN_POINT('Ctrl Pts',(207.848042812058,-0.39215664862377,-12.0816061552867));
#33632=CARTESIAN_POINT('Ctrl Pts',(207.808551761505,-2.41273997645199,-11.8447321596798));
#33633=CARTESIAN_POINT('Ctrl Pts',(207.769060710952,-4.25505917229834,-11.1411056586128));
#33634=CARTESIAN_POINT('Ctrl Pts',(207.729569660399,-6.09737836814469,-10.4374791575458));
#33635=CARTESIAN_POINT('Ctrl Pts',(207.690078609846,-7.76143343200917,-9.26710015101879));
#33636=CARTESIAN_POINT('Ctrl Pts',(207.650587559294,-9.04648917416844,-7.77115161850466));
#33637=CARTESIAN_POINT('Ctrl Pts',(207.611096508741,-10.3315449163277,-6.27520308599052));
#33638=CARTESIAN_POINT('Ctrl Pts',(207.571605458188,-11.2376013367818,-4.45368502748925));
#33639=CARTESIAN_POINT('Ctrl Pts',(207.532114407635,-11.6553607257316,-2.52632741528232));
#33640=CARTESIAN_POINT('Ctrl Pts',(207.515128554141,-11.8350470009086,-1.69733417316286));
#33641=CARTESIAN_POINT('Ctrl Pts',(207.498142700646,-11.9243971510314,-0.848760359091592));
#33642=CARTESIAN_POINT('Ctrl Pts',(207.481156847152,-11.9240882605208,-0.000122447896127587));
#33643=CARTESIAN_POINT('Ctrl Pts',(207.268843152848,-11.9241429677904,-0.000156968565329558));
#33644=CARTESIAN_POINT('Ctrl Pts',(207.284978184043,-11.9245213105338,-0.806275979334776));
#33645=CARTESIAN_POINT('Ctrl Pts',(207.301113215238,-11.8439616826702,-1.61232040125019));
#33646=CARTESIAN_POINT('Ctrl Pts',(207.317248246433,-11.6817049171041,-2.40156921564886));
#33647=CARTESIAN_POINT('Ctrl Pts',(207.356739296986,-11.2845758347925,-4.33328316473606));
#33648=CARTESIAN_POINT('Ctrl Pts',(207.396230347538,-10.3980460408117,-6.1643842587982));
#33649=CARTESIAN_POINT('Ctrl Pts',(207.435721398091,-9.12905774534167,-7.67398652266591));
#33650=CARTESIAN_POINT('Ctrl Pts',(207.475212448644,-7.86006944987165,-9.18358878653363));
#33651=CARTESIAN_POINT('Ctrl Pts',(207.514703499197,-6.20862265291245,-10.3716922202069));
#33652=CARTESIAN_POINT('Ctrl Pts',(207.554194549749,-4.37393160722762,-11.0949757441439));
#33653=CARTESIAN_POINT('Ctrl Pts',(207.593685600302,-2.53924056154279,-11.8182592680808));
#33654=CARTESIAN_POINT('Ctrl Pts',(207.633176650855,-0.521305267132348,
-12.0767228822814));
#33655=CARTESIAN_POINT('Ctrl Pts',(207.672667701408,1.43645046571683,-11.8391880856495));
#33656=CARTESIAN_POINT('Ctrl Pts',(207.712158751961,3.39420619856601,-11.6016532890176));
#33657=CARTESIAN_POINT('Ctrl Pts',(207.751649802513,5.29178236985393,-10.8681200815533));
#33658=CARTESIAN_POINT('Ctrl Pts',(207.791140853066,6.90027410676151,-9.7270746742996));
#33659=CARTESIAN_POINT('Ctrl Pts',(207.830631903619,8.50876584366908,-8.58602926704593));
#33660=CARTESIAN_POINT('Ctrl Pts',(207.870122954172,9.8281731461963,-7.03747166000294));
#33661=CARTESIAN_POINT('Ctrl Pts',(207.909614004724,10.6993357311611,-5.26820456889654));
#33662=CARTESIAN_POINT('Ctrl Pts',(207.949105055277,11.570498316126,-3.49893747779013));
#33663=CARTESIAN_POINT('Ctrl Pts',(207.98859610583,11.9934161835284,-1.5089609026203));
#33664=CARTESIAN_POINT('Ctrl Pts',(208.028087156383,11.9170726932381,0.461674010448334));
#33665=CARTESIAN_POINT('Ctrl Pts',(208.067578206935,11.8407292029477,2.43230892351694));
#33666=CARTESIAN_POINT('Ctrl Pts',(208.107069257488,11.2651243549645,4.38360217448438));
#33667=CARTESIAN_POINT('Ctrl Pts',(208.146560308041,10.2596934407489,6.08016899187007));
#33668=CARTESIAN_POINT('Ctrl Pts',(208.186051358594,9.25426252653324,7.77673580925578));
#33669=CARTESIAN_POINT('Ctrl Pts',(208.225542409147,7.81900554608517,9.21857619305974));
#33670=CARTESIAN_POINT('Ctrl Pts',(208.265033459699,6.12705774506347,10.2317607407768));
#33671=CARTESIAN_POINT('Ctrl Pts',(208.304524510252,4.4351099440418,11.2449452884938));
#33672=CARTESIAN_POINT('Ctrl Pts',(208.344015560805,2.48647132244651,11.829474000124));
#33673=CARTESIAN_POINT('Ctrl Pts',(208.383506611358,0.516206423454282,11.9148350973158));
#33674=CARTESIAN_POINT('Ctrl Pts',(208.422997661911,-1.45405847553796,12.0001961945076));
#33675=CARTESIAN_POINT('Ctrl Pts',(208.462488712463,-3.44594965192712,11.5863896772611));
#33676=CARTESIAN_POINT('Ctrl Pts',(208.501979763016,-5.21918500094195,10.7233330822924));
#33677=CARTESIAN_POINT('Ctrl Pts',(208.541470813569,-6.9924203499568,9.86027648732369));
#33678=CARTESIAN_POINT('Ctrl Pts',(208.580961864122,-8.5469998715973,8.54796981463284));
#33679=CARTESIAN_POINT('Ctrl Pts',(208.620452914674,-9.69539442575685,6.94471679745451));
#33680=CARTESIAN_POINT('Ctrl Pts',(208.659943965227,-10.8437889799164,5.34146378027619));
#33681=CARTESIAN_POINT('Ctrl Pts',(208.69943501578,-11.585998566595,3.44726441861042));
#33682=CARTESIAN_POINT('Ctrl Pts',(208.738926066333,-11.8324903419393,1.49061624027016));
#33683=CARTESIAN_POINT('Ctrl Pts',(208.748898428504,-11.894734957408,0.996519375179027));
#33684=CARTESIAN_POINT('Ctrl Pts',(208.758870790676,-11.9253689368238,0.49844031140405));
#33685=CARTESIAN_POINT('Ctrl Pts',(208.768843152848,-11.9248763938011,0.000301080366776068));
#33686=CARTESIAN_POINT('Origin',(212.6,0.,0.));
#33687=CARTESIAN_POINT('',(210.481156847152,-11.9257187659321,-0.000199934177370631));
#33688=CARTESIAN_POINT('',(210.268843152848,-11.9258152927569,-0.000165876011026085));
#33689=CARTESIAN_POINT('',(212.6,-11.925,-1.46039130798322E-15));
#33690=CARTESIAN_POINT('Ctrl Pts',(210.481156847152,-11.9257187659321,-0.000199934177370631));
#33691=CARTESIAN_POINT('Ctrl Pts',(210.445927913913,-11.9243221171086,1.75919632918402));
#33692=CARTESIAN_POINT('Ctrl Pts',(210.410698980674,-11.5299628057005,3.51919798316331));
#33693=CARTESIAN_POINT('Ctrl Pts',(210.375470047435,-10.7763254526979,5.108872047103));
#33694=CARTESIAN_POINT('Ctrl Pts',(210.335978996882,-9.93151046485828,6.8908703379858));
#33695=CARTESIAN_POINT('Ctrl Pts',(210.296487946329,-8.63522530351655,8.45883432193996));
#33696=CARTESIAN_POINT('Ctrl Pts',(210.256996895776,-7.04384102480421,9.6236202893412));
#33697=CARTESIAN_POINT('Ctrl Pts',(210.217505845224,-5.45245674609186,10.7884062567424));
#33698=CARTESIAN_POINT('Ctrl Pts',(210.178014794671,-3.56597335000889,11.5500142075908));
#33699=CARTESIAN_POINT('Ctrl Pts',(210.138523744118,-1.61195758638579,11.8165712707125));
#33700=CARTESIAN_POINT('Ctrl Pts',(210.099032693566,0.342058177237336,12.0831283338342));
#33701=CARTESIAN_POINT('Ctrl Pts',(210.059541643013,2.3636063084006,11.8546345092293));
#33702=CARTESIAN_POINT('Ctrl Pts',(210.02005059246,4.20882717982609,11.1586530381804));
#33703=CARTESIAN_POINT('Ctrl Pts',(209.980559541907,6.05404805125158,10.4626715671314));
#33704=CARTESIAN_POINT('Ctrl Pts',(209.941068491354,7.7229416629393,9.29920244963827));
#33705=CARTESIAN_POINT('Ctrl Pts',(209.901577440802,9.01418915048089,7.8085951243157));
#33706=CARTESIAN_POINT('Ctrl Pts',(209.862086390249,10.3054366380225,6.31798779899315));
#33707=CARTESIAN_POINT('Ctrl Pts',(209.822595339696,11.2190380014179,4.50024226584114));
#33708=CARTESIAN_POINT('Ctrl Pts',(209.783104289143,11.6447853833703,2.57463341689275));
#33709=CARTESIAN_POINT('Ctrl Pts',(209.743613238591,12.0705327653226,0.649024567944349));
#33710=CARTESIAN_POINT('Ctrl Pts',(209.704122188038,12.0084261658319,-1.38444759680043));
#33711=CARTESIAN_POINT('Ctrl Pts',(209.664631137485,11.4659575124806,-3.2804850522635));
#33712=CARTESIAN_POINT('Ctrl Pts',(209.625140086932,10.9234888591293,-5.17652250772661));
#33713=CARTESIAN_POINT('Ctrl Pts',(209.58564903638,9.90065815191745,-6.93512525390801));
#33714=CARTESIAN_POINT('Ctrl Pts',(209.546157985827,8.52084959881122,-8.34415280124789));
#33715=CARTESIAN_POINT('Ctrl Pts',(209.506666935274,7.14104104570499,-9.75318034858777));
#33716=CARTESIAN_POINT('Ctrl Pts',(209.467175884721,5.40425464670437,-10.8126326970861));
#33717=CARTESIAN_POINT('Ctrl Pts',(209.427684834168,3.51999918242787,-11.3947079651846));
#33718=CARTESIAN_POINT('Ctrl Pts',(209.388193783616,1.63574371815139,-11.9767832332831));
#33719=CARTESIAN_POINT('Ctrl Pts',(209.348702733063,-0.395980811400968,
-12.0814814209816));
#33720=CARTESIAN_POINT('Ctrl Pts',(209.30921168251,-2.33008719862318,-11.6961727715927));
#33721=CARTESIAN_POINT('Ctrl Pts',(209.269720631957,-4.26419358584538,-11.3108641222038));
#33722=CARTESIAN_POINT('Ctrl Pts',(209.230229581405,-6.10068183073744,-10.4355486357274));
#33723=CARTESIAN_POINT('Ctrl Pts',(209.190738530852,-7.61801610538814,-9.17581573889653));
#33724=CARTESIAN_POINT('Ctrl Pts',(209.151247480299,-9.13535038003885,-7.91608284206565));
#33725=CARTESIAN_POINT('Ctrl Pts',(209.111756429746,-10.3335306844482,-6.27193253488027));
#33726=CARTESIAN_POINT('Ctrl Pts',(209.072265379193,-11.0680203647811,-4.44169889354584));
#33727=CARTESIAN_POINT('Ctrl Pts',(209.041895868513,-11.6328595341468,-3.03420784581842));
#33728=CARTESIAN_POINT('Ctrl Pts',(209.011526357832,-11.9234740292446,-1.51666790116677));
#33729=CARTESIAN_POINT('Ctrl Pts',(208.981156847152,-11.9250072207259,0.000301374860750547));
#33730=CARTESIAN_POINT('Ctrl Pts',(208.768843152848,-11.9248763938011,0.000301080366776068));
#33731=CARTESIAN_POINT('Ctrl Pts',(208.798361841229,-11.9234184419388,-1.47421583728277));
#33732=CARTESIAN_POINT('Ctrl Pts',(208.82788052961,-11.6492331794196,-2.94925993414675));
#33733=CARTESIAN_POINT('Ctrl Pts',(208.857399217991,-11.1148764047439,-4.32311079838467));
#33734=CARTESIAN_POINT('Ctrl Pts',(208.896890268544,-10.3999967281943,-6.16109266368449));
#33735=CARTESIAN_POINT('Ctrl Pts',(208.936381319096,-9.21946341108495,-7.81795939926939));
#33736=CARTESIAN_POINT('Ctrl Pts',(208.975872369649,-7.71568434876186,-9.09384294443857));
#33737=CARTESIAN_POINT('Ctrl Pts',(209.015363420202,-6.21190528643878,-10.3697264896077));
#33738=CARTESIAN_POINT('Ctrl Pts',(209.054854470755,-4.38488047890197,-11.2646268443612));
#33739=CARTESIAN_POINT('Ctrl Pts',(209.094345521308,-2.45500417832141,-11.6705920566297));
#33740=CARTESIAN_POINT('Ctrl Pts',(209.13383657186,-0.525127877740846,-12.0765572688982));
#33741=CARTESIAN_POINT('Ctrl Pts',(209.173327622413,1.50759991588345,-11.9935873386817));
#33742=CARTESIAN_POINT('Ctrl Pts',(209.212818672966,3.39797097106338,-11.431690939999));
#33743=CARTESIAN_POINT('Ctrl Pts',(209.252309723519,5.28834202624329,-10.8697945413162));
#33744=CARTESIAN_POINT('Ctrl Pts',(209.291800774071,7.03635634297882,-9.82897167416715));
#33745=CARTESIAN_POINT('Ctrl Pts',(209.331291824624,8.43115071540099,-8.43477694322957));
#33746=CARTESIAN_POINT('Ctrl Pts',(209.370782875177,9.82594508782317,-7.04058221229198));
#33747=CARTESIAN_POINT('Ctrl Pts',(209.41027392573,10.867519515932,-5.29301561756582));
#33748=CARTESIAN_POINT('Ctrl Pts',(209.449764976283,11.4302287341484,-3.402886356153));
#33749=CARTESIAN_POINT('Ctrl Pts',(209.489256026835,11.9929379523648,-1.51275709474018));
#33750=CARTESIAN_POINT('Ctrl Pts',(209.528747077388,12.0767819606888,0.519934833359339));
#33751=CARTESIAN_POINT('Ctrl Pts',(209.568238127941,11.6716466449402,2.44998552312061));
#33752=CARTESIAN_POINT('Ctrl Pts',(209.607729178494,11.2665113291916,4.38003621288187));
#33753=CARTESIAN_POINT('Ctrl Pts',(209.647220229046,10.3723966893704,6.20744566430488));
#33754=CARTESIAN_POINT('Ctrl Pts',(209.686711279599,9.09715989664615,7.71177322557509));
#33755=CARTESIAN_POINT('Ctrl Pts',(209.726202330152,7.82192310392194,9.21610078684532));
#33756=CARTESIAN_POINT('Ctrl Pts',(209.765693380705,6.16556415829473,10.3973464579627));
#33757=CARTESIAN_POINT('Ctrl Pts',(209.805184431257,4.32788986569333,11.1130164122201));
#33758=CARTESIAN_POINT('Ctrl Pts',(209.84467548181,2.49021557309193,11.8286863664774));
#33759=CARTESIAN_POINT('Ctrl Pts',(209.884166532363,0.471225933516344,12.0787806038747));
#33760=CARTESIAN_POINT('Ctrl Pts',(209.923657582916,-1.48552805694534,11.8331302223829));
#33761=CARTESIAN_POINT('Ctrl Pts',(209.963148633469,-3.44228204740699,11.5874798408911));
#33762=CARTESIAN_POINT('Ctrl Pts',(210.002639684021,-5.33680038875474,10.8460848405102));
#33763=CARTESIAN_POINT('Ctrl Pts',(210.042130734574,-6.94054707461293,9.69837980143724));
#33764=CARTESIAN_POINT('Ctrl Pts',(210.081621785127,-8.54429376047112,8.55067476236425));
#33765=CARTESIAN_POINT('Ctrl Pts',(210.12111283568,-9.85726879083975,6.99665968459916));
#33766=CARTESIAN_POINT('Ctrl Pts',(210.160603886232,-10.7210878084062,5.22379561930672));
#33767=CARTESIAN_POINT('Ctrl Pts',(210.196683641771,-11.5102888690802,3.60407415878444));
#33768=CARTESIAN_POINT('Ctrl Pts',(210.23276339731,-11.9245799369333,1.80167970713185));
#33769=CARTESIAN_POINT('Ctrl Pts',(210.268843152848,-11.9258152927569,-0.000165876011026086));
#33770=CARTESIAN_POINT('Origin',(212.6,0.,0.));
#33771=CARTESIAN_POINT('',(211.981156847152,-11.9240555281102,-9.42862044917003E-5));
#33772=CARTESIAN_POINT('',(211.768843152848,-11.9240993487478,-0.000130385428097346));
#33773=CARTESIAN_POINT('',(212.6,-11.925,-1.46039130798322E-15));
#33774=CARTESIAN_POINT('Ctrl Pts',(211.981156847152,-11.9240555281102,-9.42862044917003E-5));
#33775=CARTESIAN_POINT('Ctrl Pts',(211.959311571099,-11.9237506840456,1.09133601012478));
#33776=CARTESIAN_POINT('Ctrl Pts',(211.937466295046,-11.7751872270301,2.18284765302012));
#33777=CARTESIAN_POINT('Ctrl Pts',(211.915621018993,-11.4794611311497,3.23291447374606));
#33778=CARTESIAN_POINT('Ctrl Pts',(211.87612996844,-10.9448588595244,5.13118491906222));
#33779=CARTESIAN_POINT('Ctrl Pts',(211.836638917888,-9.92932880492338,6.89401360690861));
#33780=CARTESIAN_POINT('Ctrl Pts',(211.797147867335,-8.55537449659076,8.30875027180494));
#33781=CARTESIAN_POINT('Ctrl Pts',(211.757656816782,-7.18142018825815,9.72348693670128));
#33782=CARTESIAN_POINT('Ctrl Pts',(211.718165766229,-5.44904162619398,10.7901315786476));
#33783=CARTESIAN_POINT('Ctrl Pts',(211.678674715676,-3.56721587304484,11.3800147087441));
#33784=CARTESIAN_POINT('Ctrl Pts',(211.639183665124,-1.68539011989571,11.9698978388406));
#33785=CARTESIAN_POINT('Ctrl Pts',(211.599692614571,0.345882824338399,12.0830194570873));
#33786=CARTESIAN_POINT('Ctrl Pts',(211.560201564018,2.28157022685008,11.7057336872187));
#33787=CARTESIAN_POINT('Ctrl Pts',(211.520710513465,4.2172576293617,11.32844791735));
#33788=CARTESIAN_POINT('Ctrl Pts',(211.481219462913,6.0573594901509,10.4607547593661));
#33789=CARTESIAN_POINT('Ctrl Pts',(211.44172841236,7.57990407032705,9.20732415747235));
#33790=CARTESIAN_POINT('Ctrl Pts',(211.402237361807,9.10244865050324,7.95389355557854));
#33791=CARTESIAN_POINT('Ctrl Pts',(211.362746311254,10.3074359500664,6.31472550977488));
#33792=CARTESIAN_POINT('Ctrl Pts',(211.323255260701,11.0495081864258,4.48755308539555));
#33793=CARTESIAN_POINT('Ctrl Pts',(211.283764210149,11.7915804227853,2.66038066101622));
#33794=CARTESIAN_POINT('Ctrl Pts',(211.244273159596,12.0707375959411,0.645203858061226));
#33795=CARTESIAN_POINT('Ctrl Pts',(211.204782109043,11.8533049379526,-1.31488627038385));
#33796=CARTESIAN_POINT('Ctrl Pts',(211.16529105849,11.6358722799641,-3.27497639882889));
#33797=CARTESIAN_POINT('Ctrl Pts',(211.125800007938,10.9218497908313,-5.17997985276401));
#33798=CARTESIAN_POINT('Ctrl Pts',(211.086308957385,9.79737010097926,-6.80009580524951));
#33799=CARTESIAN_POINT('Ctrl Pts',(211.046817906832,8.67289041112725,-8.42021175773503));
#33800=CARTESIAN_POINT('Ctrl Pts',(211.007326856279,7.137953520556,-9.75544020877092));
#33801=CARTESIAN_POINT('Ctrl Pts',(210.967835805727,5.37771907610233,-10.6447123678688));
#33802=CARTESIAN_POINT('Ctrl Pts',(210.928344755174,3.61748463164866,-11.5339845269667));
#33803=CARTESIAN_POINT('Ctrl Pts',(210.888853704621,1.63195263331257,-11.9773003941266));
#33804=CARTESIAN_POINT('Ctrl Pts',(210.849362654068,-0.339361922652062,
-11.9211827157203));
#33805=CARTESIAN_POINT('Ctrl Pts',(210.809871603515,-2.31067647861667,-11.8650650373139));
#33806=CARTESIAN_POINT('Ctrl Pts',(210.770380552962,-4.26777359220982,-11.3095138133413));
#33807=CARTESIAN_POINT('Ctrl Pts',(210.73088950241,-5.97456837120942,-10.3215452638584));
#33808=CARTESIAN_POINT('Ctrl Pts',(210.691398451857,-7.68136315020902,-9.33357671437552));
#33809=CARTESIAN_POINT('Ctrl Pts',(210.651907401304,-9.13785559461506,-7.91319083938231));
#33810=CARTESIAN_POINT('Ctrl Pts',(210.612416350752,-10.16834882185,-6.23172898105467));
#33811=CARTESIAN_POINT('Ctrl Pts',(210.572925300199,-11.1988420490849,-4.55026712272701));
#33812=CARTESIAN_POINT('Ctrl Pts',(210.533434249646,-11.8033360591487,-2.6077292810649));
#33813=CARTESIAN_POINT('Ctrl Pts',(210.493943199093,-11.9089106570118,-0.638444061328108));
#33814=CARTESIAN_POINT('Ctrl Pts',(210.489681081779,-11.9203049176139,-0.42590667593657));
#33815=CARTESIAN_POINT('Ctrl Pts',(210.485418964466,-11.9258877373027,-0.213057735605563));
#33816=CARTESIAN_POINT('Ctrl Pts',(210.481156847152,-11.9257187659321,-0.000199934177370631));
#33817=CARTESIAN_POINT('Ctrl Pts',(210.268843152848,-11.9258152927569,-0.000165876011026086));
#33818=CARTESIAN_POINT('Ctrl Pts',(210.272254447862,-11.9259320940794,-0.17052808502141));
#33819=CARTESIAN_POINT('Ctrl Pts',(210.275665742877,-11.9223563995277,-0.340885387442564));
#33820=CARTESIAN_POINT('Ctrl Pts',(210.279077037891,-11.9150559677764,-0.511082921451824));
#33821=CARTESIAN_POINT('Ctrl Pts',(210.318568088444,-11.830542104816,-2.48138434409818));
#33822=CARTESIAN_POINT('Ctrl Pts',(210.358059138996,-11.2468513741308,-4.43027413657111));
#33823=CARTESIAN_POINT('Ctrl Pts',(210.397550189549,-10.2343944683165,-6.12265745691662));
#33824=CARTESIAN_POINT('Ctrl Pts',(210.437041240102,-9.22193756250219,-7.81504077726213));
#33825=CARTESIAN_POINT('Ctrl Pts',(210.476532290655,-7.78071448155873,-9.25091762548023));
#33826=CARTESIAN_POINT('Ctrl Pts',(210.516023341207,-6.08458016266289,-10.2570779811783));
#33827=CARTESIAN_POINT('Ctrl Pts',(210.55551439176,-4.38844584376707,-11.2632383368764));
#33828=CARTESIAN_POINT('Ctrl Pts',(210.595005442313,-2.43740028691886,-11.8396822000545));
#33829=CARTESIAN_POINT('Ctrl Pts',(210.634496492866,-0.466798384223374,
-11.9168730687345));
#33830=CARTESIAN_POINT('Ctrl Pts',(210.673987543418,1.50380351847213,-11.9940639374146));
#33831=CARTESIAN_POINT('Ctrl Pts',(210.713478593971,3.49396176701487,-11.5720018115967));
#33832=CARTESIAN_POINT('Ctrl Pts',(210.752969644524,5.26360329995653,-10.7016001031869));
#33833=CARTESIAN_POINT('Ctrl Pts',(210.792460695077,7.0332448328982,-9.83119839477717));
#33834=CARTESIAN_POINT('Ctrl Pts',(210.831951745629,8.58236965023875,-8.51245710377558));
#33835=CARTESIAN_POINT('Ctrl Pts',(210.871442796182,9.72410661359659,-6.90445617230285));
#33836=CARTESIAN_POINT('Ctrl Pts',(210.910933846735,10.8658435769544,-5.29645524083012));
#33837=CARTESIAN_POINT('Ctrl Pts',(210.950424897288,11.6001926863296,-3.39919466888623));
#33838=CARTESIAN_POINT('Ctrl Pts',(210.989915947841,11.8385693083198,-1.44154125849834));
#33839=CARTESIAN_POINT('Ctrl Pts',(211.029406998393,12.07694593031,0.516112151889512));
#33840=CARTESIAN_POINT('Ctrl Pts',(211.068898048946,11.8193500649152,2.53415840072137));
#33841=CARTESIAN_POINT('Ctrl Pts',(211.108389099499,11.0968555365749,4.36916029326344));
#33842=CARTESIAN_POINT('Ctrl Pts',(211.147880150052,10.3743610082346,6.20416218580552));
#33843=CARTESIAN_POINT('Ctrl Pts',(211.187371200604,9.18696781694879,7.85611972205781));
#33844=CARTESIAN_POINT('Ctrl Pts',(211.226862251157,7.67791136562249,9.12575703870582));
#33845=CARTESIAN_POINT('Ctrl Pts',(211.26635330171,6.16885491429619,10.3953943553538));
#33846=CARTESIAN_POINT('Ctrl Pts',(211.305844352263,4.33813520292946,11.2827114523975));
#33847=CARTESIAN_POINT('Ctrl Pts',(211.345335402816,2.40659220044616,11.6806711471814));
#33848=CARTESIAN_POINT('Ctrl Pts',(211.384826453368,0.475049197962844,12.0786308419652));
#33849=CARTESIAN_POINT('Ctrl Pts',(211.424317503921,-1.55731709563709,11.9872331344892));
#33850=CARTESIAN_POINT('Ctrl Pts',(211.463808554474,-3.44534205666278,11.4175033426943));
#33851=CARTESIAN_POINT('Ctrl Pts',(211.503299605027,-5.3333670176885,10.8477735508993));
#33852=CARTESIAN_POINT('Ctrl Pts',(211.542790655579,-7.07705064613995,9.79971167478558));
#33853=CARTESIAN_POINT('Ctrl Pts',(211.582281706132,-8.46605214766769,8.3997455616712));
#33854=CARTESIAN_POINT('Ctrl Pts',(211.621772756685,-9.85505364919538,6.99977944855687));
#33855=CARTESIAN_POINT('Ctrl Pts',(211.661263807238,-10.8893730237993,5.24790909844197));
#33856=CARTESIAN_POINT('Ctrl Pts',(211.700754857791,-11.4442401839961,3.35546287102892));
#33857=CARTESIAN_POINT('Ctrl Pts',(211.723450956143,-11.7631306532074,2.26784567414334));
#33858=CARTESIAN_POINT('Ctrl Pts',(211.746147054496,-11.9236593462382,1.13379664328528));
#33859=CARTESIAN_POINT('Ctrl Pts',(211.768843152848,-11.9240993487478,-0.000130385428097346));
#33860=CARTESIAN_POINT('Origin',(212.6,0.,0.));
#33861=CARTESIAN_POINT('',(213.481156847152,-11.9251100366554,0.000297839544098621));
#33862=CARTESIAN_POINT('',(213.268843152848,-11.9249776593072,0.000301781866272833));
#33863=CARTESIAN_POINT('',(212.6,-11.925,-1.46039130798322E-15));
#33864=CARTESIAN_POINT('Ctrl Pts',(213.481156847152,-11.9251100366554,0.000297839544098621));
#33865=CARTESIAN_POINT('Ctrl Pts',(213.472695228285,-11.925539783909,0.422948611961856));
#33866=CARTESIAN_POINT('Ctrl Pts',(213.464233609418,-11.9035018557077,0.84555479724396));
#33867=CARTESIAN_POINT('Ctrl Pts',(213.455771990551,-11.8586550796965,1.26572649372693));
#33868=CARTESIAN_POINT('Ctrl Pts',(213.416280939998,-11.649351596942,3.22670133407911));
#33869=CARTESIAN_POINT('Ctrl Pts',(213.376789889446,-10.9432341408314,5.13464903060221));
#33870=CARTESIAN_POINT('Ctrl Pts',(213.337298838893,-9.82548175657631,6.75941359197088));
#33871=CARTESIAN_POINT('Ctrl Pts',(213.29780778834,-8.70772937232116,8.38417815333963));
#33872=CARTESIAN_POINT('Ctrl Pts',(213.258316737787,-7.17834205992146,9.72575957955392));
#33873=CARTESIAN_POINT('Ctrl Pts',(213.218825687234,-5.4218100198409,10.6223227198616));
#33874=CARTESIAN_POINT('Ctrl Pts',(213.179334636682,-3.66527797976036,11.5188858601692));
#33875=CARTESIAN_POINT('Ctrl Pts',(213.139843586129,-1.68160121199899,11.9704307145702));
#33876=CARTESIAN_POINT('Ctrl Pts',(213.100352535576,0.289929083907081,11.922487365581));
#33877=CARTESIAN_POINT('Ctrl Pts',(213.060861485023,2.26145937981309,11.8745440165919));
#33878=CARTESIAN_POINT('Ctrl Pts',(213.021370434471,4.22084320386379,11.3271124642125));
#33879=CARTESIAN_POINT('Ctrl Pts',(212.981879383918,5.93171981764215,10.3462294514053));
#33880=CARTESIAN_POINT('Ctrl Pts',(212.942388333365,7.64259643142056,9.36534643859798));
#33881=CARTESIAN_POINT('Ctrl Pts',(212.902897282812,9.1049658349266,7.95101196536274));
#33882=CARTESIAN_POINT('Ctrl Pts',(212.86340623226,10.1424222072035,6.27383739245451));
#33883=CARTESIAN_POINT('Ctrl Pts',(212.823915181707,11.1798785794803,4.59666281954626));
#33884=CARTESIAN_POINT('Ctrl Pts',(212.784424131154,11.792421920528,2.65664814696501));
#33885=CARTESIAN_POINT('Ctrl Pts',(212.744933080601,11.9061610434206,0.687817609739553));
#33886=CARTESIAN_POINT('Ctrl Pts',(212.705442030048,12.0199001663132,-1.28101292748585));
#33887=CARTESIAN_POINT('Ctrl Pts',(212.665950979496,11.6348350710507,-3.27865932935547));
#33888=CARTESIAN_POINT('Ctrl Pts',(212.626459928943,10.7974162126884,-5.06414523746193));
#33889=CARTESIAN_POINT('Ctrl Pts',(212.58696887839,9.95999735432603,-6.84963114556838));
#33890=CARTESIAN_POINT('Ctrl Pts',(212.547477827837,8.67022473286378,-8.42295655991168));
#33891=CARTESIAN_POINT('Ctrl Pts',(212.507986777285,7.08368379585762,-9.59433102078714));
#33892=CARTESIAN_POINT('Ctrl Pts',(212.468495726732,5.49714285885149,-10.7657054816626));
#33893=CARTESIAN_POINT('Ctrl Pts',(212.429004676179,3.61383360630147,-11.5351289890702));
#33894=CARTESIAN_POINT('Ctrl Pts',(212.389513625626,1.66093989066995,-11.8097858801807));
#33895=CARTESIAN_POINT('Ctrl Pts',(212.350022575074,-0.291953824961641,
-12.0844427712912));
#33896=CARTESIAN_POINT('Ctrl Pts',(212.310531524521,-2.31443200367473,-11.8643330461045));
#33897=CARTESIAN_POINT('Ctrl Pts',(212.271040473968,-4.16252282642839,-11.1760085708448));
#33898=CARTESIAN_POINT('Ctrl Pts',(212.231549423415,-6.01061364918205,-10.4876840955851));
#33899=CARTESIAN_POINT('Ctrl Pts',(212.192058372862,-7.68431711597629,-9.33114487025232));
#33900=CARTESIAN_POINT('Ctrl Pts',(212.15256732231,-8.98173414892402,-7.84590437962295));
#33901=CARTESIAN_POINT('Ctrl Pts',(212.113076271757,-10.2791511818717,-6.36066388899365));
#33902=CARTESIAN_POINT('Ctrl Pts',(212.073585221204,-11.2002817809729,-4.54672213306777));
#33903=CARTESIAN_POINT('Ctrl Pts',(212.034094170651,-11.6340098361987,-2.6228951537119));
#33904=CARTESIAN_POINT('Ctrl Pts',(212.016448396151,-11.8278124155081,-1.7632721105357));
#33905=CARTESIAN_POINT('Ctrl Pts',(211.998802621652,-11.9243017694307,-0.881709736823186));
#33906=CARTESIAN_POINT('Ctrl Pts',(211.981156847152,-11.9240555281102,-9.42862044917003E-5));
#33907=CARTESIAN_POINT('Ctrl Pts',(211.768843152848,-11.9240993487478,-0.000130385428097346));
#33908=CARTESIAN_POINT('Ctrl Pts',(211.785638105048,-11.9244249474918,-0.839228363854304));
#33909=CARTESIAN_POINT('Ctrl Pts',(211.802433057249,-11.8370876556473,-1.67825953518361));
#33910=CARTESIAN_POINT('Ctrl Pts',(211.819228009449,-11.6613877061497,-2.49835970882992));
#33911=CARTESIAN_POINT('Ctrl Pts',(211.858719060002,-11.248253122317,-4.42671395656453));
#33912=CARTESIAN_POINT('Ctrl Pts',(211.898210110554,-10.3465690088622,-6.25040034732254));
#33913=CARTESIAN_POINT('Ctrl Pts',(211.937701161107,-9.06510564359358,-7.74942734260614));
#33914=CARTESIAN_POINT('Ctrl Pts',(211.97719221166,-7.78364227832489,-9.24845433788976));
#33915=CARTESIAN_POINT('Ctrl Pts',(212.016683262213,-6.12239966124234,-10.4228219376989));
#33916=CARTESIAN_POINT('Ctrl Pts',(212.056174312765,-4.28177371622964,-11.1308660180082));
#33917=CARTESIAN_POINT('Ctrl Pts',(212.095665363318,-2.44114777121695,-11.8389100983174));
#33918=CARTESIAN_POINT('Ctrl Pts',(212.135156413871,-0.421138498274144,
-12.0806306591266));
#33919=CARTESIAN_POINT('Ctrl Pts',(212.174647464424,1.5345801079983,-11.8268689161578));
#33920=CARTESIAN_POINT('Ctrl Pts',(212.214138514977,3.49029871427071,-11.573107173189));
#33921=CARTESIAN_POINT('Ctrl Pts',(212.253629565529,5.38172665387273,-10.8238631264422));
#33922=CARTESIAN_POINT('Ctrl Pts',(212.293120616082,6.98070071601359,-9.66951818764984));
#33923=CARTESIAN_POINT('Ctrl Pts',(212.332611666635,8.57967477815445,-8.51517324885752));
#33924=CARTESIAN_POINT('Ctrl Pts',(212.372102717188,9.88619496283413,-6.95572741801974));
#33925=CARTESIAN_POINT('Ctrl Pts',(212.41159376774,10.7426555616574,-5.17929685878644));
#33926=CARTESIAN_POINT('Ctrl Pts',(212.451084818293,11.5991161604807,-3.40286629955314));
#33927=CARTESIAN_POINT('Ctrl Pts',(212.490575868846,12.0055171734476,-1.40945101192424));
#33928=CARTESIAN_POINT('Ctrl Pts',(212.530066919399,11.9128343908349,0.560483045581709));
#33929=CARTESIAN_POINT('Ctrl Pts',(212.569557969951,11.8201516082223,2.53041710308769));
#33930=CARTESIAN_POINT('Ctrl Pts',(212.609049020504,11.2283850300301,4.47686993047078));
#33931=CARTESIAN_POINT('Ctrl Pts',(212.648540071057,10.2089195394423,6.16504065720881));
#33932=CARTESIAN_POINT('Ctrl Pts',(212.68803112161,9.18945404885441,7.85321138394682));
#33933=CARTESIAN_POINT('Ctrl Pts',(212.727522172163,7.74228964587083,9.28310001003975));
#33934=CARTESIAN_POINT('Ctrl Pts',(212.767013222715,6.04199797015777,10.2822188751482));
#33935=CARTESIAN_POINT('Ctrl Pts',(212.806504273268,4.34170629444471,11.2813377402566));
#33936=CARTESIAN_POINT('Ctrl Pts',(212.845995323821,2.38828734600218,11.8496868443805));
#33937=CARTESIAN_POINT('Ctrl Pts',(212.885486374374,0.417382319487588,11.9187061574327));
#33938=CARTESIAN_POINT('Ctrl Pts',(212.924977424926,-1.55352270702703,11.9877254704848));
#33939=CARTESIAN_POINT('Ctrl Pts',(212.964468475479,-3.5419138116137,11.5574149924652));
#33940=CARTESIAN_POINT('Ctrl Pts',(213.003959526032,-5.3079311036409,10.679683135133));
#33941=CARTESIAN_POINT('Ctrl Pts',(213.043450576585,-7.07394839566808,9.80195127780094));
#33942=CARTESIAN_POINT('Ctrl Pts',(213.082941627138,-8.61759187513578,8.47679804115636));
#33943=CARTESIAN_POINT('Ctrl Pts',(213.12243267769,-9.75265161819899,6.86407684119899));
#33944=CARTESIAN_POINT('Ctrl Pts',(213.161923728243,-10.8877113612622,5.2513556412416));
#33945=CARTESIAN_POINT('Ctrl Pts',(213.201414778796,-11.614187367921,3.35106647797142));
#33946=CARTESIAN_POINT('Ctrl Pts',(213.240905829349,-11.8444447382294,1.3924414928011));
#33947=CARTESIAN_POINT('Ctrl Pts',(213.250218270515,-11.8987420583598,0.930575331067063));
#33948=CARTESIAN_POINT('Ctrl Pts',(213.259530711682,-11.9254461332588,0.465465287460084));
#33949=CARTESIAN_POINT('Ctrl Pts',(213.268843152848,-11.9249776593072,0.000301781866272833));
#33950=CARTESIAN_POINT('Origin',(212.6,0.,0.));
#33951=CARTESIAN_POINT('',(214.981156847152,-11.9256350387103,-0.000223418725388003));
#33952=CARTESIAN_POINT('',(214.768843152848,-11.92574165171,-0.000192647346739548));
#33953=CARTESIAN_POINT('',(212.6,-11.925,-1.46039130798322E-15));
#33954=CARTESIAN_POINT('Ctrl Pts',(214.981156847152,-11.9256350387103,-0.000223418725388003));
#33955=CARTESIAN_POINT('Ctrl Pts',(214.946587834918,-11.9241468048938,1.72625030866615));
#33956=CARTESIAN_POINT('Ctrl Pts',(214.912018822685,-11.5448800822796,3.45335664987414));
#33957=CARTESIAN_POINT('Ctrl Pts',(214.877449810451,-10.8183213363969,5.01933136170478));
#33958=CARTESIAN_POINT('Ctrl Pts',(214.837958759898,-9.98831300496768,6.80827418978669));
#33959=CARTESIAN_POINT('Ctrl Pts',(214.798467709345,-8.70507509800421,8.38693398487368));
#33960=CARTESIAN_POINT('Ctrl Pts',(214.758976658793,-7.12340477955964,9.56487680018312));
#33961=CARTESIAN_POINT('Ctrl Pts',(214.71948560824,-5.54173446111503,10.7428196154926));
#33962=CARTESIAN_POINT('Ctrl Pts',(214.679994557687,-3.66163173118932,11.5200454510245));
#33963=CARTESIAN_POINT('Ctrl Pts',(214.640503507134,-1.70989363898263,11.8027974480418));
#33964=CARTESIAN_POINT('Ctrl Pts',(214.601012456582,0.241844453224007,12.085549445059));
#33965=CARTESIAN_POINT('Ctrl Pts',(214.561521406029,2.26521790771161,11.8738276035617));
#33966=CARTESIAN_POINT('Ctrl Pts',(214.522030355476,4.11614690820027,11.1931719582184));
#33967=CARTESIAN_POINT('Ctrl Pts',(214.482539304923,5.96707590868894,10.5125163128752));
#33968=CARTESIAN_POINT('Ctrl Pts',(214.44304825437,7.64556045517865,9.36292686368587));
#33969=CARTESIAN_POINT('Ctrl Pts',(214.403557203818,8.94912472748544,7.88307874298126));
#33970=CARTESIAN_POINT('Ctrl Pts',(214.364066153265,10.2526889997922,6.40323062227666));
#33971=CARTESIAN_POINT('Ctrl Pts',(214.324575102712,11.1813329979161,4.59312383005675));
#33972=CARTESIAN_POINT('Ctrl Pts',(214.285084052159,11.6230342694774,2.67111179599225));
#33973=CARTESIAN_POINT('Ctrl Pts',(214.245593001607,12.0647355410387,0.749099761927715));
#33974=CARTESIAN_POINT('Ctrl Pts',(214.206101951054,12.0194940860374,-1.28481751398142));
#33975=CARTESIAN_POINT('Ctrl Pts',(214.166610900501,11.492767387372,-3.18528831283648));
#33976=CARTESIAN_POINT('Ctrl Pts',(214.127119849948,10.9660406887066,-5.08575911169154));
#33977=CARTESIAN_POINT('Ctrl Pts',(214.087628799396,9.95782874637702,-6.85278343349253));
#33978=CARTESIAN_POINT('Ctrl Pts',(214.048137748843,8.58975230474426,-8.27320489286197));
#33979=CARTESIAN_POINT('Ctrl Pts',(214.00864669829,7.22167586311151,-9.69362635223138));
#33980=CARTESIAN_POINT('Ctrl Pts',(213.969155647737,5.49373492217559,-10.7674449491692));
#33981=CARTESIAN_POINT('Ctrl Pts',(213.929664597184,3.61437123374004,-11.365125799605));
#33982=CARTESIAN_POINT('Ctrl Pts',(213.890173546632,1.73500754530452,-11.9628066500407));
#33983=CARTESIAN_POINT('Ctrl Pts',(213.850682496079,-0.295778890630705,
-12.0843497539743));
#33984=CARTESIAN_POINT('Ctrl Pts',(213.811191445526,-2.23301402882067,-11.7150933501712));
#33985=CARTESIAN_POINT('Ctrl Pts',(213.771700394973,-4.17024916701075,-11.345836946368));
#33986=CARTESIAN_POINT('Ctrl Pts',(213.732209344421,-6.01393300745556,-10.485781034828));
#33987=CARTESIAN_POINT('Ctrl Pts',(213.692718293868,-7.54166171656932,-9.23867427767465));
#33988=CARTESIAN_POINT('Ctrl Pts',(213.653227243315,-9.06939042568303,-7.99156752052131));
#33989=CARTESIAN_POINT('Ctrl Pts',(213.613736192762,-10.2811640034656,-6.35740991775461));
#33990=CARTESIAN_POINT('Ctrl Pts',(213.57424514221,-11.0308060376576,-4.5333301242806));
#33991=CARTESIAN_POINT('Ctrl Pts',(213.543215710524,-11.61982471311,-3.10008997115947));
#33992=CARTESIAN_POINT('Ctrl Pts',(213.512186278838,-11.9235341191794,-1.54959627362695));
#33993=CARTESIAN_POINT('Ctrl Pts',(213.481156847152,-11.9251100366554,0.000297839544098621));
#33994=CARTESIAN_POINT('Ctrl Pts',(213.268843152848,-11.9249776593072,0.000301781866272833));
#33995=CARTESIAN_POINT('Ctrl Pts',(213.299021762234,-11.9234594867745,-1.50714266637844));
#33996=CARTESIAN_POINT('Ctrl Pts',(213.329200371621,-11.6365756334932,-3.01514857156817));
#33997=CARTESIAN_POINT('Ctrl Pts',(213.359378981007,-11.0786438839662,-4.41513467066438));
#33998=CARTESIAN_POINT('Ctrl Pts',(213.39887003156,-10.3485469254364,-6.24712504188916));
#33999=CARTESIAN_POINT('Ctrl Pts',(213.438361082112,-9.15431427441883,-7.89414497726828));
#34000=CARTESIAN_POINT('Ctrl Pts',(213.477852132665,-7.64000637878046,-9.15751423695523));
#34001=CARTESIAN_POINT('Ctrl Pts',(213.517343183218,-6.12569848314209,-10.4208834966422));
#34002=CARTESIAN_POINT('Ctrl Pts',(213.556834233771,-4.29131534288294,-11.3006020806369));
#34003=CARTESIAN_POINT('Ctrl Pts',(213.596325284324,-2.35813884685473,-11.6905494159513));
#34004=CARTESIAN_POINT('Ctrl Pts',(213.635816334876,-0.424962350826485,
-12.0804967512656));
#34005=CARTESIAN_POINT('Ctrl Pts',(213.675307385429,1.60700750097082,-11.9806728378995));
#34006=CARTESIAN_POINT('Ctrl Pts',(213.714798435982,3.49265390767523,-11.4031194481618));
#34007=CARTESIAN_POINT('Ctrl Pts',(213.754289486535,5.37830031437964,-10.825566058424));
#34008=CARTESIAN_POINT('Ctrl Pts',(213.793780537087,7.11762327599115,-9.77028319231473));
#34009=CARTESIAN_POINT('Ctrl Pts',(213.83327158764,8.50080802599692,-8.36456976616193));
#34010=CARTESIAN_POINT('Ctrl Pts',(213.872762638193,9.88399277600267,-6.95885634000915));
#34011=CARTESIAN_POINT('Ctrl Pts',(213.912253688746,10.9110393144027,-5.20271235381288));
#34012=CARTESIAN_POINT('Ctrl Pts',(213.951744739298,11.4580548769386,-3.30798169657998));
#34013=CARTESIAN_POINT('Ctrl Pts',(213.991235789851,12.0050704394744,-1.41325103934708));
#34014=CARTESIAN_POINT('Ctrl Pts',(214.030726840404,12.0720550261461,0.620066288922465));
#34015=CARTESIAN_POINT('Ctrl Pts',(214.070217890957,11.650928277111,2.54669094109573));
#34016=CARTESIAN_POINT('Ctrl Pts',(214.10970894151,11.2298015280759,4.473315593269));
#34017=CARTESIAN_POINT('Ctrl Pts',(214.149199992062,10.3205634433338,6.29324756934605));
#34018=CARTESIAN_POINT('Ctrl Pts',(214.188691042615,9.03289553728178,7.78694822638488));
#34019=CARTESIAN_POINT('Ctrl Pts',(214.228182093168,7.74522763122972,9.28064888342373));
#34020=CARTESIAN_POINT('Ctrl Pts',(214.267673143721,6.07912990386763,10.4481182214244));
#34021=CARTESIAN_POINT('Ctrl Pts',(214.307164194273,4.23558395169564,11.1485242546259));
#34022=CARTESIAN_POINT('Ctrl Pts',(214.346655244826,2.39203799952365,11.8489302878274));
#34023=CARTESIAN_POINT('Ctrl Pts',(214.386146295379,0.371043822541859,12.0822730162297));
#34024=CARTESIAN_POINT('Ctrl Pts',(214.425637345932,-1.5836057755406,11.8204042746227));
#34025=CARTESIAN_POINT('Ctrl Pts',(214.465128396485,-3.53825537362304,11.5585355330157));
#34026=CARTESIAN_POINT('Ctrl Pts',(214.504619447037,-5.42656039280606,10.8014553213994));
#34027=CARTESIAN_POINT('Ctrl Pts',(214.54411049759,-7.02073434061572,9.64049032914524));
#34028=CARTESIAN_POINT('Ctrl Pts',(214.583601548143,-8.6149082884254,8.47952533689109));
#34029=CARTESIAN_POINT('Ctrl Pts',(214.623092598696,-9.9149511648617,6.9146755639991));
#34030=CARTESIAN_POINT('Ctrl Pts',(214.662583649248,-10.7640386201078,5.13470905238759));
#34031=CARTESIAN_POINT('Ctrl Pts',(214.698003483782,-11.5255918517417,3.53824305734485));
#34032=CARTESIAN_POINT('Ctrl Pts',(214.733423318315,-11.9243768133226,1.76872774634368));
#34033=CARTESIAN_POINT('Ctrl Pts',(214.768843152848,-11.92574165171,-0.000192647346739548));
#34034=CARTESIAN_POINT('Origin',(212.6,0.,0.));
#34035=CARTESIAN_POINT('',(216.481156847152,-11.9240315088021,-6.52149305474525E-5));
#34036=CARTESIAN_POINT('',(216.268843152848,-11.9240641358096,-0.000102538611651484));
#34037=CARTESIAN_POINT('',(212.6,-11.925,-1.46039130798322E-15));
#34038=CARTESIAN_POINT('Ctrl Pts',(216.481156847152,-11.9240315088021,-6.52149305474525E-5));
#34039=CARTESIAN_POINT('Ctrl Pts',(216.459971492104,-11.9238275369958,1.05840031273444));
#34040=CARTESIAN_POINT('Ctrl Pts',(216.438786137057,-11.7842138861413,2.11691862153893));
#34041=CARTESIAN_POINT('Ctrl Pts',(216.417600782009,-11.5058760523776,3.13760738835481));
#34042=CARTESIAN_POINT('Ctrl Pts',(216.378109731456,-10.9870339825039,5.04024586660471));
#34043=CARTESIAN_POINT('Ctrl Pts',(216.338618680904,-9.98615748628875,6.81143544251588));
#34044=CARTESIAN_POINT('Ctrl Pts',(216.299127630351,-8.62398243222592,8.23751727553837));
#34045=CARTESIAN_POINT('Ctrl Pts',(216.259636579798,-7.26180737816309,9.66359910856087));
#34046=CARTESIAN_POINT('Ctrl Pts',(216.220145529245,-5.53833376625262,10.7445731986947));
#34047=CARTESIAN_POINT('Ctrl Pts',(216.180654478692,-3.66146445378734,11.3500414937473));
#34048=CARTESIAN_POINT('Ctrl Pts',(216.14116342814,-1.7845951413221,11.9555097888));
#34049=CARTESIAN_POINT('Ctrl Pts',(216.101672377587,0.245669871697946,12.0854722887714));
#34050=CARTESIAN_POINT('Ctrl Pts',(216.062181327034,2.18441943934548,11.7242515995327));
#34051=CARTESIAN_POINT('Ctrl Pts',(216.022690276481,4.12316900699302,11.3630309102939));
#34052=CARTESIAN_POINT('Ctrl Pts',(215.983199225929,5.97040312926806,10.5106270318449));
#34053=CARTESIAN_POINT('Ctrl Pts',(215.943708175376,7.50328970160239,9.26986556051175));
#34054=CARTESIAN_POINT('Ctrl Pts',(215.904217124823,9.03617627393673,8.02910408917863));
#34055=CARTESIAN_POINT('Ctrl Pts',(215.86472607427,10.2547152963304,6.39998502496138));
#34056=CARTESIAN_POINT('Ctrl Pts',(215.825235023717,11.011914240016,4.57902922317239));
#34057=CARTESIAN_POINT('Ctrl Pts',(215.785743973165,11.7691131837017,2.7580734213834));
#34058=CARTESIAN_POINT('Ctrl Pts',(215.746252922612,12.0649720486793,0.745280882022666));
#34059=CARTESIAN_POINT('Ctrl Pts',(215.706761872059,11.8638013396419,-1.21654495586739));
#34060=CARTESIAN_POINT('Ctrl Pts',(215.667270821506,11.6626306306044,-3.17837079375747));
#34061=CARTESIAN_POINT('Ctrl Pts',(215.627779770954,10.9644303475518,-5.08922993017687));
#34062=CARTESIAN_POINT('Ctrl Pts',(215.588288720401,9.85342448602773,-6.7186151664077));
#34063=CARTESIAN_POINT('Ctrl Pts',(215.548797669848,8.7424186245037,-8.34800040263853));
#34064=CARTESIAN_POINT('Ctrl Pts',(215.509306619295,7.21860718450825,-9.6959117386808));
#34065=CARTESIAN_POINT('Ctrl Pts',(215.469815568742,5.46580774825511,-10.5997504458949));
#34066=CARTESIAN_POINT('Ctrl Pts',(215.43032451819,3.713008312002,-11.503589153109));
#34067=CARTESIAN_POINT('Ctrl Pts',(215.390833467637,1.73122087949119,-11.9633552314949));
#34068=CARTESIAN_POINT('Ctrl Pts',(215.351342417084,-0.240491260510576,
-11.9235870361965));
#34069=CARTESIAN_POINT('Ctrl Pts',(215.311851366531,-2.21220340051235,-11.8838188408981));
#34070=CARTESIAN_POINT('Ctrl Pts',(215.272360315979,-4.17384024800508,-11.3445163719153));
#34071=CARTESIAN_POINT('Ctrl Pts',(215.232869265426,-5.88876928204609,-10.3707357597696));
#34072=CARTESIAN_POINT('Ctrl Pts',(215.193378214873,-7.60369831608712,-9.39695514762394));
#34073=CARTESIAN_POINT('Ctrl Pts',(215.15388716432,-9.07191953667642,-7.98869639231527));
#34074=CARTESIAN_POINT('Ctrl Pts',(215.114396113767,-10.1163212173628,-6.31583793991495));
#34075=CARTESIAN_POINT('Ctrl Pts',(215.074905063215,-11.1607228980492,-4.64297948751464));
#34076=CARTESIAN_POINT('Ctrl Pts',(215.035414012662,-11.7813050388328,-2.70552133802269));
#34077=CARTESIAN_POINT('Ctrl Pts',(214.995922962109,-11.903206731277,-0.737179332738295));
#34078=CARTESIAN_POINT('Ctrl Pts',(214.99100092379,-11.9184001685996,-0.491851476438355));
#34079=CARTESIAN_POINT('Ctrl Pts',(214.986078885471,-11.9258469378476,-0.246043860042586));
#34080=CARTESIAN_POINT('Ctrl Pts',(214.981156847152,-11.9256350387103,-0.000223418725388003));
#34081=CARTESIAN_POINT('Ctrl Pts',(214.768843152848,-11.92574165171,-0.000192647346739548));
#34082=CARTESIAN_POINT('Ctrl Pts',(214.772914368868,-11.9258985285555,-0.203515365788062));
#34083=CARTESIAN_POINT('Ctrl Pts',(214.776985584887,-11.920804851864,-0.406830224423079));
#34084=CARTESIAN_POINT('Ctrl Pts',(214.781056800907,-11.9104080006084,-0.609873533518392));
#34085=CARTESIAN_POINT('Ctrl Pts',(214.820547851459,-11.809557891807,-2.57940635748183));
#34086=CARTESIAN_POINT('Ctrl Pts',(214.860038902012,-11.2097256401482,-4.52338875507772));
#34087=CARTESIAN_POINT('Ctrl Pts',(214.899529952565,-10.183269092108,-6.20731786406665));
#34088=CARTESIAN_POINT('Ctrl Pts',(214.939021003118,-9.15681254406792,-7.89124697305558));
#34089=CARTESIAN_POINT('Ctrl Pts',(214.978512053671,-7.70373169964654,-9.31512279343753));
#34090=CARTESIAN_POINT('Ctrl Pts',(215.018003104223,-5.99931189964917,-10.3071829904476));
#34091=CARTESIAN_POINT('Ctrl Pts',(215.057494154776,-4.2948920996518,-11.2992431874576));
#34092=CARTESIAN_POINT('Ctrl Pts',(215.096985205329,-2.33913334407844,-11.8594877610957));
#34093=CARTESIAN_POINT('Ctrl Pts',(215.136476255882,-0.367959078840414,
-11.9203343318945));
#34094=CARTESIAN_POINT('Ctrl Pts',(215.175967306434,1.60321518639762,-11.9811809026933));
#34095=CARTESIAN_POINT('Ctrl Pts',(215.215458356987,3.58980496130032,-11.5426294706528));
#34096=CARTESIAN_POINT('Ctrl Pts',(215.25494940754,5.35216764988208,-10.6575825549418));
#34097=CARTESIAN_POINT('Ctrl Pts',(215.294440458093,7.11453033846384,-9.7725356392308));
#34098=CARTESIAN_POINT('Ctrl Pts',(215.333931508646,8.65266594072465,-8.44099323984933));
#34099=CARTESIAN_POINT('Ctrl Pts',(215.373422559198,9.78102894879953,-6.82357949837102));
#34100=CARTESIAN_POINT('Ctrl Pts',(215.412913609751,10.9093919568744,-5.20616575689267));
#34101=CARTESIAN_POINT('Ctrl Pts',(215.452404660304,11.6279823707634,-3.30288067331745));
#34102=CARTESIAN_POINT('Ctrl Pts',(215.491895710857,11.8501165306539,-1.34331778733379));
#34103=CARTESIAN_POINT('Ctrl Pts',(215.531386761409,12.0722506905443,0.616245098649828));
#34104=CARTESIAN_POINT('Ctrl Pts',(215.570877811962,11.7979285964363,2.63208578704189));
#34105=CARTESIAN_POINT('Ctrl Pts',(215.610368862515,11.0602417600243,4.46103314016583));
#34106=CARTESIAN_POINT('Ctrl Pts',(215.649859913068,10.3225549236123,6.28998049328975));
#34107=CARTESIAN_POINT('Ctrl Pts',(215.68935096362,9.12150334489629,7.93203451114556));
#34108=CARTESIAN_POINT('Ctrl Pts',(215.728842014173,7.60197003992331,9.18911399319609));
#34109=CARTESIAN_POINT('Ctrl Pts',(215.768333064726,6.08243673495028,10.4461934752467));
#34110=CARTESIAN_POINT('Ctrl Pts',(215.807824115279,4.2444217037202,11.318298421492));
#34111=CARTESIAN_POINT('Ctrl Pts',(215.847315165832,2.30964495058899,11.7002266931057));
#34112=CARTESIAN_POINT('Ctrl Pts',(215.886806216384,0.374868197457755,12.0821549647194));
#34113=CARTESIAN_POINT('Ctrl Pts',(215.926297266937,-1.65667027757459,11.9739065617016));
#34114=CARTESIAN_POINT('Ctrl Pts',(215.96578831749,-3.53990571068435,11.3885395036988));
#34115=CARTESIAN_POINT('Ctrl Pts',(216.005279368043,-5.42314114379405,10.8031724456961));
#34116=CARTESIAN_POINT('Ctrl Pts',(216.044770418595,-7.15807353498107,9.74068673270843));
#34117=CARTESIAN_POINT('Ctrl Pts',(216.084261469148,-8.53541775284281,8.3292501614671));
#34118=CARTESIAN_POINT('Ctrl Pts',(216.123752519701,-9.91276197070455,6.91781359022576));
#34119=CARTESIAN_POINT('Ctrl Pts',(216.163243570254,-10.932518015241,5.15742616073064));
#34120=CARTESIAN_POINT('Ctrl Pts',(216.202734620806,-11.4716725754646,3.26044364913367));
#34121=CARTESIAN_POINT('Ctrl Pts',(216.224770798154,-11.7725231565545,2.20191918688213));
#34122=CARTESIAN_POINT('Ctrl Pts',(216.246806975501,-11.9237294127371,1.10086327286869));
#34123=CARTESIAN_POINT('Ctrl Pts',(216.268843152848,-11.9240641358096,-0.000102538611651484));
#34124=CARTESIAN_POINT('Origin',(212.6,0.,0.));
#34125=CARTESIAN_POINT('',(217.981156847152,-11.9252129121757,0.000290991664972789));
#34126=CARTESIAN_POINT('',(217.768843152848,-11.9250802682536,0.000299202489012452));
#34127=CARTESIAN_POINT('',(212.6,-11.925,-1.46039130798322E-15));
#34128=CARTESIAN_POINT('Ctrl Pts',(217.981156847152,-11.9252129121757,0.000290991664972789));
#34129=CARTESIAN_POINT('Ctrl Pts',(217.97335514929,-11.9256075493655,0.389969574352947));
#34130=CARTESIAN_POINT('Ctrl Pts',(217.965553451429,-11.9068787673408,0.779610388074303));
#34131=CARTESIAN_POINT('Ctrl Pts',(217.957751753567,-11.8687436293108,1.16734250236723));
#34132=CARTESIAN_POINT('Ctrl Pts',(217.918260703014,-11.6757091526497,3.12998560879517));
#34133=CARTESIAN_POINT('Ctrl Pts',(217.878769652462,-10.9854380465733,5.04372333236306));
#34134=CARTESIAN_POINT('Ctrl Pts',(217.839278601909,-9.8811978089238,6.67770122999309));
#34135=CARTESIAN_POINT('Ctrl Pts',(217.799787551356,-8.7769575712744,8.31167912762302));
#34136=CARTESIAN_POINT('Ctrl Pts',(217.760296500803,-7.25874820205201,9.66589719931515));
#34137=CARTESIAN_POINT('Ctrl Pts',(217.720805450251,-5.50971150490726,10.5769959340461));
#34138=CARTESIAN_POINT('Ctrl Pts',(217.681314399698,-3.76067480776247,11.4880946687772));
#34139=CARTESIAN_POINT('Ctrl Pts',(217.641823349145,-1.78081078269529,11.956074066547));
#34140=CARTESIAN_POINT('Ctrl Pts',(217.602332298592,0.191049302430142,11.9244817086603));
#34141=CARTESIAN_POINT('Ctrl Pts',(217.562841248039,2.16290938755557,11.8928893507736));
#34142=CARTESIAN_POINT('Ctrl Pts',(217.523350197487,4.12676553273927,11.3617252372304));
#34143=CARTESIAN_POINT('Ctrl Pts',(217.483859146934,5.84571750285487,10.3950637676231));
#34144=CARTESIAN_POINT('Ctrl Pts',(217.444368096381,7.56466947297048,9.42840229801586));
#34145=CARTESIAN_POINT('Ctrl Pts',(217.404877045828,9.03871726801803,8.02624347234463));
#34146=CARTESIAN_POINT('Ctrl Pts',(217.365385995275,10.0900463010733,6.35772990133517));
#34147=CARTESIAN_POINT('Ctrl Pts',(217.325894944723,11.1413753341286,4.68921633032567));
#34148=CARTESIAN_POINT('Ctrl Pts',(217.28640389417,11.7699856051916,2.75434801397791));
#34149=CARTESIAN_POINT('Ctrl Pts',(217.246912843617,11.9000477713734,0.786528381665041));
#34150=CARTESIAN_POINT('Ctrl Pts',(217.207421793064,12.0301099375552,-1.18129125064785));
#34151=CARTESIAN_POINT('Ctrl Pts',(217.167930742512,11.6616239988558,-3.18206219892579));
#34152=CARTESIAN_POINT('Ctrl Pts',(217.128439691959,10.8390404644088,-4.97443119030136));
#34153=CARTESIAN_POINT('Ctrl Pts',(217.088948641406,10.0164569299618,-6.76680018167684));
#34154=CARTESIAN_POINT('Ctrl Pts',(217.049457590853,8.73977579976731,-8.35076721614989));
#34155=CARTESIAN_POINT('Ctrl Pts',(217.009966540301,7.16300329300085,-9.53525813392556));
#34156=CARTESIAN_POINT('Ctrl Pts',(216.970475489748,5.58623078623438,-10.7197490517012));
#34157=CARTESIAN_POINT('Ctrl Pts',(216.930984439195,3.70936690289596,-11.5047638527795));
#34158=CARTESIAN_POINT('Ctrl Pts',(216.891493388642,1.75881798967936,-11.7956060944453));
#34159=CARTESIAN_POINT('Ctrl Pts',(216.85200233809,-0.191730923537244,-12.0864483361111));
#34160=CARTESIAN_POINT('Ctrl Pts',(216.812511287537,-2.21596486663205,-11.8831180183643));
#34161=CARTESIAN_POINT('Ctrl Pts',(216.773020236984,-4.06970022246687,-11.210142905217));
#34162=CARTESIAN_POINT('Ctrl Pts',(216.733529186431,-5.92343557830169,-10.5371677920697));
#34163=CARTESIAN_POINT('Ctrl Pts',(216.694038135878,-7.60667234687653,-9.39454788352191));
#34164=CARTESIAN_POINT('Ctrl Pts',(216.654547085326,-8.91636144680795,-7.92011757526435));
#34165=CARTESIAN_POINT('Ctrl Pts',(216.615056034773,-10.2260505467394,-6.44568726700679));
#34166=CARTESIAN_POINT('Ctrl Pts',(216.57556498422,-11.1621919780274,-4.6394465590395));
#34167=CARTESIAN_POINT('Ctrl Pts',(216.536073933667,-11.6118588719053,-2.71928251476157));
#34168=CARTESIAN_POINT('Ctrl Pts',(216.517768238162,-11.8202976225301,-1.82920899626814));
#34169=CARTESIAN_POINT('Ctrl Pts',(216.499462542657,-11.924207755354,-0.914656809388016));
#34170=CARTESIAN_POINT('Ctrl Pts',(216.481156847152,-11.9240315088021,-6.52149305474525E-5));
#34171=CARTESIAN_POINT('Ctrl Pts',(216.268843152848,-11.9240641358096,-0.000102538611651484));
#34172=CARTESIAN_POINT('Ctrl Pts',(216.286298026054,-11.9243292702156,-0.872178413671098));
#34173=CARTESIAN_POINT('Ctrl Pts',(216.303752899259,-11.829934037933,-1.74419775627108));
#34174=CARTESIAN_POINT('Ctrl Pts',(216.321207772465,-11.6402685376495,-2.59497838897577));
#34175=CARTESIAN_POINT('Ctrl Pts',(216.360698823018,-11.2111568636999,-4.51984032178938));
#34176=CARTESIAN_POINT('Ctrl Pts',(216.40018987357,-10.2943804398899,-6.33598659371769));
#34177=CARTESIAN_POINT('Ctrl Pts',(216.439680924123,-9.00053013148815,-7.82433523182753));
#34178=CARTESIAN_POINT('Ctrl Pts',(216.479171974676,-7.70667982308639,-9.31268386993737));
#34179=CARTESIAN_POINT('Ctrl Pts',(216.518663025229,-6.03575563009282,-10.4732348742287));
#34180=CARTESIAN_POINT('Ctrl Pts',(216.558154075781,-4.18932136621622,-11.1659908184813));
#34181=CARTESIAN_POINT('Ctrl Pts',(216.597645126334,-2.34288710233966,-11.8587467627338));
#34182=CARTESIAN_POINT('Ctrl Pts',(216.637136176887,-0.320942767580052,
-12.0837076469475));
#34183=CARTESIAN_POINT('Ctrl Pts',(216.67662722744,1.63260421669074,-11.8137364089219));
#34184=CARTESIAN_POINT('Ctrl Pts',(216.716118277992,3.58615120096156,-11.5437651708964));
#34185=CARTESIAN_POINT('Ctrl Pts',(216.755609328545,5.47130083474357,-10.7788618106316));
#34186=CARTESIAN_POINT('Ctrl Pts',(216.795100379098,7.06064726013488,-9.61129672498948));
#34187=CARTESIAN_POINT('Ctrl Pts',(216.834591429651,8.64999368552619,-8.44373163934735));
#34188=CARTESIAN_POINT('Ctrl Pts',(216.874082480203,9.9435369025268,-6.87350482832784));
#34189=CARTESIAN_POINT('Ctrl Pts',(216.913573530756,10.7852366161257,-5.09003296669331));
#34190=CARTESIAN_POINT('Ctrl Pts',(216.953064581309,11.6269363297247,-3.30656110505875));
#34191=CARTESIAN_POINT('Ctrl Pts',(216.992555631862,12.0167925399219,-1.30984419280916));
#34192=CARTESIAN_POINT('Ctrl Pts',(217.032046682415,11.9077768388131,0.659253536107953));
#34193=CARTESIAN_POINT('Ctrl Pts',(217.071537732967,11.7987611377042,2.62835126502504));
#34194=CARTESIAN_POINT('Ctrl Pts',(217.11102878352,11.1908735252894,4.56982981060956));
#34195=CARTESIAN_POINT('Ctrl Pts',(217.150519834073,10.1574435673132,6.24948835063251));
#34196=CARTESIAN_POINT('Ctrl Pts',(217.190010884626,9.124013609337,7.9291468906555));
#34197=CARTESIAN_POINT('Ctrl Pts',(217.229501935179,7.66504130579948,9.34698542511683));
#34198=CARTESIAN_POINT('Ctrl Pts',(217.268992985731,5.9565226850241,10.331969897877));
#34199=CARTESIAN_POINT('Ctrl Pts',(217.308484036284,4.24800406424873,11.3169543706372));
#34200=CARTESIAN_POINT('Ctrl Pts',(217.347975086837,2.28993912623549,11.8690847816963));
#34201=CARTESIAN_POINT('Ctrl Pts',(217.38746613739,0.318529511998548,11.9217575641274));
#34202=CARTESIAN_POINT('Ctrl Pts',(217.426957187942,-1.65288010223834,11.9744303465586));
#34203=CARTESIAN_POINT('Ctrl Pts',(217.466448238495,-3.63763439269893,11.5276455003618));
#34204=CARTESIAN_POINT('Ctrl Pts',(217.505939289048,-5.39631217813664,10.6352987425807));
#34205=CARTESIAN_POINT('Ctrl Pts',(217.545430339601,-7.15498996357436,9.74295198479951));
#34206=CARTESIAN_POINT('Ctrl Pts',(217.584921390154,-8.68759124398921,8.40504331543394));
#34207=CARTESIAN_POINT('Ctrl Pts',(217.624412440706,-9.80923811751666,6.78296484007562));
#34208=CARTESIAN_POINT('Ctrl Pts',(217.663903491259,-10.9308849910441,5.16088636471731));
#34209=CARTESIAN_POINT('Ctrl Pts',(217.703394541812,-11.6415774576842,3.25463808336625));
#34210=CARTESIAN_POINT('Ctrl Pts',(217.742885592365,-11.8555845880801,1.29417098666344));
#34211=CARTESIAN_POINT('Ctrl Pts',(217.751538112526,-11.902473718262,0.864631107573521));
#34212=CARTESIAN_POINT('Ctrl Pts',(217.760190632687,-11.925519392479,0.432488445912876));
#34213=CARTESIAN_POINT('Ctrl Pts',(217.768843152848,-11.9250802682536,0.000299202489012452));
#34214=CARTESIAN_POINT('Origin',(212.6,0.,0.));
#34215=CARTESIAN_POINT('',(219.481156847152,-11.9255450374969,-0.000244099323242208));
#34216=CARTESIAN_POINT('',(219.268843152848,-11.9256599882878,-0.000216904810520898));
#34217=CARTESIAN_POINT('',(212.6,-11.925,-1.46039130798322E-15));
#34218=CARTESIAN_POINT('Ctrl Pts',(219.481156847152,-11.9255450374969,-0.000244099323242208));
#34219=CARTESIAN_POINT('Ctrl Pts',(219.447247755924,-11.9239920023089,1.69330829367419));
#34220=CARTESIAN_POINT('Ctrl Pts',(219.413338664695,-11.5594992250726,3.3875078677213));
#34221=CARTESIAN_POINT('Ctrl Pts',(219.379429573467,-10.8595732414316,4.929445496933));
#34222=CARTESIAN_POINT('Ctrl Pts',(219.339938522914,-10.0444286474036,6.72520983795926));
#34223=CARTESIAN_POINT('Ctrl Pts',(219.300447472361,-8.77432624161127,8.31445687564588));
#34224=CARTESIAN_POINT('Ctrl Pts',(219.260956421809,-7.20247865493554,9.50547553041038));
#34225=CARTESIAN_POINT('Ctrl Pts',(219.221465371256,-5.63063106825982,10.6964941851749));
#34226=CARTESIAN_POINT('Ctrl Pts',(219.181974320703,-3.75703830070067,11.4892844570173));
#34227=CARTESIAN_POINT('Ctrl Pts',(219.14248327015,-1.8077121018322,11.7882119434258));
#34228=CARTESIAN_POINT('Ctrl Pts',(219.102992219598,0.141614097036269,12.0871394298343));
#34229=CARTESIAN_POINT('Ctrl Pts',(219.063501169045,2.16667372721406,11.8922041308089));
#34230=CARTESIAN_POINT('Ctrl Pts',(219.024010118492,4.02318356787142,11.2269211198753));
#34231=CARTESIAN_POINT('Ctrl Pts',(218.984519067939,5.87969340852889,10.5616381089417));
#34232=CARTESIAN_POINT('Ctrl Pts',(218.945028017386,7.56765345966592,9.42600738609977));
#34233=CARTESIAN_POINT('Ctrl Pts',(218.905536966834,8.88344487013097,7.95702023976691));
#34234=CARTESIAN_POINT('Ctrl Pts',(218.866045916281,10.1992362805959,6.48803309343413));
#34235=CARTESIAN_POINT('Ctrl Pts',(218.826554865728,11.142859050389,4.68568952361048));
#34236=CARTESIAN_POINT('Ctrl Pts',(218.787063815175,11.6004838356406,2.76740648179358));
#34237=CARTESIAN_POINT('Ctrl Pts',(218.747572764623,12.0581086208923,0.849123439976685));
#34238=CARTESIAN_POINT('Ctrl Pts',(218.70808171407,12.0297354216026,-1.18509907383346));
#34239=CARTESIAN_POINT('Ctrl Pts',(218.668590663517,11.5187869007824,-3.08987252004248));
#34240=CARTESIAN_POINT('Ctrl Pts',(218.629099612964,11.0078383799622,-4.99464596625151));
#34241=CARTESIAN_POINT('Ctrl Pts',(218.589608562411,10.0143145376115,-6.76997034485942));
#34242=CARTESIAN_POINT('Ctrl Pts',(218.550117511859,8.65806429053415,-8.20168803340916));
#34243=CARTESIAN_POINT('Ctrl Pts',(218.510626461306,7.30181404345685,-9.63340572195891));
#34244=CARTESIAN_POINT('Ctrl Pts',(218.471135410753,5.58283739165299,-10.7215167204505));
#34245=CARTESIAN_POINT('Ctrl Pts',(218.4316443602,3.70849472352703,-11.3347620505055));
#34246=CARTESIAN_POINT('Ctrl Pts',(218.392153309648,1.83415205540107,-11.9480073805605));
#34247=CARTESIAN_POINT('Ctrl Pts',(218.352662259095,-0.195556629046985,
-12.0863870421789));
#34248=CARTESIAN_POINT('Ctrl Pts',(218.313171208542,-2.13578729389285,-11.7332082778509));
#34249=CARTESIAN_POINT('Ctrl Pts',(218.273680157989,-4.07601795873877,-11.3800295135228));
#34250=CARTESIAN_POINT('Ctrl Pts',(218.234189107437,-5.92677060398249,-10.5352923232482));
#34251=CARTESIAN_POINT('Ctrl Pts',(218.194698056884,-7.4647886851439,-9.30089746972142));
#34252=CARTESIAN_POINT('Ctrl Pts',(218.155207006331,-9.00280676630527,-8.06650261619464));
#34253=CARTESIAN_POINT('Ctrl Pts',(218.115715955778,-10.2280902833843,-6.44245009941565));
#34254=CARTESIAN_POINT('Ctrl Pts',(218.076224905225,-10.992833118301,-4.62464959638219));
#34255=CARTESIAN_POINT('Ctrl Pts',(218.044535552534,-11.6064963426142,-3.16596666805982));
#34256=CARTESIAN_POINT('Ctrl Pts',(218.012846199843,-11.9236099537796,-1.58252626966517));
#34257=CARTESIAN_POINT('Ctrl Pts',(217.981156847152,-11.9252129121757,0.000290991664972789));
#34258=CARTESIAN_POINT('Ctrl Pts',(217.768843152848,-11.9250802682536,0.000299202489012452));
#34259=CARTESIAN_POINT('Ctrl Pts',(217.79968168324,-11.9235151813752,-1.54007064004802));
#34260=CARTESIAN_POINT('Ctrl Pts',(217.830520213631,-11.6236255785851,-3.08103220501337));
#34261=CARTESIAN_POINT('Ctrl Pts',(217.861358744023,-11.0416494811308,-4.5068549126511));
#34262=CARTESIAN_POINT('Ctrl Pts',(217.900849794576,-10.2963854496338,-6.33272780320826));
#34263=CARTESIAN_POINT('Ctrl Pts',(217.940340845128,-9.08853559248812,-7.96978767226803));
#34264=CARTESIAN_POINT('Ctrl Pts',(217.979831895681,-7.56380300299659,-9.22055576414479));
#34265=CARTESIAN_POINT('Ctrl Pts',(218.019322946234,-6.03907041350506,-10.4713238560216));
#34266=CARTESIAN_POINT('Ctrl Pts',(218.058813996787,-4.19745509166771,-11.3358001707153));
#34267=CARTESIAN_POINT('Ctrl Pts',(218.098305047339,-2.26111134538818,-11.7097028122664));
#34268=CARTESIAN_POINT('Ctrl Pts',(218.137796097892,-0.324767599108595,
-12.0836054538175));
#34269=CARTESIAN_POINT('Ctrl Pts',(218.177287148445,1.70630457161319,-11.9669344222258));
#34270=CARTESIAN_POINT('Ctrl Pts',(218.216778198998,3.5870966533059,-11.3737637599735));
#34271=CARTESIAN_POINT('Ctrl Pts',(218.256269249551,5.46788873499856,-10.7805930977212));
#34272=CARTESIAN_POINT('Ctrl Pts',(218.295760300103,7.19840072766217,-9.71092280480824));
#34273=CARTESIAN_POINT('Ctrl Pts',(218.335251350656,8.56988073317214,-8.29378735482445));
#34274=CARTESIAN_POINT('Ctrl Pts',(218.374742401209,9.94136073868211,-6.87665190484067));
#34275=CARTESIAN_POINT('Ctrl Pts',(218.414233451762,10.9538087570385,-5.11205129778605));
#34276=CARTESIAN_POINT('Ctrl Pts',(218.453724502314,11.4850930454499,-3.21284954599589));
#34277=CARTESIAN_POINT('Ctrl Pts',(218.493215552867,12.0163773338614,-1.31364779420564));
#34278=CARTESIAN_POINT('Ctrl Pts',(218.53270660342,12.0664978923279,0.720155102320104));
#34279=CARTESIAN_POINT('Ctrl Pts',(218.572197653973,11.6294086710342,2.64322122228095));
#34280=CARTESIAN_POINT('Ctrl Pts',(218.611688704526,11.1923194497406,4.56628734224172));
#34281=CARTESIAN_POINT('Ctrl Pts',(218.651179755078,10.2680204486868,6.37861668563754));
#34282=CARTESIAN_POINT('Ctrl Pts',(218.690670805631,8.96800998266048,7.86158771615087));
#34283=CARTESIAN_POINT('Ctrl Pts',(218.730161856184,7.66799951663418,9.3445587466642));
#34284=CARTESIAN_POINT('Ctrl Pts',(218.769652906737,5.99227758563538,10.4981714642951));
#34285=CARTESIAN_POINT('Ctrl Pts',(218.809143957289,4.14298675516752,11.18326540928));
#34286=CARTESIAN_POINT('Ctrl Pts',(218.848635007842,2.29369592469966,11.8683593542649));
#34287=CARTESIAN_POINT('Ctrl Pts',(218.888126058395,0.270836194762722,12.0849345266039));
#34288=CARTESIAN_POINT('Ctrl Pts',(218.927617108948,-1.68157458903359,11.8068654336887));
#34289=CARTESIAN_POINT('Ctrl Pts',(218.9671081595,-3.6339853728299,11.5287963407735));
#34290=CARTESIAN_POINT('Ctrl Pts',(219.006599210053,-5.51594721048561,10.7560829826041));
#34291=CARTESIAN_POINT('Ctrl Pts',(219.046090260606,-7.10043878836543,9.5819378771089));
#34292=CARTESIAN_POINT('Ctrl Pts',(219.085581311159,-8.68493036624525,8.4077927716137));
#34293=CARTESIAN_POINT('Ctrl Pts',(219.125072361712,-9.97195168434919,6.83221591879273));
#34294=CARTESIAN_POINT('Ctrl Pts',(219.164563412264,-10.806249185254,5.04526936978167));
#34295=CARTESIAN_POINT('Ctrl Pts',(219.199323325792,-11.5405955392276,3.47240395715747));
#34296=CARTESIAN_POINT('Ctrl Pts',(219.23408323932,-11.9241953954151,1.73578046983011));
#34297=CARTESIAN_POINT('Ctrl Pts',(219.268843152848,-11.9256599882878,-0.000216904810520898));
#34298=CARTESIAN_POINT('Origin',(212.6,0.,0.));
#34299=CARTESIAN_POINT('',(220.981156847152,-11.9240411815327,1.80394148113772E-5));
#34300=CARTESIAN_POINT('',(220.768843152848,-11.9240373570162,-7.43698370121595E-5));
#34301=CARTESIAN_POINT('',(212.6,-11.925,-1.46039130798322E-15));
#34302=CARTESIAN_POINT('Ctrl Pts',(220.981156847152,-11.9240411815327,1.80394148113772E-5));
#34303=CARTESIAN_POINT('Ctrl Pts',(220.96063141311,-11.9239219583868,1.02549140231068));
#34304=CARTESIAN_POINT('Ctrl Pts',(220.940105979067,-11.7929513953952,2.05097956229081));
#34305=CARTESIAN_POINT('Ctrl Pts',(220.919580545025,-11.5314859766584,3.04206109250113));
#34306=CARTESIAN_POINT('Ctrl Pts',(220.880089494472,-11.0284250402679,4.94890753145148));
#34307=CARTESIAN_POINT('Ctrl Pts',(220.84059844392,-10.0422985541953,6.7283875893475));
#34308=CARTESIAN_POINT('Ctrl Pts',(220.801107393367,-8.6920036461207,8.16572986837976));
#34309=CARTESIAN_POINT('Ctrl Pts',(220.761616342814,-7.34170873804613,9.60307214741197));
#34310=CARTESIAN_POINT('Ctrl Pts',(220.722125292261,-5.62724540796957,10.6982766475804));
#34311=CARTESIAN_POINT('Ctrl Pts',(220.682634241708,-3.7554581716358,11.3192820256276));
#34312=CARTESIAN_POINT('Ctrl Pts',(220.643143191156,-1.88367093530202,11.9402874036747));
#34313=CARTESIAN_POINT('Ctrl Pts',(220.603652140603,0.145440207288969,12.0870936596005));
#34314=CARTESIAN_POINT('Ctrl Pts',(220.56416109005,2.08711696474266,11.7419659708025));
#34315=CARTESIAN_POINT('Ctrl Pts',(220.524670039497,4.02879372219635,11.3968382820046));
#34316=CARTESIAN_POINT('Ctrl Pts',(220.485178988944,5.88303609451274,10.559776648483));
#34317=CARTESIAN_POINT('Ctrl Pts',(220.445687938392,7.4261600300081,9.33176816120625));
#34318=CARTESIAN_POINT('Ctrl Pts',(220.406196887839,8.96928396550346,8.10375967392952));
#34319=CARTESIAN_POINT('Ctrl Pts',(220.366705837286,10.2012894641778,6.4848043328977));
#34320=CARTESIAN_POINT('Ctrl Pts',(220.327214786733,10.9735626651117,4.67019108695998));
#34321=CARTESIAN_POINT('Ctrl Pts',(220.287723736181,11.7458358660456,2.85557784102226));
#34322=CARTESIAN_POINT('Ctrl Pts',(220.248232685628,12.0583767692391,0.845306690178657));
#34323=CARTESIAN_POINT('Ctrl Pts',(220.208741635075,11.8734820243007,-1.11812027943816));
#34324=CARTESIAN_POINT('Ctrl Pts',(220.169250584522,11.6885872793624,-3.08154724905498));
#34325=CARTESIAN_POINT('Ctrl Pts',(220.12975953397,11.0062568862923,-4.998130037445));
#34326=CARTESIAN_POINT('Ctrl Pts',(220.090268483417,9.90880117091153,-6.63667234241024));
#34327=CARTESIAN_POINT('Ctrl Pts',(220.050777432864,8.81134545553077,-8.27521464737553));
#34328=CARTESIAN_POINT('Ctrl Pts',(220.011286382311,7.29876441783939,-9.63571646891601));
#34329=CARTESIAN_POINT('Ctrl Pts',(219.971795331758,5.55352057176231,-10.554059644325));
#34330=CARTESIAN_POINT('Ctrl Pts',(219.932304281206,3.80827672568522,-11.472402819734));
#34331=CARTESIAN_POINT('Ctrl Pts',(219.892813230653,1.83037007122243,-11.9485873490116));
#34332=CARTESIAN_POINT('Ctrl Pts',(219.8533221801,-0.141604077312892,-11.92517133466));
#34333=CARTESIAN_POINT('Ctrl Pts',(219.813831129547,-2.11357822584816,-11.9017553203085));
#34334=CARTESIAN_POINT('Ctrl Pts',(219.774340078995,-4.07961986845595,-11.3787387623278));
#34335=CARTESIAN_POINT('Ctrl Pts',(219.734849028442,-5.80256521181501,-10.4192130724648));
#34336=CARTESIAN_POINT('Ctrl Pts',(219.695357977889,-7.52551055517407,-9.45968738260177));
#34337=CARTESIAN_POINT('Ctrl Pts',(219.655866927336,-9.00535959928439,-8.06365256085633));
#34338=CARTESIAN_POINT('Ctrl Pts',(219.616375876784,-10.063597914105,-6.39951254893597));
#34339=CARTESIAN_POINT('Ctrl Pts',(219.576884826231,-11.1218362289256,-4.73537253701557));
#34340=CARTESIAN_POINT('Ctrl Pts',(219.537393775678,-11.7584638144564,-2.80312733492023));
#34341=CARTESIAN_POINT('Ctrl Pts',(219.497902725125,-11.8966842160899,-0.83586391168958));
#34342=CARTESIAN_POINT('Ctrl Pts',(219.492320765801,-11.9162213175072,-0.557796241793535));
#34343=CARTESIAN_POINT('Ctrl Pts',(219.486738806476,-11.925800691038,-0.279028939291055));
#34344=CARTESIAN_POINT('Ctrl Pts',(219.481156847152,-11.9255450374969,-0.000244099323242208));
#34345=CARTESIAN_POINT('Ctrl Pts',(219.268843152848,-11.9256599882878,-0.000216904810520898));
#34346=CARTESIAN_POINT('Ctrl Pts',(219.273574289873,-11.9258593325571,-0.236501769201835));
#34347=CARTESIAN_POINT('Ctrl Pts',(219.278305426898,-11.9189793690461,-0.472775034442688));
#34348=CARTESIAN_POINT('Ctrl Pts',(219.283036563923,-11.9049409507008,-0.708622204330391));
#34349=CARTESIAN_POINT('Ctrl Pts',(219.322527614475,-11.787761531537,-2.67725098423027));
#34350=CARTESIAN_POINT('Ctrl Pts',(219.362018665028,-11.1718290095037,-4.61619229882879));
#34351=CARTESIAN_POINT('Ctrl Pts',(219.401509715581,-10.1314434090349,-6.2915513919816));
#34352=CARTESIAN_POINT('Ctrl Pts',(219.441000766134,-9.09105780856628,-7.96691048513431));
#34353=CARTESIAN_POINT('Ctrl Pts',(219.480491816687,-7.62621912966225,-9.37868735684133));
#34354=CARTESIAN_POINT('Ctrl Pts',(219.519982867239,-5.91363106200984,-10.3565791710799));
#34355=CARTESIAN_POINT('Ctrl Pts',(219.559473917792,-4.20104299435734,-11.3344709853185));
#34356=CARTESIAN_POINT('Ctrl Pts',(219.598964968345,-2.24070553795645,-11.8784777420885));
#34357=CARTESIAN_POINT('Ctrl Pts',(219.638456018898,-0.269094468648538,
-11.9229758300881));
#34358=CARTESIAN_POINT('Ctrl Pts',(219.67794706945,1.70251660065938,-11.9674739180876));
#34359=CARTESIAN_POINT('Ctrl Pts',(219.717438120003,3.68540128287429,-11.5124633373165));
#34360=CARTESIAN_POINT('Ctrl Pts',(219.756929170556,5.44036392915078,-10.6128320802783));
#34361=CARTESIAN_POINT('Ctrl Pts',(219.796420221109,7.19532657542723,-9.71320082324006));
#34362=CARTESIAN_POINT('Ctrl Pts',(219.835911271661,8.72236718576524,-8.36894888993472));
#34363=CARTESIAN_POINT('Ctrl Pts',(219.875402322214,9.83727863996894,-6.74223356644574));
#34364=CARTESIAN_POINT('Ctrl Pts',(219.914893372767,10.9521900941726,-5.11551824295682));
#34365=CARTESIAN_POINT('Ctrl Pts',(219.95438442332,11.654972392242,-3.20633952928414));
#34366=CARTESIAN_POINT('Ctrl Pts',(219.993875473873,11.8608488152243,-1.24500193187064));
#34367=CARTESIAN_POINT('Ctrl Pts',(220.033366524425,12.0667252382066,0.716335665542974));
#34368=CARTESIAN_POINT('Ctrl Pts',(220.072857574978,11.7756957861018,2.72983214669756));
#34369=CARTESIAN_POINT('Ctrl Pts',(220.112348625531,11.0228673695967,4.55259919220793));
#34370=CARTESIAN_POINT('Ctrl Pts',(220.151839676084,10.2700389530916,6.3753662377182));
#34371=CARTESIAN_POINT('Ctrl Pts',(220.191330726636,9.05541157218612,8.00740384758426));
#34372=CARTESIAN_POINT('Ctrl Pts',(220.230821777189,7.52550591863462,9.25183902618784));
#34373=CARTESIAN_POINT('Ctrl Pts',(220.270312827742,5.99560026508303,10.4962742047915));
#34374=CARTESIAN_POINT('Ctrl Pts',(220.309803878295,4.15041633888536,11.3531069521326));
#34375=CARTESIAN_POINT('Ctrl Pts',(220.349294928847,2.21253887728794,11.7189775750894));
#34376=CARTESIAN_POINT('Ctrl Pts',(220.3887859794,0.274661415690581,12.0848481980461));
#34377=CARTESIAN_POINT('Ctrl Pts',(220.428277029953,-1.75590958130649,11.9597566966185));
#34378=CARTESIAN_POINT('Ctrl Pts',(220.467768080506,-3.63422594846958,11.3587925450367));
#34379=CARTESIAN_POINT('Ctrl Pts',(220.507259131059,-5.51254231563271,10.757828393455));
#34380=CARTESIAN_POINT('Ctrl Pts',(220.546750181611,-7.23860405296182,9.68099159171901));
#34381=CARTESIAN_POINT('Ctrl Pts',(220.586241232164,-8.60419632377035,8.25818180128231));
#34382=CARTESIAN_POINT('Ctrl Pts',(220.625732282717,-9.96978859457889,6.83537201084561));
#34383=CARTESIAN_POINT('Ctrl Pts',(220.66522333327,-10.9749113988668,5.06658923170817));
#34384=CARTESIAN_POINT('Ctrl Pts',(220.704714383822,-11.4983161621042,3.16520052856484));
#34385=CARTESIAN_POINT('Ctrl Pts',(220.726090640164,-11.7816318559873,2.13599082775773));
#34386=CARTESIAN_POINT('Ctrl Pts',(220.747466896506,-11.9238047153297,1.06792774302866));
#34387=CARTESIAN_POINT('Ctrl Pts',(220.768843152848,-11.9240373570162,-7.43698370121595E-5));
#34388=CARTESIAN_POINT('Origin',(201.227129595899,0.,0.));
#34389=CARTESIAN_POINT('',(219.977129595899,-11.0664557742297,-0.000226514961028955));
#34390=CARTESIAN_POINT('',(220.272870404101,-11.0650567036372,-6.90124023777772E-5));
#34391=CARTESIAN_POINT('',(201.227129595899,-11.06595,-5.55035408696717E-13));
#34392=CARTESIAN_POINT('',(221.275,-7.33091411968472,8.28932732930165));
#34393=CARTESIAN_POINT('Ctrl Pts',(219.977129595899,-11.0664557742297,-0.00022651496102942));
#34394=CARTESIAN_POINT('Ctrl Pts',(219.982711555224,-11.0666930110685,-0.258928326268467));
#34395=CARTESIAN_POINT('Ctrl Pts',(220.027784565101,-10.9949140254131,-2.34775325236548));
#34396=CARTESIAN_POINT('Ctrl Pts',(220.112348625531,-9.72987795281957,-6.18729765367837));
#34397=CARTESIAN_POINT('Ctrl Pts',(220.230821777189,-5.61014574409689,-10.0737005557397));
#34398=CARTESIAN_POINT('Ctrl Pts',(220.349294928847,-0.136908381828727,
-11.5297194437361));
#34399=CARTESIAN_POINT('Ctrl Pts',(220.467768080506,5.36935983023475,-10.20407562191));
#34400=CARTESIAN_POINT('Ctrl Pts',(220.586241232164,9.58021420357832,-6.41659256981546));
#34401=CARTESIAN_POINT('Ctrl Pts',(220.704714383822,11.4797447729354,-1.08104305857399));
#34402=CARTESIAN_POINT('Ctrl Pts',(220.823187535481,10.6096662804338,4.51532424750848));
#34403=CARTESIAN_POINT('Ctrl Pts',(220.941660687139,7.17990244444507,9.02231263897793));
#34404=CARTESIAN_POINT('Ctrl Pts',(221.060133838797,2.01790159414706,11.3525974650078));
#34405=CARTESIAN_POINT('Ctrl Pts',(221.171246943085,-3.27998607346621,10.9692951231732));
#34406=CARTESIAN_POINT('Ctrl Pts',(221.242868996819,-6.21473622449859,9.27482791577466));
#34407=CARTESIAN_POINT('Ctrl Pts',(221.275,-7.33129268303492,8.28936271098459));
#34408=CARTESIAN_POINT('',(221.275,5.44726799658334,9.63236838871412));
#34409=CARTESIAN_POINT('Origin',(221.275,0.,0.));
#34410=CARTESIAN_POINT('Ctrl Pts',(220.272870404101,-11.0650567036372,-6.90124023777772E-5));
#34411=CARTESIAN_POINT('Ctrl Pts',(220.290985198312,-11.0652396482432,-0.839923763907543));
#34412=CARTESIAN_POINT('Ctrl Pts',(220.348591043075,-10.7650251550423,-3.51056971559727));
#34413=CARTESIAN_POINT('Ctrl Pts',(220.445687938392,-8.639031892527,-7.6367698092379));
#34414=CARTESIAN_POINT('Ctrl Pts',(220.56416109005,-3.96073003010559,-10.828943343905));
#34415=CARTESIAN_POINT('Ctrl Pts',(220.682634241709,1.67312238226268,-11.4084734661502));
#34416=CARTESIAN_POINT('Ctrl Pts',(220.801107393367,6.9033507794017,-9.23569581394894));
#34417=CARTESIAN_POINT('Ctrl Pts',(220.919580545025,10.4680037040556,-4.83449558382035));
#34418=CARTESIAN_POINT('Ctrl Pts',(221.038053696683,11.5072892832615,0.732618747333446));
#34419=CARTESIAN_POINT('Ctrl Pts',(221.156526848342,9.7699936824466,6.12389733841086));
#34420=CARTESIAN_POINT('Ctrl Pts',(221.235508949447,7.04065173359568,8.73128281072966));
#34421=CARTESIAN_POINT('Ctrl Pts',(221.275,5.44726799658334,9.63236838871412));
#34422=CARTESIAN_POINT('Origin',(201.227129595899,0.,0.));
#34423=CARTESIAN_POINT('',(218.477129595899,-11.0661475744647,0.000270029283923045));
#34424=CARTESIAN_POINT('',(218.772870404101,-11.0665624442258,-0.000201279480846472));
#34425=CARTESIAN_POINT('',(201.227129595899,-11.06595,-5.55035408696717E-13));
#34426=CARTESIAN_POINT('Ctrl Pts',(218.477129595899,-11.0661475744646,0.000270029283922883));
#34427=CARTESIAN_POINT('Ctrl Pts',(218.50881894859,-11.064660089562,-1.46852466027703));
#34428=CARTESIAN_POINT('Ctrl Pts',(218.579999351834,-10.4036740682491,-4.7690199151945));
#34429=CARTESIAN_POINT('Ctrl Pts',(218.690670805631,-7.21724808383853,-8.99246948207381));
#34430=CARTESIAN_POINT('Ctrl Pts',(218.809143957289,-2.06496223864743,-11.3441221891729));
#34431=CARTESIAN_POINT('Ctrl Pts',(218.927617108948,3.58551696051438,-10.9588888768492));
#34432=CARTESIAN_POINT('Ctrl Pts',(219.046090260606,8.37095335800593,-7.92971103942582));
#34433=CARTESIAN_POINT('Ctrl Pts',(219.164563412264,11.1368112607131,-2.98740894949973));
#34434=CARTESIAN_POINT('Ctrl Pts',(219.283036563923,11.2157990354753,2.67563623960653));
#34435=CARTESIAN_POINT('Ctrl Pts',(219.401509715581,8.58886006959068,7.69315669910092));
#34436=CARTESIAN_POINT('Ctrl Pts',(219.519982867239,3.8897703770425,10.8546240695241));
#34437=CARTESIAN_POINT('Ctrl Pts',(219.638456018897,-1.74776638133898,11.3973018738637));
#34438=CARTESIAN_POINT('Ctrl Pts',(219.756929170556,-6.96363654138209,9.19026350689656));
#34439=CARTESIAN_POINT('Ctrl Pts',(219.86982036289,-10.3328647442766,4.97443341609356));
#34440=CARTESIAN_POINT('Ctrl Pts',(219.943220504671,-11.0650146161803,1.57132619810322));
#34441=CARTESIAN_POINT('Ctrl Pts',(219.977129595899,-11.0664557742297,-0.00022651496102942));
#34442=CARTESIAN_POINT('Ctrl Pts',(218.772870404101,-11.0665624442258,-0.000201279480847652));
#34443=CARTESIAN_POINT('Ctrl Pts',(218.777601541126,-11.0667474281854,-0.219464717225433));
#34444=CARTESIAN_POINT('Ctrl Pts',(218.821823728703,-11.007072604194,-2.26883103935306));
#34445=CARTESIAN_POINT('Ctrl Pts',(218.905536966834,-9.79547360465598,-6.08291662972795));
#34446=CARTESIAN_POINT('Ctrl Pts',(219.024010118492,-5.71752855338079,-10.0131436167636));
#34447=CARTESIAN_POINT('Ctrl Pts',(219.14248327015,-0.260170999755849,-11.5275968419408));
#34448=CARTESIAN_POINT('Ctrl Pts',(219.260956421809,5.25995547801919,-10.260898895706));
#34449=CARTESIAN_POINT('Ctrl Pts',(219.379429573467,9.51106366467834,-6.51865369284798));
#34450=CARTESIAN_POINT('Ctrl Pts',(219.497902725125,11.4675300222433,-1.2037162874228));
#34451=CARTESIAN_POINT('Ctrl Pts',(219.616375876784,10.657336974314,4.40162997311355));
#34452=CARTESIAN_POINT('Ctrl Pts',(219.734849028442,7.27595185085969,8.94503792000617));
#34453=CARTESIAN_POINT('Ctrl Pts',(219.8533221801,2.13916868907181,11.3303632886701));
#34454=CARTESIAN_POINT('Ctrl Pts',(219.971795331758,-3.51371109060621,10.9821227099977));
#34455=CARTESIAN_POINT('Ctrl Pts',(220.090268483417,-8.31887156411482,7.98433096001791));
#34456=CARTESIAN_POINT('Ctrl Pts',(220.190626840864,-10.6891769307306,3.81314382160942));
#34457=CARTESIAN_POINT('Ctrl Pts',(220.251494147759,-11.0648408209311,0.990996646370493));
#34458=CARTESIAN_POINT('Ctrl Pts',(220.272870404101,-11.0650567036372,-6.90124023777772E-5));
#34459=CARTESIAN_POINT('Origin',(201.227129595899,0.,0.));
#34460=CARTESIAN_POINT('',(216.977129595899,-11.0650512767152,-6.05169948032443E-5));
#34461=CARTESIAN_POINT('',(217.272870404101,-11.0660244859104,0.000277648619103621));
#34462=CARTESIAN_POINT('',(201.227129595899,-11.06595,-5.55035408696717E-13));
#34463=CARTESIAN_POINT('Ctrl Pts',(216.977129595899,-11.0650512767152,-6.05169948027923E-5));
#34464=CARTESIAN_POINT('Ctrl Pts',(216.995435291404,-11.0652148268645,-0.848767003760925));
#34465=CARTESIAN_POINT('Ctrl Pts',(217.053232037462,-10.7607722633556,-3.52828058602642));
#34466=CARTESIAN_POINT('Ctrl Pts',(217.150519834073,-8.62068509653071,-7.65747776726749));
#34467=CARTESIAN_POINT('Ctrl Pts',(217.268992985731,-3.93474448792423,-10.8384022394674));
#34468=CARTESIAN_POINT('Ctrl Pts',(217.38746613739,1.70049365109212,-11.4044508255478));
#34469=CARTESIAN_POINT('Ctrl Pts',(217.505939289048,6.92547022714963,-9.21905848894597));
#34470=CARTESIAN_POINT('Ctrl Pts',(217.624412440706,10.4796059636719,-4.80947358199571));
#34471=CARTESIAN_POINT('Ctrl Pts',(217.742885592365,11.5054291016218,0.760446235638654));
#34472=CARTESIAN_POINT('Ctrl Pts',(217.861358744023,9.75544927040927,6.14690058665455));
#34473=CARTESIAN_POINT('Ctrl Pts',(217.979831895681,5.65186708233216,10.0503520223619));
#34474=CARTESIAN_POINT('Ctrl Pts',(218.098305047339,0.184713897477963,11.5290527826799));
#34475=CARTESIAN_POINT('Ctrl Pts',(218.216778198998,-5.32700341275905,10.2262511180883));
#34476=CARTESIAN_POINT('Ctrl Pts',(218.335251350656,-9.55352642391547,6.4562613142035));
#34477=CARTESIAN_POINT('Ctrl Pts',(218.422035149623,-10.9611611781699,2.5536733215898));
#34478=CARTESIAN_POINT('Ctrl Pts',(218.469327898038,-11.0665137828848,0.361877049166292));
#34479=CARTESIAN_POINT('Ctrl Pts',(218.477129595899,-11.0661475744646,0.000270029283922883));
#34480=CARTESIAN_POINT('Ctrl Pts',(217.272870404101,-11.0660244859104,0.000277648619103552));
#34481=CARTESIAN_POINT('Ctrl Pts',(217.303708934492,-11.0645721443471,-1.42912743809139));
#34482=CARTESIAN_POINT('Ctrl Pts',(217.374038515437,-10.42991951896,-4.69024517517523));
#34483=CARTESIAN_POINT('Ctrl Pts',(217.483859146934,-7.31297897803034,-8.91479199580349));
#34484=CARTESIAN_POINT('Ctrl Pts',(217.602332298592,-2.18613040678854,-11.3213961906678));
#34485=CARTESIAN_POINT('Ctrl Pts',(217.720805450251,3.46814458380223,-10.9965972467579));
#34486=CARTESIAN_POINT('Ctrl Pts',(217.839278601909,8.28569406435969,-8.01875624603833));
#34487=CARTESIAN_POINT('Ctrl Pts',(217.957751753567,11.104234730707,-3.1063079221047));
#34488=CARTESIAN_POINT('Ctrl Pts',(218.076224905225,11.2437646914523,2.55556909998565));
#34489=CARTESIAN_POINT('Ctrl Pts',(218.194698056884,8.6706209101412,7.60088882263999));
#34490=CARTESIAN_POINT('Ctrl Pts',(218.313171208542,4.00560075861009,10.8124160308581));
#34491=CARTESIAN_POINT('Ctrl Pts',(218.4316443602,-1.62581172654604,11.4153367927059));
#34492=CARTESIAN_POINT('Ctrl Pts',(218.550117511859,-6.86498043029599,9.26419028054612));
#34493=CARTESIAN_POINT('Ctrl Pts',(218.663859526492,-10.3048207733217,5.05312341969914));
#34494=CARTESIAN_POINT('Ctrl Pts',(218.738110490573,-11.0652033573079,1.61073877485134));
#34495=CARTESIAN_POINT('Ctrl Pts',(218.772870404101,-11.0665624442258,-0.000201279480847652));
#34496=CARTESIAN_POINT('Origin',(201.227129595899,0.,0.));
#34497=CARTESIAN_POINT('',(215.477129595899,-11.0665392919594,-0.000207324146620239));
#34498=CARTESIAN_POINT('',(215.772870404101,-11.065081553347,-9.51519639225129E-5));
#34499=CARTESIAN_POINT('',(201.227129595899,-11.06595,-5.55035408696717E-13));
#34500=CARTESIAN_POINT('Ctrl Pts',(215.477129595899,-11.0665392919594,-0.000207324146620537));
#34501=CARTESIAN_POINT('Ctrl Pts',(215.482051634218,-11.0667359263627,-0.228319417445807));
#34502=CARTESIAN_POINT('Ctrl Pts',(215.52646472309,-11.0043819432692,-2.28653868628294));
#34503=CARTESIAN_POINT('Ctrl Pts',(215.610368862515,-9.7808528815819,-6.10639780874076));
#34504=CARTESIAN_POINT('Ctrl Pts',(215.728842014173,-5.6934912171844,-10.0268307580006));
#34505=CARTESIAN_POINT('Ctrl Pts',(215.847315165831,-0.232516305860531,
-11.5281877785388));
#34506=CARTESIAN_POINT('Ctrl Pts',(215.96578831749,5.28455555295532,-10.2482510653024));
#34507=CARTESIAN_POINT('Ctrl Pts',(216.084261469148,9.52667409494713,-6.4958184994969));
#34508=CARTESIAN_POINT('Ctrl Pts',(216.202734620806,11.4703846414241,-1.17620298738114));
#34509=CARTESIAN_POINT('Ctrl Pts',(216.321207772465,10.6467470547827,4.42718357889284));
#34510=CARTESIAN_POINT('Ctrl Pts',(216.439680924123,7.25447236425265,8.96246662510033));
#34511=CARTESIAN_POINT('Ctrl Pts',(216.558154075782,2.11198168868298,11.3354625241501));
#34512=CARTESIAN_POINT('Ctrl Pts',(216.67662722744,-3.54004626624265,10.9736616369653));
#34513=CARTESIAN_POINT('Ctrl Pts',(216.795100379098,-8.33800169158112,7.96435214445806));
#34514=CARTESIAN_POINT('Ctrl Pts',(216.895267835251,-10.6938035719187,3.79543445167127));
#34515=CARTESIAN_POINT('Ctrl Pts',(216.955944240852,-11.064861998576,0.982155550582976));
#34516=CARTESIAN_POINT('Ctrl Pts',(216.977129595899,-11.0650512767152,-6.05169948027923E-5));
#34517=CARTESIAN_POINT('Ctrl Pts',(215.772870404101,-11.065081553347,-9.51519639225129E-5));
#34518=CARTESIAN_POINT('Ctrl Pts',(215.790325277306,-11.0653275880705,-0.809348655494953));
#34519=CARTESIAN_POINT('Ctrl Pts',(215.847271201065,-10.7795512155158,-3.44933924082071));
#34520=CARTESIAN_POINT('Ctrl Pts',(215.943708175376,-8.70206265507251,-7.56487167166418));
#34521=CARTESIAN_POINT('Ctrl Pts',(216.062181327034,-4.05039886300789,-10.7957142844788));
#34522=CARTESIAN_POINT('Ctrl Pts',(216.180654478693,1.57846526560428,-11.4219799188598));
#34523=CARTESIAN_POINT('Ctrl Pts',(216.299127630351,6.8265084328873,-9.29257555671587));
#34524=CARTESIAN_POINT('Ctrl Pts',(216.417600782009,10.4275863101622,-4.92124187636331));
#34525=CARTESIAN_POINT('Ctrl Pts',(216.536073933668,11.512901864686,0.637391963915507));
#34526=CARTESIAN_POINT('Ctrl Pts',(216.654547085325,9.82061156918846,6.04224844479904));
#34527=CARTESIAN_POINT('Ctrl Pts',(216.773020236984,5.75899784281591,9.98935041471651));
#34528=CARTESIAN_POINT('Ctrl Pts',(216.891493388642,0.307966723115988,11.5264189737753));
#34529=CARTESIAN_POINT('Ctrl Pts',(217.009966540301,-5.21736453236138,10.2826205413801));
#34530=CARTESIAN_POINT('Ctrl Pts',(217.128439691959,-9.48395299500455,6.55803426722514));
#34531=CARTESIAN_POINT('Ctrl Pts',(217.216074313226,-10.9474406210577,2.63260814707565));
#34532=CARTESIAN_POINT('Ctrl Pts',(217.26421788394,-11.0664319766208,0.401332957488395));
#34533=CARTESIAN_POINT('Ctrl Pts',(217.272870404101,-11.0660244859104,0.000277648619103552));
#34534=CARTESIAN_POINT('Origin',(201.227129595899,0.,0.));
#34535=CARTESIAN_POINT('',(213.977129595899,-11.0660521098639,0.000276383857342581));
#34536=CARTESIAN_POINT('',(214.272870404101,-11.0666382248001,-0.000178769468103801));
#34537=CARTESIAN_POINT('',(201.227129595899,-11.06595,-5.55035408696717E-13));
#34538=CARTESIAN_POINT('Ctrl Pts',(213.977129595899,-11.0660521098639,0.000276383857342327));
#34539=CARTESIAN_POINT('Ctrl Pts',(214.008159027585,-11.0645897179147,-1.437966866595));
#34540=CARTESIAN_POINT('Ctrl Pts',(214.078679509824,-10.424073677229,-4.70792184462568));
#34541=CARTESIAN_POINT('Ctrl Pts',(214.188691042615,-7.2915719210082,-8.93230967950104));
#34542=CARTESIAN_POINT('Ctrl Pts',(214.307164194274,-2.15896482813512,-11.3266079724081));
#34543=CARTESIAN_POINT('Ctrl Pts',(214.425637345932,3.4945147091572,-10.9882457306536));
#34544=CARTESIAN_POINT('Ctrl Pts',(214.54411049759,8.30490667276723,-7.99885632114799));
#34545=CARTESIAN_POINT('Ctrl Pts',(214.662583649248,11.1116545830117,-3.0796606497433));
#34546=CARTESIAN_POINT('Ctrl Pts',(214.781056800907,11.2376016720611,2.58253479160174));
#34547=CARTESIAN_POINT('Ctrl Pts',(214.899529952565,8.65236191079344,7.62166718339193));
#34548=CARTESIAN_POINT('Ctrl Pts',(215.018003104223,3.9796509504845,10.8219940677331));
#34549=CARTESIAN_POINT('Ctrl Pts',(215.136476255882,-1.65319168566326,11.4114037059512));
#34550=CARTESIAN_POINT('Ctrl Pts',(215.25494940754,-6.88718484395786,9.24769496766087));
#34551=CARTESIAN_POINT('Ctrl Pts',(215.368500520879,-10.3111568532547,5.0354698445964));
#34552=CARTESIAN_POINT('Ctrl Pts',(215.442560583666,-11.0651582671375,1.60189514492085));
#34553=CARTESIAN_POINT('Ctrl Pts',(215.477129595899,-11.0665392919594,-0.000207324146620537));
#34554=CARTESIAN_POINT('Ctrl Pts',(214.272870404101,-11.0666382248001,-0.000178769468104391));
#34555=CARTESIAN_POINT('Ctrl Pts',(214.27694162012,-11.0667838005927,-0.188854579626239));
#34556=CARTESIAN_POINT('Ctrl Pts',(214.320503886693,-11.0162073889607,-2.20761953155798));
#34557=CARTESIAN_POINT('Ctrl Pts',(214.403557203818,-9.84558069118264,-6.00147637793954));
#34558=CARTESIAN_POINT('Ctrl Pts',(214.522030355476,-5.80036812003173,-9.96538546839381));
#34559=CARTESIAN_POINT('Ctrl Pts',(214.640503507134,-0.355757151167077,
-11.5250429374883));
#34560=CARTESIAN_POINT('Ctrl Pts',(214.758976658793,5.17468388520643,-10.3041653980194));
#34561=CARTESIAN_POINT('Ctrl Pts',(214.877449810451,9.4566792733418,-6.59730209879029));
#34562=CARTESIAN_POINT('Ctrl Pts',(214.995922962109,11.4571536357504,-1.29877189235286));
#34563=CARTESIAN_POINT('Ctrl Pts',(215.114396113768,10.6934719810851,4.31310037575084));
#34564=CARTESIAN_POINT('Ctrl Pts',(215.232869265426,7.34988035404288,8.88439286855379));
#34565=CARTESIAN_POINT('Ctrl Pts',(215.351342417084,2.23305458427189,11.3122343100387));
#34566=CARTESIAN_POINT('Ctrl Pts',(215.469815568742,-3.42251854473055,11.0108830105732));
#34567=CARTESIAN_POINT('Ctrl Pts',(215.588288720401,-8.25237391435474,8.05304306701711));
#34568=CARTESIAN_POINT('Ctrl Pts',(215.689306998854,-10.6730009525744,3.87435598552514));
#34569=CARTESIAN_POINT('Ctrl Pts',(215.750834226754,-11.0647709429668,1.02155957521071));
#34570=CARTESIAN_POINT('Ctrl Pts',(215.772870404101,-11.065081553347,-9.51519639225129E-5));
#34571=CARTESIAN_POINT('Origin',(201.227129595899,0.,0.));
#34572=CARTESIAN_POINT('',(212.477129595899,-11.0650735657267,-8.74940401521985E-5));
#34573=CARTESIAN_POINT('',(212.772870404101,-11.0659292686802,0.000280042182215501));
#34574=CARTESIAN_POINT('',(201.227129595899,-11.06595,-5.55035408696717E-13));
#34575=CARTESIAN_POINT('Ctrl Pts',(212.477129595899,-11.0650735657267,-8.74940401521251E-5));
#34576=CARTESIAN_POINT('Ctrl Pts',(212.494775370399,-11.06530206838,-0.818193363706625));
#34577=CARTESIAN_POINT('Ctrl Pts',(212.551912195452,-10.775377450498,-3.46705175012318));
#34578=CARTESIAN_POINT('Ctrl Pts',(212.648540071057,-8.68388996795875,-7.58572556280073));
#34579=CARTESIAN_POINT('Ctrl Pts',(212.767013222715,-4.02448899226784,-10.8053998371582));
#34580=CARTESIAN_POINT('Ctrl Pts',(212.885486374374,1.60586129747547,-11.4181603939958));
#34581=CARTESIAN_POINT('Ctrl Pts',(213.003959526032,6.84878105175381,-9.27617245392087));
#34582=CARTESIAN_POINT('Ctrl Pts',(213.12243267769,10.4393620179098,-4.89621261270018));
#34583=CARTESIAN_POINT('Ctrl Pts',(213.240905829349,11.5113396508456,0.665008821455645));
#34584=CARTESIAN_POINT('Ctrl Pts',(213.359378981007,9.806088333898,6.06579004561915));
#34585=CARTESIAN_POINT('Ctrl Pts',(213.477852132665,5.73501746579043,10.0031371057694));
#34586=CARTESIAN_POINT('Ctrl Pts',(213.596325284323,0.280314716669852,11.5271245742102));
#34587=CARTESIAN_POINT('Ctrl Pts',(213.714798435982,-5.24201683759653,10.2700748178432));
#34588=CARTESIAN_POINT('Ctrl Pts',(213.83327158764,-9.49965797713093,6.5352640044053));
#34589=CARTESIAN_POINT('Ctrl Pts',(213.920715307613,-10.9505570442949,2.61489706102027));
#34590=CARTESIAN_POINT('Ctrl Pts',(213.968667977032,-11.0664508990984,0.392480351575348));
#34591=CARTESIAN_POINT('Ctrl Pts',(213.977129595899,-11.0660521098639,0.000276383857342327));
#34592=CARTESIAN_POINT('Ctrl Pts',(212.772870404101,-11.0659292686802,0.000280042182215223));
#34593=CARTESIAN_POINT('Ctrl Pts',(212.803049013487,-11.0645204618591,-1.39857152109217));
#34594=CARTESIAN_POINT('Ctrl Pts',(212.872718673426,-10.4499369733853,-4.62913162145941));
#34595=CARTESIAN_POINT('Ctrl Pts',(212.981879383918,-7.3866553660777,-8.85384099497784));
#34596=CARTESIAN_POINT('Ctrl Pts',(213.100352535576,-2.27994036961207,-11.3028779420362));
#34597=CARTESIAN_POINT('Ctrl Pts',(213.218825687235,3.37683366346876,-11.0249794680452));
#34598=CARTESIAN_POINT('Ctrl Pts',(213.337298838893,8.21891188410895,-8.08719143478177));
#34599=CARTESIAN_POINT('Ctrl Pts',(213.455771990551,11.0780931775952,-3.1982853859645));
#34600=CARTESIAN_POINT('Ctrl Pts',(213.574245142209,11.2645706837284,2.46223986907059));
#34601=CARTESIAN_POINT('Ctrl Pts',(213.692718293868,8.73335478842003,7.52872446043392));
#34602=CARTESIAN_POINT('Ctrl Pts',(213.811191445526,4.09512733028103,10.7788269310876));
#34603=CARTESIAN_POINT('Ctrl Pts',(213.929664597184,-1.53109166664286,11.4284266708017));
#34604=CARTESIAN_POINT('Ctrl Pts',(214.048137748843,-6.78791906966887,9.32080106885565));
#34605=CARTESIAN_POINT('Ctrl Pts',(214.162539684481,-10.28272188813,5.11413873802353));
#34606=CARTESIAN_POINT('Ctrl Pts',(214.237450569567,-11.0653717062799,1.64131260416363));
#34607=CARTESIAN_POINT('Ctrl Pts',(214.272870404101,-11.0666382248001,-0.000178769468104391));
#34608=CARTESIAN_POINT('Origin',(201.227129595899,0.,0.));
#34609=CARTESIAN_POINT('',(210.977129595899,-11.0666169876618,-0.000185531372268859));
#34610=CARTESIAN_POINT('',(211.272870404101,-11.0651142296248,-0.000120992757266514));
#34611=CARTESIAN_POINT('',(201.227129595899,-11.06595,-5.55035408696717E-13));
#34612=CARTESIAN_POINT('Ctrl Pts',(210.977129595899,-11.0666169876618,-0.000185531372269392));
#34613=CARTESIAN_POINT('Ctrl Pts',(210.981391713213,-11.0667737867174,-0.197709538727662));
#34614=CARTESIAN_POINT('Ctrl Pts',(211.02514488108,-11.0135913758753,-2.22532648196755));
#34615=CARTESIAN_POINT('Ctrl Pts',(211.108389099499,-9.83115519349314,-6.02507799544502));
#34616=CARTESIAN_POINT('Ctrl Pts',(211.226862251157,-5.77644511420377,-9.97927147302517));
#34617=CARTESIAN_POINT('Ctrl Pts',(211.345335402816,-0.328108308124205,
-11.5258631879735));
#34618=CARTESIAN_POINT('Ctrl Pts',(211.463808554474,5.19938799803607,-10.2917220005022));
#34619=CARTESIAN_POINT('Ctrl Pts',(211.582281706132,9.47247853494596,-6.57459715075616));
#34620=CARTESIAN_POINT('Ctrl Pts',(211.700754857791,11.460236311957,-1.27128319576909));
#34621=CARTESIAN_POINT('Ctrl Pts',(211.819228009449,10.6830943445901,4.33874089043461));
#34622=CARTESIAN_POINT('Ctrl Pts',(211.937701161107,7.32854611626294,8.90199916375812));
#34623=CARTESIAN_POINT('Ctrl Pts',(212.056174312765,2.2059108492439,11.3175586861713));
#34624=CARTESIAN_POINT('Ctrl Pts',(212.174647464424,-3.44892307207615,11.0026409071933));
#34625=CARTESIAN_POINT('Ctrl Pts',(212.293120616082,-8.27166887053497,8.03322297623846));
#34626=CARTESIAN_POINT('Ctrl Pts',(212.393947993241,-10.6777090723953,3.85664871067693));
#34627=CARTESIAN_POINT('Ctrl Pts',(212.455284319846,-11.0647906819383,1.0127186349046));
#34628=CARTESIAN_POINT('Ctrl Pts',(212.477129595899,-11.0650735657267,-8.74940401521251E-5));
#34629=CARTESIAN_POINT('Ctrl Pts',(211.272870404101,-11.0651142296248,-0.000120992757266861));
#34630=CARTESIAN_POINT('Ctrl Pts',(211.289665356301,-11.0654163729725,-0.778772252662076));
#34631=CARTESIAN_POINT('Ctrl Pts',(211.345951359054,-10.7938026724476,-3.38810849938383));
#34632=CARTESIAN_POINT('Ctrl Pts',(211.44172841236,-8.7644967721873,-7.4924478104204));
#34633=CARTESIAN_POINT('Ctrl Pts',(211.560201564018,-4.13978539143139,-10.7617542610137));
#34634=CARTESIAN_POINT('Ctrl Pts',(211.678674715676,1.48369174414633,-11.4346769377148));
#34635=CARTESIAN_POINT('Ctrl Pts',(211.797147867335,6.74921300408072,-9.34886633165234));
#34636=CARTESIAN_POINT('Ctrl Pts',(211.915621018993,10.3864172902835,-5.00754567963735));
#34637=CARTESIAN_POINT('Ctrl Pts',(212.034094170651,11.5177917027214,0.541896811466134));
#34638=CARTESIAN_POINT('Ctrl Pts',(212.15256732231,9.87038054147729,5.96060112975038));
#34639=CARTESIAN_POINT('Ctrl Pts',(212.271040473968,5.84163867350336,9.94124919060903));
#34640=CARTESIAN_POINT('Ctrl Pts',(212.389513625626,0.403541462807075,11.523468755082));
#34641=CARTESIAN_POINT('Ctrl Pts',(212.507986777285,-5.13191427148244,10.325533098669));
#34642=CARTESIAN_POINT('Ctrl Pts',(212.626459928943,-9.42924296622852,6.636456505198));
#34643=CARTESIAN_POINT('Ctrl Pts',(212.714754471215,-10.9364980717932,2.6938341513483));
#34644=CARTESIAN_POINT('Ctrl Pts',(212.763557962934,-11.066363994829,0.431934222033988));
#34645=CARTESIAN_POINT('Ctrl Pts',(212.772870404101,-11.0659292686802,0.000280042182215223));
#34646=CARTESIAN_POINT('Origin',(201.227129595899,0.,0.));
#34647=CARTESIAN_POINT('',(209.477129595899,-11.0659567005612,0.00027966449786441));
#34648=CARTESIAN_POINT('',(209.772870404101,-11.0667065609126,-0.00015392667879921));
#34649=CARTESIAN_POINT('',(201.227129595899,-11.06595,-5.55035408696717E-13));
#34650=CARTESIAN_POINT('Ctrl Pts',(209.477129595899,-11.0659567005612,0.000279664497864693));
#34651=CARTESIAN_POINT('Ctrl Pts',(209.50749910658,-11.0645339567228,-1.40741057953197));
#34652=CARTESIAN_POINT('Ctrl Pts',(209.577359667813,-10.4441767046115,-4.64681166211135));
#34653=CARTESIAN_POINT('Ctrl Pts',(209.686711279599,-7.36539431433226,-8.87153559898989));
#34654=CARTESIAN_POINT('Ctrl Pts',(209.805184431257,-2.25281894488235,-11.3083148210209));
#34655=CARTESIAN_POINT('Ctrl Pts',(209.923657582916,3.40327213884093,-11.0168469190931));
#34656=CARTESIAN_POINT('Ctrl Pts',(210.042130734574,8.23828885633043,-8.06745151887539));
#34657=CARTESIAN_POINT('Ctrl Pts',(210.160603886232,11.0857337530526,-3.17170056060973));
#34658=CARTESIAN_POINT('Ctrl Pts',(210.279077037891,11.2586314950991,2.48925574164375));
#34659=CARTESIAN_POINT('Ctrl Pts',(210.397550189549,8.71526872597554,7.54965352342579));
#34660=CARTESIAN_POINT('Ctrl Pts',(210.516023341207,4.0692578423892,10.7886198330415));
#34661=CARTESIAN_POINT('Ctrl Pts',(210.634496492866,-1.55850330026388,11.4247207735161));
#34662=CARTESIAN_POINT('Ctrl Pts',(210.752969644524,-6.81025951080084,9.30449045812232));
#34663=CARTESIAN_POINT('Ctrl Pts',(210.867180678869,-10.2891458759462,5.09649002157397));
#34664=CARTESIAN_POINT('Ctrl Pts',(210.94190066266,-11.0653209502573,1.63246780871538));
#34665=CARTESIAN_POINT('Ctrl Pts',(210.977129595899,-11.0666169876618,-0.000185531372269392));
#34666=CARTESIAN_POINT('Ctrl Pts',(209.772870404101,-11.0667065609126,-0.000153926678798932));
#34667=CARTESIAN_POINT('Ctrl Pts',(209.776281699115,-11.0668149481323,-0.158243627877831));
#34668=CARTESIAN_POINT('Ctrl Pts',(209.819184044682,-11.0250845540694,-2.14641047456581));
#34669=CARTESIAN_POINT('Ctrl Pts',(209.901577440802,-9.89501069369702,-5.91962340298576));
#34670=CARTESIAN_POINT('Ctrl Pts',(210.02005059246,-5.88280879368037,-9.9169419963289));
#34671=CARTESIAN_POINT('Ctrl Pts',(210.138523744118,-0.451318836496845,
-11.5216964536208));
#34672=CARTESIAN_POINT('Ctrl Pts',(210.256996895777,5.08905642651245,-10.3467232759617));
#34673=CARTESIAN_POINT('Ctrl Pts',(210.375470047435,9.40164454536766,-6.67549681328017));
#34674=CARTESIAN_POINT('Ctrl Pts',(210.493943199093,11.4459893320066,-1.39373816520411));
#34675=CARTESIAN_POINT('Ctrl Pts',(210.612416350752,10.7288716045437,4.2242741334779));
#34676=CARTESIAN_POINT('Ctrl Pts',(210.73088950241,7.42330338187457,8.82313690034356));
#34677=CARTESIAN_POINT('Ctrl Pts',(210.849362654068,2.32678695671764,11.2933272475212));
#34678=CARTESIAN_POINT('Ctrl Pts',(210.967835805727,-3.33109072546143,11.0388863768181));
#34679=CARTESIAN_POINT('Ctrl Pts',(211.086308957385,-8.18530854892373,8.1212007622316));
#34680=CARTESIAN_POINT('Ctrl Pts',(211.187987156843,-10.6565440575799,3.9355649498659));
#34681=CARTESIAN_POINT('Ctrl Pts',(211.250174305748,-11.0647059238997,1.0521205001896));
#34682=CARTESIAN_POINT('Ctrl Pts',(211.272870404101,-11.0651142296248,-0.000120992757266861));
#34683=CARTESIAN_POINT('Origin',(201.227129595899,0.,0.));
#34684=CARTESIAN_POINT('',(207.977129595899,-11.0651039401686,-0.000113627027166958));
#34685=CARTESIAN_POINT('',(208.272870404101,-11.0658352981118,0.000279391217192781));
#34686=CARTESIAN_POINT('',(201.227129595899,-11.06595,-5.55035408696717E-13));
#34687=CARTESIAN_POINT('Ctrl Pts',(207.977129595899,-11.0651039401686,-0.000113627027167121));
#34688=CARTESIAN_POINT('Ctrl Pts',(207.994115449394,-11.0653905789061,-0.787617584544385));
#34689=CARTESIAN_POINT('Ctrl Pts',(208.050592353441,-10.7897081350621,-3.40582138748802));
#34690=CARTESIAN_POINT('Ctrl Pts',(208.146560308041,-8.74649764535955,-7.51345168544144));
#34691=CARTESIAN_POINT('Ctrl Pts',(208.265033459699,-4.11395673115298,-10.771654343876));
#34692=CARTESIAN_POINT('Ctrl Pts',(208.383506611358,1.51111850823841,-11.4310847317218));
#34693=CARTESIAN_POINT('Ctrl Pts',(208.501979763016,6.77162088338667,-9.33264849340337));
#34694=CARTESIAN_POINT('Ctrl Pts',(208.620452914674,10.3984001537186,-4.9826149292203));
#34695=CARTESIAN_POINT('Ctrl Pts',(208.738926066332,11.5164585613786,0.569525674392788));
#34696=CARTESIAN_POINT('Ctrl Pts',(208.857399217991,9.85605302940134,5.98426235816675));
#34697=CARTESIAN_POINT('Ctrl Pts',(208.975872369649,5.817773450173,9.95523427008149));
#34698=CARTESIAN_POINT('Ctrl Pts',(209.094345521308,0.375896258524645,11.5244036415153));
#34699=CARTESIAN_POINT('Ctrl Pts',(209.212818672966,-5.15666976717709,10.3131922411068));
#34700=CARTESIAN_POINT('Ctrl Pts',(209.331291824624,-9.44513623567911,6.61381726230806));
#34701=CARTESIAN_POINT('Ctrl Pts',(209.419395465602,-10.9396905378665,2.67612257791915));
#34702=CARTESIAN_POINT('Ctrl Pts',(209.468008056027,-11.0663840243592,0.423082087090511));
#34703=CARTESIAN_POINT('Ctrl Pts',(209.477129595899,-11.0659567005612,0.000279664497864693));
#34704=CARTESIAN_POINT('Ctrl Pts',(208.272870404101,-11.0658352981118,0.000279391217193198));
#34705=CARTESIAN_POINT('Ctrl Pts',(208.302389092482,-11.0644823738004,-1.36801666621322));
#34706=CARTESIAN_POINT('Ctrl Pts',(208.371398831416,-10.4696593756224,-4.56800686291313));
#34707=CARTESIAN_POINT('Ctrl Pts',(208.479899620902,-7.45982377135673,-8.79228111253593));
#34708=CARTESIAN_POINT('Ctrl Pts',(208.59837277256,-2.37359354017129,-11.2835823906954));
#34709=CARTESIAN_POINT('Ctrl Pts',(208.716845924218,3.28529051715118,-11.0526034977951));
#34710=CARTESIAN_POINT('Ctrl Pts',(208.835319075877,8.15156448652971,-8.15507046465587));
#34711=CARTESIAN_POINT('Ctrl Pts',(208.953792227535,11.0511897802984,-3.29004290266605));
#34712=CARTESIAN_POINT('Ctrl Pts',(209.072265379193,11.2846020076979,2.3687413090957));
#34713=CARTESIAN_POINT('Ctrl Pts',(209.190738530852,8.79548807096082,7.4560423453157));
#34714=CARTESIAN_POINT('Ctrl Pts',(209.30921168251,4.18437227866815,10.7444965677815));
#34715=CARTESIAN_POINT('Ctrl Pts',(209.427684834168,-1.43626631304541,11.4407306121404));
#34716=CARTESIAN_POINT('Ctrl Pts',(209.546157985827,-6.71039090158305,9.37677086258944));
#34717=CARTESIAN_POINT('Ctrl Pts',(209.661219842471,-10.2603183169951,5.17513671043559));
#34718=CARTESIAN_POINT('Ctrl Pts',(209.736790648562,-11.0655601973255,1.67189078030484));
#34719=CARTESIAN_POINT('Ctrl Pts',(209.772870404101,-11.0667065609126,-0.000153926678798932));
#34720=CARTESIAN_POINT('Origin',(201.227129595899,0.,0.));
#34721=CARTESIAN_POINT('',(206.477129595899,-11.0666876103725,-0.000161338566072536));
#34722=CARTESIAN_POINT('',(206.772870404101,-11.0651547064503,-0.000145660905285783));
#34723=CARTESIAN_POINT('',(201.227129595899,-11.06595,-5.55035408696717E-13));
#34724=CARTESIAN_POINT('Ctrl Pts',(206.477129595899,-11.0666876103725,-0.000161338566072901));
#34725=CARTESIAN_POINT('Ctrl Pts',(206.480731792208,-11.0668064580106,-0.167098809598976));
#34726=CARTESIAN_POINT('Ctrl Pts',(206.523825039069,-11.0225429972219,-2.16411670981007));
#34727=CARTESIAN_POINT('Ctrl Pts',(206.606409336483,-9.8807814135434,-5.94334383542404));
#34728=CARTESIAN_POINT('Ctrl Pts',(206.724882488141,-5.85900176316342,-9.93102591024465));
#34729=CARTESIAN_POINT('Ctrl Pts',(206.8433556398,-0.423677746264986,-11.5227459599084));
#34730=CARTESIAN_POINT('Ctrl Pts',(206.961828791458,5.11386287945728,-10.3344851705362));
#34731=CARTESIAN_POINT('Ctrl Pts',(207.080301943116,9.41763154941819,-6.65292366475841));
#34732=CARTESIAN_POINT('Ctrl Pts',(207.198775094774,11.4492998581925,-1.36627597758734));
#34733=CARTESIAN_POINT('Ctrl Pts',(207.317248246433,10.7187069544147,4.24999982531037));
#34734=CARTESIAN_POINT('Ctrl Pts',(207.435721398091,7.40211588169753,8.8409195089455));
#34735=CARTESIAN_POINT('Ctrl Pts',(207.554194549749,2.29968830857567,11.298876535884));
#34736=CARTESIAN_POINT('Ctrl Pts',(207.672667701408,-3.35756269431251,11.0308635221138));
#34737=CARTESIAN_POINT('Ctrl Pts',(207.791140853066,-8.20476720404479,8.10154136057916));
#34738=CARTESIAN_POINT('Ctrl Pts',(207.89262815123,-10.6613336413215,3.91785892862821));
#34739=CARTESIAN_POINT('Ctrl Pts',(207.954624398841,-11.0647241617092,1.04328002721838));
#34740=CARTESIAN_POINT('Ctrl Pts',(207.977129595899,-11.0651039401686,-0.000113627027167121));
#34741=CARTESIAN_POINT('Ctrl Pts',(206.772870404101,-11.0651547064503,-0.000145660905285783));
#34742=CARTESIAN_POINT('Ctrl Pts',(206.789005435296,-11.0655057942391,-0.748193683314034));
#34743=CARTESIAN_POINT('Ctrl Pts',(206.844631517043,-10.8077808658941,-3.32687665877076));
#34744=CARTESIAN_POINT('Ctrl Pts',(206.939748649344,-8.82632815191763,-7.41950869102601));
#34745=CARTESIAN_POINT('Ctrl Pts',(207.058221801002,-4.22888722542433,-10.7270541480969));
#34746=CARTESIAN_POINT('Ctrl Pts',(207.17669495266,1.3888161887093,-11.4465875899995));
#34747=CARTESIAN_POINT('Ctrl Pts',(207.295168104319,6.67145342963094,-9.40451418191398));
#34748=CARTESIAN_POINT('Ctrl Pts',(207.413641255977,10.3445339930023,-5.09350511231458));
#34749=CARTESIAN_POINT('Ctrl Pts',(207.532114407635,11.5218894583563,0.446364392591136));
#34750=CARTESIAN_POINT('Ctrl Pts',(207.650587559294,9.91947072438404,5.87854390216176));
#34751=CARTESIAN_POINT('Ctrl Pts',(207.769060710952,5.92387777273893,9.89246430345869));
#34752=CARTESIAN_POINT('Ctrl Pts',(207.88753386261,0.499088450816281,11.5197260635753));
#34753=CARTESIAN_POINT('Ctrl Pts',(208.006007014269,-5.04611108713692,10.3677355655817));
#34754=CARTESIAN_POINT('Ctrl Pts',(208.124480165927,-9.37388448524946,6.71442235183001));
#34755=CARTESIAN_POINT('Ctrl Pts',(208.213434629204,-10.9252921471334,2.75506174053056));
#34756=CARTESIAN_POINT('Ctrl Pts',(208.262898041929,-11.0662923594504,0.46253379991349));
#34757=CARTESIAN_POINT('Ctrl Pts',(208.272870404101,-11.0658352981118,0.000279391217193198));
#34758=CARTESIAN_POINT('Origin',(201.227129595899,0.,0.));
#34759=CARTESIAN_POINT('',(204.977129595899,-11.0658620952239,0.000280741946515456));
#34760=CARTESIAN_POINT('',(205.272870404101,-11.066766136903,-0.000127008754821079));
#34761=CARTESIAN_POINT('',(201.227129595899,-11.06595,-5.55035408696717E-13));
#34762=CARTESIAN_POINT('Ctrl Pts',(204.977129595899,-11.0658620952239,0.000280741946515339));
#34763=CARTESIAN_POINT('Ctrl Pts',(205.006839185574,-11.0644918505083,-1.37685467993411));
#34764=CARTESIAN_POINT('Ctrl Pts',(205.076039825802,-10.463984581982,-4.58569121052636));
#34765=CARTESIAN_POINT('Ctrl Pts',(205.184731516583,-7.43871005394589,-8.8101508004562));
#34766=CARTESIAN_POINT('Ctrl Pts',(205.303204668241,-2.34651819820973,-11.2892442895734));
#34767=CARTESIAN_POINT('Ctrl Pts',(205.4216778199,3.31179555484533,-11.0446903333316));
#34768=CARTESIAN_POINT('Ctrl Pts',(205.540150971558,8.17110447541142,-8.13549198319505));
#34769=CARTESIAN_POINT('Ctrl Pts',(205.658624123217,11.0590505604482,-3.26352232004452));
#34770=CARTESIAN_POINT('Ctrl Pts',(205.777097274875,11.2788870549277,2.39580548916746));
#34771=CARTESIAN_POINT('Ctrl Pts',(205.895570426533,8.777576190803,7.47712067870388));
#34772=CARTESIAN_POINT('Ctrl Pts',(206.014043578191,4.15858488930056,10.7545036577774));
#34773=CARTESIAN_POINT('Ctrl Pts',(206.13251672985,-1.46370773570288,11.4372521609064));
#34774=CARTESIAN_POINT('Ctrl Pts',(206.250989881508,-6.73286583398743,9.36064607483558));
#34775=CARTESIAN_POINT('Ctrl Pts',(206.365860836858,-10.2668305718026,5.15749310034477));
#34776=CARTESIAN_POINT('Ctrl Pts',(206.441240741655,-11.0655035256654,1.66304467597888));
#34777=CARTESIAN_POINT('Ctrl Pts',(206.477129595899,-11.0666876103725,-0.000161338566072901));
#34778=CARTESIAN_POINT('Ctrl Pts',(205.272870404101,-11.066766136903,-0.000127008754821131));
#34779=CARTESIAN_POINT('Ctrl Pts',(205.27562177811,-11.0668407583771,-0.127631986551504));
#34780=CARTESIAN_POINT('Ctrl Pts',(205.317864202671,-11.0337047479051,-2.08520391838922));
#34781=CARTESIAN_POINT('Ctrl Pts',(205.399597677786,-9.94376021587458,-5.83736334058754));
#34782=CARTESIAN_POINT('Ctrl Pts',(205.518070829444,-5.96484490322095,-9.86781652946403));
#34783=CARTESIAN_POINT('Ctrl Pts',(205.636543981102,-0.546849485135998,
-11.5175576204352));
#34784=CARTESIAN_POINT('Ctrl Pts',(205.755017132761,5.00307899201479,-10.3885696055));
#34785=CARTESIAN_POINT('Ctrl Pts',(205.873490284419,9.3459632629926,-6.75323245198365));
#34786=CARTESIAN_POINT('Ctrl Pts',(205.991963436077,11.4340378838074,-1.4886085900372));
#34787=CARTESIAN_POINT('Ctrl Pts',(206.110436587736,10.7635333998672,4.13515738637055));
#34788=CARTESIAN_POINT('Ctrl Pts',(206.228909739394,7.49621590665812,8.76127416208841));
#34789=CARTESIAN_POINT('Ctrl Pts',(206.347382891052,2.42035931523562,11.2736435390796));
#34790=CARTESIAN_POINT('Ctrl Pts',(206.46585604271,-3.23943382596151,11.0661305951517));
#34791=CARTESIAN_POINT('Ctrl Pts',(206.584329194369,-8.1176802770788,8.18879995973997));
#34792=CARTESIAN_POINT('Ctrl Pts',(206.686667314832,-10.639804868209,3.9967692784412));
#34793=CARTESIAN_POINT('Ctrl Pts',(206.749514384743,-11.0646464946538,1.08267989306887));
#34794=CARTESIAN_POINT('Ctrl Pts',(206.772870404101,-11.0651547064503,-0.000145660905285783));
#34795=CARTESIAN_POINT('Origin',(203.804782797639,0.,-4.68805434560642E-16));
#34796=CARTESIAN_POINT('',(204.,14.5,-1.77573785876366E-15));
#34797=CARTESIAN_POINT('Origin',(204.,0.,0.));
#34798=CARTESIAN_POINT('',(203.609565595278,15.3123475237772,1.87522173824257E-15));
#34799=CARTESIAN_POINT('',(203.804782797639,14.9061737618886,1.82547979850311E-15));
#34800=CARTESIAN_POINT('',(203.609565595278,-15.3123475237772,-1.87522173824257E-15));
#34801=CARTESIAN_POINT('Origin',(203.609565595278,0.,-9.37610869121283E-16));
#34802=CARTESIAN_POINT('Origin',(203.609565595278,0.,-9.37610869121283E-16));
#34803=CARTESIAN_POINT('Origin',(199.,0.,0.));
#34804=CARTESIAN_POINT('',(194.390434404722,-22.6876524762228,-2.77843609851737E-15));
#34805=CARTESIAN_POINT('',(199.,-19.,-2.32682891837997E-15));
#34806=CARTESIAN_POINT('',(194.390434404722,22.6876524762228,-2.77843609851737E-15));
#34807=CARTESIAN_POINT('Origin',(194.390434404722,0.,-1.38921804925869E-15));
#34808=CARTESIAN_POINT('Origin',(194.390434404722,0.,-1.38921804925869E-15));
#34809=CARTESIAN_POINT('Origin',(204.,12.,0.));
#34810=CARTESIAN_POINT('',(204.,6.4242839578383,-9.01020671414155));
#34811=CARTESIAN_POINT('Ctrl Pts',(204.,5.13002622089324,10.7654810839695));
#34812=CARTESIAN_POINT('Ctrl Pts',(204.,5.38136954563958,10.6351616725403));
#34813=CARTESIAN_POINT('Ctrl Pts',(204.,5.62773511945152,10.496037570914));
#34814=CARTESIAN_POINT('Ctrl Pts',(204.,5.86861265292755,10.3482717207313));
#34815=CARTESIAN_POINT('Ctrl Pts',(204.,5.94054489470907,10.3041450281793));
#34816=CARTESIAN_POINT('Ctrl Pts',(204.,6.01198756307411,10.2592473760111));
#34817=CARTESIAN_POINT('Ctrl Pts',(204.,6.08292661269302,10.2135823224016));
#34818=CARTESIAN_POINT('Ctrl Pts',(204.,6.32103183087106,10.0603086654917));
#34819=CARTESIAN_POINT('Ctrl Pts',(204.,6.55346587906383,9.89839258016546));
#34820=CARTESIAN_POINT('Ctrl Pts',(204.,6.77986031074224,9.72824991976574));
#34821=CARTESIAN_POINT('Ctrl Pts',(204.,6.94636210335151,9.60311849428924));
#34822=CARTESIAN_POINT('Ctrl Pts',(204.,7.1095965371914,9.47353648922993));
#34823=CARTESIAN_POINT('Ctrl Pts',(204.,7.26940436268983,9.3396565875382));
#34824=CARTESIAN_POINT('Ctrl Pts',(204.,7.35126323925222,9.27107885479835));
#34825=CARTESIAN_POINT('Ctrl Pts',(204.,7.43222284822467,9.20137326579582));
#34826=CARTESIAN_POINT('Ctrl Pts',(204.,7.51226055916463,9.13055939493385));
#34827=CARTESIAN_POINT('Ctrl Pts',(204.,7.55773359935015,9.09032683508698));
#34828=CARTESIAN_POINT('Ctrl Pts',(204.,7.60290904536994,9.04973652299996));
#34829=CARTESIAN_POINT('Ctrl Pts',(204.,7.6477826193096,9.00879196524232));
#34830=CARTESIAN_POINT('Ctrl Pts',(204.,7.67412699137662,8.98475423949447));
#34831=CARTESIAN_POINT('Ctrl Pts',(204.,7.70036463731238,8.96059682297449));
#34832=CARTESIAN_POINT('Ctrl Pts',(204.,7.72648757778976,8.93632726435297));
#34833=CARTESIAN_POINT('Ctrl Pts',(204.,7.93284762077082,8.74460814434789));
#34834=CARTESIAN_POINT('Ctrl Pts',(204.,8.13218640352905,8.54577234004366));
#34835=CARTESIAN_POINT('Ctrl Pts',(204.,8.32415293242165,8.34023927042099));
#34836=CARTESIAN_POINT('Ctrl Pts',(204.,8.51588514583175,8.13495707568082));
#34837=CARTESIAN_POINT('Ctrl Pts',(204.,8.70026349258579,7.92299346524614));
#34838=CARTESIAN_POINT('Ctrl Pts',(204.,8.87689960063644,7.70473209956972));
#34839=CARTESIAN_POINT('Ctrl Pts',(204.,9.05225022064303,7.48805915417246));
#34840=CARTESIAN_POINT('Ctrl Pts',(204.,9.21997123123925,7.2651792925663));
#34841=CARTESIAN_POINT('Ctrl Pts',(204.,9.3796390247399,7.03644147863572));
#34842=CARTESIAN_POINT('Ctrl Pts',(204.,9.43899734574093,6.95140559076701));
#34843=CARTESIAN_POINT('Ctrl Pts',(204.,9.49724219729021,6.86555986952368));
#34844=CARTESIAN_POINT('Ctrl Pts',(204.,9.55435010923125,6.77892151321272));
#34845=CARTESIAN_POINT('Ctrl Pts',(204.,9.58173223932997,6.73738011091989));
#34846=CARTESIAN_POINT('Ctrl Pts',(204.,9.60885297102288,6.69565647540693));
#34847=CARTESIAN_POINT('Ctrl Pts',(204.,9.63570963697724,6.65375247545265));
#34848=CARTESIAN_POINT('Ctrl Pts',(204.,9.65311703621794,6.62659200593547));
#34849=CARTESIAN_POINT('Ctrl Pts',(204.,9.67040803962745,6.59936427222682));
#34850=CARTESIAN_POINT('Ctrl Pts',(204.,9.68758144205299,6.57207101681937));
#34851=CARTESIAN_POINT('Ctrl Pts',(204.,9.80968961419899,6.37800757807052));
#34852=CARTESIAN_POINT('Ctrl Pts',(204.,9.92586564114257,6.18061434034615));
#34853=CARTESIAN_POINT('Ctrl Pts',(204.,10.0359210519606,5.98011103618573));
#34854=CARTESIAN_POINT('Ctrl Pts',(204.,10.169417593916,5.73690175136203));
#34855=CARTESIAN_POINT('Ctrl Pts',(204.,10.2939100827387,5.48911690808692));
#34856=CARTESIAN_POINT('Ctrl Pts',(204.,10.4093216513626,5.23730002890402));
#34857=CARTESIAN_POINT('Ctrl Pts',(204.,10.5254180230111,4.983988975761));
#34858=CARTESIAN_POINT('Ctrl Pts',(204.,10.6323255696679,4.72659728746502));
#34859=CARTESIAN_POINT('Ctrl Pts',(204.,10.729917585886,4.4656569428601));
#34860=CARTESIAN_POINT('Ctrl Pts',(204.,10.8274066332726,4.20499191506283));
#34861=CARTESIAN_POINT('Ctrl Pts',(204.,10.9155999298627,3.94078508903903));
#34862=CARTESIAN_POINT('Ctrl Pts',(204.,10.9943206955058,3.67355490271475));
#34863=CARTESIAN_POINT('Ctrl Pts',(204.,11.070722593291,3.41419648293933));
#34864=CARTESIAN_POINT('Ctrl Pts',(204.,11.1382016992343,3.15198962618184));
#34865=CARTESIAN_POINT('Ctrl Pts',(204.,11.1965490037965,2.88740594074757));
#34866=CARTESIAN_POINT('Ctrl Pts',(204.,11.2184292430073,2.78818705870972));
#34867=CARTESIAN_POINT('Ctrl Pts',(204.,11.239024842206,2.68863395369663));
#34868=CARTESIAN_POINT('Ctrl Pts',(204.,11.2583230272717,2.58877165055923));
#34869=CARTESIAN_POINT('Ctrl Pts',(204.,11.2646093596117,2.55624177152537));
#34870=CARTESIAN_POINT('Ctrl Pts',(204.,11.2707580139378,2.52367908422497));
#34871=CARTESIAN_POINT('Ctrl Pts',(204.,11.276768526349,2.49108445736322));
#34872=CARTESIAN_POINT('Ctrl Pts',(204.,11.2819534753436,2.46296680844873));
#34873=CARTESIAN_POINT('Ctrl Pts',(204.,11.2870354183249,2.43482633632079));
#34874=CARTESIAN_POINT('Ctrl Pts',(204.,11.2920119385415,2.40667621364387));
#34875=CARTESIAN_POINT('Ctrl Pts',(204.,11.3401602971382,2.13432080420421));
#34876=CARTESIAN_POINT('Ctrl Pts',(204.,11.3785026931062,1.86075051089294));
#34877=CARTESIAN_POINT('Ctrl Pts',(204.,11.4069431380994,1.58648424740416));
#34878=CARTESIAN_POINT('Ctrl Pts',(204.,11.4353262302546,1.31277106768745));
#34879=CARTESIAN_POINT('Ctrl Pts',(204.,11.4538473676115,1.03836410278021));
#34880=CARTESIAN_POINT('Ctrl Pts',(204.,11.4623602432515,0.763770255373622));
#34881=CARTESIAN_POINT('Ctrl Pts',(204.,11.4653760895116,0.666490221838948));
#34882=CARTESIAN_POINT('Ctrl Pts',(204.,11.4671353615187,0.569186696189433));
#34883=CARTESIAN_POINT('Ctrl Pts',(204.,11.4676299794862,0.471882172297525));
#34884=CARTESIAN_POINT('Ctrl Pts',(204.,11.4690308522032,0.196293209297684));
#34885=CARTESIAN_POINT('Ctrl Pts',(204.,11.4602910303519,-0.0793043509409153));
#34886=CARTESIAN_POINT('Ctrl Pts',(204.,11.4415458577,-0.354378400011464));
#34887=CARTESIAN_POINT('Ctrl Pts',(204.,11.4228350041333,-0.628948837304771));
#34888=CARTESIAN_POINT('Ctrl Pts',(204.,11.3941552173243,-0.902998297934441));
#34889=CARTESIAN_POINT('Ctrl Pts',(204.,11.355590982303,-1.17598467682026));
#34890=CARTESIAN_POINT('Ctrl Pts',(204.,11.3322925135319,-1.3409085919427));
#34891=CARTESIAN_POINT('Ctrl Pts',(204.,11.3053853286628,-1.50544419830023));
#34892=CARTESIAN_POINT('Ctrl Pts',(204.,11.2748795879635,-1.66946821774531));
#34893=CARTESIAN_POINT('Ctrl Pts',(204.,11.2605870333378,-1.74631677818365));
#34894=CARTESIAN_POINT('Ctrl Pts',(204.,11.2455044662696,-1.82305299259109));
#34895=CARTESIAN_POINT('Ctrl Pts',(204.,11.2296324649341,-1.89966391050251));
#34896=CARTESIAN_POINT('Ctrl Pts',(204.,11.2207832961272,-1.94237704608795));
#34897=CARTESIAN_POINT('Ctrl Pts',(204.,11.2116872345337,-1.98505777273071));
#34898=CARTESIAN_POINT('Ctrl Pts',(204.,11.2023523551507,-2.02766811322841));
#34899=CARTESIAN_POINT('Ctrl Pts',(204.,11.1437789246351,-2.29503459071588));
#34900=CARTESIAN_POINT('Ctrl Pts',(204.,11.0757667283023,-2.55984023401176));
#34901=CARTESIAN_POINT('Ctrl Pts',(204.,10.9984988879299,-2.82157931663494));
#34902=CARTESIAN_POINT('Ctrl Pts',(204.,10.9211642668246,-3.08354461404129));
#34903=CARTESIAN_POINT('Ctrl Pts',(204.,10.8345578076104,-3.34243866433772));
#34904=CARTESIAN_POINT('Ctrl Pts',(204.,10.738812096583,-3.59774315463838));
#34905=CARTESIAN_POINT('Ctrl Pts',(204.,10.6439399624884,-3.85071826526072));
#34906=CARTESIAN_POINT('Ctrl Pts',(204.,10.5400943383499,-4.10016957985931));
#34907=CARTESIAN_POINT('Ctrl Pts',(204.,10.4273575366565,-4.34557304492614));
#34908=CARTESIAN_POINT('Ctrl Pts',(204.,10.3326692805132,-4.55168875700633));
#34909=CARTESIAN_POINT('Ctrl Pts',(204.,10.2317079682769,-4.75494878389947));
#34910=CARTESIAN_POINT('Ctrl Pts',(204.,10.1244983728406,-4.95502732763819));
#34911=CARTESIAN_POINT('Ctrl Pts',(204.,10.015461477266,-5.15851604701587));
#34912=CARTESIAN_POINT('Ctrl Pts',(204.,9.89996122074432,-5.3587140873406));
#34913=CARTESIAN_POINT('Ctrl Pts',(204.,9.77819623555298,-5.55535964468922));
#34914=CARTESIAN_POINT('Ctrl Pts',(204.,9.72492405453176,-5.64139207602925));
#34915=CARTESIAN_POINT('Ctrl Pts',(204.,9.67045252598315,-5.72674429116772));
#34916=CARTESIAN_POINT('Ctrl Pts',(204.,9.61479723035913,-5.81139313701224));
#34917=CARTESIAN_POINT('Ctrl Pts',(204.,9.58095274764431,-5.86286885675988));
#34918=CARTESIAN_POINT('Ctrl Pts',(204.,9.54667050012853,-5.91408445789606));
#34919=CARTESIAN_POINT('Ctrl Pts',(204.,9.51195388615793,-5.96503458703567));
#34920=CARTESIAN_POINT('Ctrl Pts',(204.,9.49594011558806,-5.9885364089368));
#34921=CARTESIAN_POINT('Ctrl Pts',(204.,9.47983416005849,-6.01198133597758));
#34922=CARTESIAN_POINT('Ctrl Pts',(204.,9.46364417473069,-6.03535773337556));
#34923=CARTESIAN_POINT('Ctrl Pts',(204.,9.31055150742202,-6.25640518692579));
#34924=CARTESIAN_POINT('Ctrl Pts',(204.,9.14977308434649,-6.47158654910881));
#34925=CARTESIAN_POINT('Ctrl Pts',(204.,8.9817196830734,-6.68056443750362));
#34926=CARTESIAN_POINT('Ctrl Pts',(204.,8.81244499279347,-6.89106102409696));
#34927=CARTESIAN_POINT('Ctrl Pts',(204.,8.63578878909517,-7.0952641246414));
#34928=CARTESIAN_POINT('Ctrl Pts',(204.,8.45212755363202,-7.29279890909091));
#34929=CARTESIAN_POINT('Ctrl Pts',(204.,8.26882949894822,-7.48994307852151));
#34930=CARTESIAN_POINT('Ctrl Pts',(204.,8.07855362515398,-7.68044571246501));
#34931=CARTESIAN_POINT('Ctrl Pts',(204.,7.88163787795555,-7.86389759447329));
#34932=CARTESIAN_POINT('Ctrl Pts',(204.,7.6862339608845,-8.04594101582726));
#34933=CARTESIAN_POINT('Ctrl Pts',(204.,7.48429126870913,-8.22104191791924));
#34934=CARTESIAN_POINT('Ctrl Pts',(204.,7.27611121107159,-8.38875832568992));
#34935=CARTESIAN_POINT('Ctrl Pts',(204.,7.07157555393425,-8.5535386896949));
#34936=CARTESIAN_POINT('Ctrl Pts',(204.,6.86101854652668,-8.71119112116731));
#34937=CARTESIAN_POINT('Ctrl Pts',(204.,6.64470498300361,-8.86125088123046));
#34938=CARTESIAN_POINT('Ctrl Pts',(204.,6.57188067822712,-8.9117701252554));
#34939=CARTESIAN_POINT('Ctrl Pts',(204.,6.4984037733868,-8.96142840640969));
#34940=CARTESIAN_POINT('Ctrl Pts',(204.,6.42428395783811,-9.01020671414169));
#34941=CARTESIAN_POINT('',(204.,-6.42465676560637,-9.01028147758818));
#34942=CARTESIAN_POINT('Origin',(204.,0.,0.));
#34943=CARTESIAN_POINT('Ctrl Pts',(204.,-6.42465676560677,-9.01028147758789));
#34944=CARTESIAN_POINT('Ctrl Pts',(204.,-6.65054912801718,-8.86194699748741));
#34945=CARTESIAN_POINT('Ctrl Pts',(204.,-6.87070467837785,-8.70551035742835));
#34946=CARTESIAN_POINT('Ctrl Pts',(204.,-7.08464448205146,-8.54123692224679));
#34947=CARTESIAN_POINT('Ctrl Pts',(204.,-7.14173823356622,-8.49739755001365));
#34948=CARTESIAN_POINT('Ctrl Pts',(204.,-7.19838920257658,-8.45299978400815));
#34949=CARTESIAN_POINT('Ctrl Pts',(204.,-7.25458803292142,-8.40804809380943));
#34950=CARTESIAN_POINT('Ctrl Pts',(204.,-7.4639774887815,-8.24056400396366));
#34951=CARTESIAN_POINT('Ctrl Pts',(204.,-7.6670926166537,-8.06539371176003));
#34952=CARTESIAN_POINT('Ctrl Pts',(204.,-7.86365984101134,-7.88300433101605));
#34953=CARTESIAN_POINT('Ctrl Pts',(204.,-8.00894357130265,-7.74819950947673));
#34954=CARTESIAN_POINT('Ctrl Pts',(204.,-8.15064981364656,-7.6094500659697));
#34955=CARTESIAN_POINT('Ctrl Pts',(204.,-8.28865671380878,-7.46693033139527));
#34956=CARTESIAN_POINT('Ctrl Pts',(204.,-8.35438639477961,-7.39905128567645));
#34957=CARTESIAN_POINT('Ctrl Pts',(204.,-8.41927676170901,-7.33031681857506));
#34958=CARTESIAN_POINT('Ctrl Pts',(204.,-8.48331377713208,-7.26074491649885));
#34959=CARTESIAN_POINT('Ctrl Pts',(204.,-8.52430087856167,-7.21621519274132));
#34960=CARTESIAN_POINT('Ctrl Pts',(204.,-8.56493837736498,-7.17134238784771));
#34961=CARTESIAN_POINT('Ctrl Pts',(204.,-8.60522246310078,-7.12613111045349));
#34962=CARTESIAN_POINT('Ctrl Pts',(204.,-8.6307288154565,-7.09750504756524));
#34963=CARTESIAN_POINT('Ctrl Pts',(204.,-8.65608834062076,-7.06874902546348));
#34964=CARTESIAN_POINT('Ctrl Pts',(204.,-8.68129526525307,-7.03987015636087));
#34965=CARTESIAN_POINT('Ctrl Pts',(204.,-8.85913295253149,-6.83612648801025));
#34966=CARTESIAN_POINT('Ctrl Pts',(204.,-9.02945634830405,-6.62618328961249));
#34967=CARTESIAN_POINT('Ctrl Pts',(204.,-9.19199863370888,-6.41052061691195));
#34968=CARTESIAN_POINT('Ctrl Pts',(204.,-9.35567666968762,-6.1933510193907));
#34969=CARTESIAN_POINT('Ctrl Pts',(204.,-9.51146491604776,-5.97038128340569));
#34970=CARTESIAN_POINT('Ctrl Pts',(204.,-9.65905552542869,-5.74206275455145));
#34971=CARTESIAN_POINT('Ctrl Pts',(204.,-9.80619753499587,-5.51443819701386));
#34972=CARTESIAN_POINT('Ctrl Pts',(204.,-9.94519205346384,-5.28149679965102));
#34973=CARTESIAN_POINT('Ctrl Pts',(204.,-10.0756928459269,-5.04365469710717));
#34974=CARTESIAN_POINT('Ctrl Pts',(204.,-10.121650657997,-4.9598950321676));
#34975=CARTESIAN_POINT('Ctrl Pts',(204.,-10.1665546751333,-4.87552733484104));
#34976=CARTESIAN_POINT('Ctrl Pts',(204.,-10.2103884138121,-4.79056903948713));
#34977=CARTESIAN_POINT('Ctrl Pts',(204.,-10.2257962386725,-4.76070568366332));
#34978=CARTESIAN_POINT('Ctrl Pts',(204.,-10.2410718169294,-4.73076935251653));
#34979=CARTESIAN_POINT('Ctrl Pts',(204.,-10.2562144105126,-4.70076079351632));
#34980=CARTESIAN_POINT('Ctrl Pts',(204.,-10.2706014570784,-4.67224952605507));
#34981=CARTESIAN_POINT('Ctrl Pts',(204.,-10.284863946233,-4.6436819915071));
#34982=CARTESIAN_POINT('Ctrl Pts',(204.,-10.2990008454926,-4.61506022377236));
#34983=CARTESIAN_POINT('Ctrl Pts',(204.,-10.3969751316163,-4.41670008765512));
#34984=CARTESIAN_POINT('Ctrl Pts',(204.,-10.4889285784169,-4.21571654717207));
#34985=CARTESIAN_POINT('Ctrl Pts',(204.,-10.5747194144341,-4.01236004123072));
#34986=CARTESIAN_POINT('Ctrl Pts',(204.,-10.6797305993346,-3.76344408892707));
#34987=CARTESIAN_POINT('Ctrl Pts',(204.,-10.7755102375713,-3.51097344526088));
#34988=CARTESIAN_POINT('Ctrl Pts',(204.,-10.862082533099,-3.25549885901863));
#34989=CARTESIAN_POINT('Ctrl Pts',(204.,-10.9495611244006,-2.99734979664691));
#34990=CARTESIAN_POINT('Ctrl Pts',(204.,-11.0276387752821,-2.73613301072007));
#34991=CARTESIAN_POINT('Ctrl Pts',(204.,-11.0962936510127,-2.4723904858174));
#34992=CARTESIAN_POINT('Ctrl Pts',(204.,-11.1652522053208,-2.20748135833999));
#34993=CARTESIAN_POINT('Ctrl Pts',(204.,-11.224704598828,-1.9400234909498));
#34994=CARTESIAN_POINT('Ctrl Pts',(204.,-11.2745791857272,-1.67054859462426));
#34995=CARTESIAN_POINT('Ctrl Pts',(204.,-11.3233278278927,-1.40715723420891));
#34996=CARTESIAN_POINT('Ctrl Pts',(204.,-11.362926170186,-1.14183827806072));
#34997=CARTESIAN_POINT('Ctrl Pts',(204.,-11.3932597362624,-0.875080645215561));
#34998=CARTESIAN_POINT('Ctrl Pts',(204.,-11.4046348235411,-0.775046532898629));
#34999=CARTESIAN_POINT('Ctrl Pts',(204.,-11.4147065686262,-0.674810074975735));
#35000=CARTESIAN_POINT('Ctrl Pts',(204.,-11.4234671746766,-0.574397033518757));
#35001=CARTESIAN_POINT('Ctrl Pts',(204.,-11.4262148823748,-0.542903129396417));
#35002=CARTESIAN_POINT('Ctrl Pts',(204.,-11.4288336031237,-0.511391854752237));
#35003=CARTESIAN_POINT('Ctrl Pts',(204.,-11.4313230765255,-0.479864005876946));
#35004=CARTESIAN_POINT('Ctrl Pts',(204.,-11.4334153680567,-0.453366252918575));
#35005=CARTESIAN_POINT('Ctrl Pts',(204.,-11.4354160841983,-0.426860091688597));
#35006=CARTESIAN_POINT('Ctrl Pts',(204.,-11.4373246045135,-0.400354135471182));
#35007=CARTESIAN_POINT('Ctrl Pts',(204.,-11.4571851542671,-0.124526386594492));
#35008=CARTESIAN_POINT('Ctrl Pts',(204.,-11.467086561415,0.151537388123827));
#35009=CARTESIAN_POINT('Ctrl Pts',(204.,-11.4670322276902,0.427285070384512));
#35010=CARTESIAN_POINT('Ctrl Pts',(204.,-11.4669776265041,0.704390139058355));
#35011=CARTESIAN_POINT('Ctrl Pts',(204.,-11.4568691710756,0.98117661984866));
#35012=CARTESIAN_POINT('Ctrl Pts',(204.,-11.4366600361361,1.25709887328326));
#35013=CARTESIAN_POINT('Ctrl Pts',(204.,-11.4298934228941,1.34948576561938));
#35014=CARTESIAN_POINT('Ctrl Pts',(204.,-11.4219939898967,1.44177584848161));
#35015=CARTESIAN_POINT('Ctrl Pts',(204.,-11.412958684684,1.53394881608885));
#35016=CARTESIAN_POINT('Ctrl Pts',(204.,-11.3860912032069,1.80803535124878));
#35017=CARTESIAN_POINT('Ctrl Pts',(204.,-11.3491838657346,2.08108650375856));
#35018=CARTESIAN_POINT('Ctrl Pts',(204.,-11.3024701946929,2.35261240030303));
#35019=CARTESIAN_POINT('Ctrl Pts',(204.,-11.2555816827369,2.62515456970653));
#35020=CARTESIAN_POINT('Ctrl Pts',(204.,-11.1988131424943,2.89616064928337));
#35021=CARTESIAN_POINT('Ctrl Pts',(204.,-11.1323486392896,3.16512786231975));
#35022=CARTESIAN_POINT('Ctrl Pts',(204.,-11.0912368266875,3.33149831760495));
#35023=CARTESIAN_POINT('Ctrl Pts',(204.,-11.0464142478112,3.49708850676293));
#35024=CARTESIAN_POINT('Ctrl Pts',(204.,-10.997914928214,3.66177647998853));
#35025=CARTESIAN_POINT('Ctrl Pts',(204.,-10.9753867054638,3.73827502421373));
#35026=CARTESIAN_POINT('Ctrl Pts',(204.,-10.9520650672135,3.81457886186982));
#35027=CARTESIAN_POINT('Ctrl Pts',(204.,-10.9279529066472,3.89067554151667));
#35028=CARTESIAN_POINT('Ctrl Pts',(204.,-10.9143162205251,3.93371218820865));
#35029=CARTESIAN_POINT('Ctrl Pts',(204.,-10.9004243749725,3.97668935780195));
#35030=CARTESIAN_POINT('Ctrl Pts',(204.,-10.8862900827949,4.01956828440585));
#35031=CARTESIAN_POINT('Ctrl Pts',(204.,-10.798911086603,4.28464824153112));
#35032=CARTESIAN_POINT('Ctrl Pts',(204.,-10.702209612138,4.54617686608043));
#35033=CARTESIAN_POINT('Ctrl Pts',(204.,-10.5964725843817,4.80366716089838));
#35034=CARTESIAN_POINT('Ctrl Pts',(204.,-10.4901388166223,5.06261063406443));
#35035=CARTESIAN_POINT('Ctrl Pts',(204.,-10.3746670590857,5.31747067532474));
#35036=CARTESIAN_POINT('Ctrl Pts',(204.,-10.2502963436619,5.56774633407479));
#35037=CARTESIAN_POINT('Ctrl Pts',(204.,-10.1261430056542,5.8175845564411));
#35038=CARTESIAN_POINT('Ctrl Pts',(204.,-9.99312157354115,6.06285500942485));
#35039=CARTESIAN_POINT('Ctrl Pts',(204.,-9.85142032185599,6.30304466996495));
#35040=CARTESIAN_POINT('Ctrl Pts',(204.,-9.73102700503411,6.50711647282378));
#35041=CARTESIAN_POINT('Ctrl Pts',(204.,-9.60436711932939,6.70752057533099));
#35042=CARTESIAN_POINT('Ctrl Pts',(204.,-9.47152968713627,6.90392906505641));
#35043=CARTESIAN_POINT('Ctrl Pts',(204.,-9.33469133475788,7.10625316665515));
#35044=CARTESIAN_POINT('Ctrl Pts',(204.,-9.19129761317494,7.30433764131528));
#35045=CARTESIAN_POINT('Ctrl Pts',(204.,-9.04161060192979,7.49794996228298));
#35046=CARTESIAN_POINT('Ctrl Pts',(204.,-8.97612253451004,7.58265535270634));
#35047=CARTESIAN_POINT('Ctrl Pts',(204.,-8.90942958866847,7.66650449296753));
#35048=CARTESIAN_POINT('Ctrl Pts',(204.,-8.84155236887728,7.74947665964046));
#35049=CARTESIAN_POINT('Ctrl Pts',(204.,-8.79958392576119,7.80077829909983));
#35050=CARTESIAN_POINT('Ctrl Pts',(204.,-8.75716272620976,7.85174466108664));
#35051=CARTESIAN_POINT('Ctrl Pts',(204.,-8.71429349733821,7.90237068802365));
#35052=CARTESIAN_POINT('Ctrl Pts',(204.,-8.69465601284209,7.92556139719303));
#35053=CARTESIAN_POINT('Ctrl Pts',(204.,-8.67492989531673,7.94867431658233));
#35054=CARTESIAN_POINT('Ctrl Pts',(204.,-8.65511880737665,7.97170556570952));
#35055=CARTESIAN_POINT('Ctrl Pts',(204.,-8.47328695105665,8.18309298647266));
#35056=CARTESIAN_POINT('Ctrl Pts',(204.,-8.28422016552803,8.38769783304993));
#35057=CARTESIAN_POINT('Ctrl Pts',(204.,-8.08840339292777,8.58524924614487));
#35058=CARTESIAN_POINT('Ctrl Pts',(204.,-7.89034148593488,8.78506568212811));
#35059=CARTESIAN_POINT('Ctrl Pts',(204.,-7.68537355787534,8.97766647086422));
#35060=CARTESIAN_POINT('Ctrl Pts',(204.,-7.47395492068874,9.16274545557204));
#35061=CARTESIAN_POINT('Ctrl Pts',(204.,-7.26126910103603,9.34893375044942));
#35062=CARTESIAN_POINT('Ctrl Pts',(204.,-7.04205459398052,9.52751026475814));
#35063=CARTESIAN_POINT('Ctrl Pts',(204.,-6.81673413565081,9.69813036804369));
#35064=CARTESIAN_POINT('Ctrl Pts',(204.,-6.5921607892943,9.86818473343318));
#35065=CARTESIAN_POINT('Ctrl Pts',(204.,-6.36152144411965,10.0303357784069));
#35066=CARTESIAN_POINT('Ctrl Pts',(204.,-6.12520100238345,10.1842031840316));
#35067=CARTESIAN_POINT('Ctrl Pts',(204.,-5.8919943458718,10.3360432150853));
#35068=CARTESIAN_POINT('Ctrl Pts',(204.,-5.65325482885913,10.4798167914932));
#35069=CARTESIAN_POINT('Ctrl Pts',(204.,-5.40932671028307,10.6151148681509));
#35070=CARTESIAN_POINT('Ctrl Pts',(204.,-5.31683948747285,10.6664141748265));
#35071=CARTESIAN_POINT('Ctrl Pts',(204.,-5.22360612044888,10.7164945619684));
#35072=CARTESIAN_POINT('Ctrl Pts',(204.,-5.12964461189203,10.7653319110786));
#35073=CARTESIAN_POINT('Origin',(193.945217202361,0.,-6.94609024629344E-16));
#35074=CARTESIAN_POINT('',(193.5,23.,2.81668763803891E-15));
#35075=CARTESIAN_POINT('',(193.945217202361,22.8438262381114,2.79756186827814E-15));
#35076=CARTESIAN_POINT('',(193.5,-23.,-2.81668763803891E-15));
#35077=CARTESIAN_POINT('Origin',(193.5,0.,0.));
#35078=CARTESIAN_POINT('Origin',(193.5,0.,0.));
#35079=CARTESIAN_POINT('Origin',(172.4,0.,0.));
#35080=CARTESIAN_POINT('',(150.8,-23.,-2.81668763803891E-15));
#35081=CARTESIAN_POINT('',(172.4,-23.,-2.81668763803891E-15));
#35082=CARTESIAN_POINT('Origin',(150.8,0.,0.));
#35083=CARTESIAN_POINT('Origin',(221.275,1.39622887047493E-15,0.));
#35084=CARTESIAN_POINT('',(221.275,-3.97626028075622,-11.2425521648637));
#35085=CARTESIAN_POINT('Ctrl Pts',(221.275,-7.33129268303527,8.28936271098428));
#35086=CARTESIAN_POINT('Ctrl Pts',(221.275,-7.54044240726459,8.11822864204739));
#35087=CARTESIAN_POINT('Ctrl Pts',(221.275,-7.74303984010792,7.93963645727318));
#35088=CARTESIAN_POINT('Ctrl Pts',(221.275,-7.9386364087855,7.75390012992646));
#35089=CARTESIAN_POINT('Ctrl Pts',(221.275,-7.99083493314403,7.70433299143922));
#35090=CARTESIAN_POINT('Ctrl Pts',(221.275,-8.0425347325609,7.65425680143036));
#35091=CARTESIAN_POINT('Ctrl Pts',(221.275,-8.09372696932752,7.60367698297605));
#35092=CARTESIAN_POINT('Ctrl Pts',(221.275,-8.2844625113853,7.41522323101266));
#35093=CARTESIAN_POINT('Ctrl Pts',(221.275,-8.46815467022213,7.21978122775128));
#35094=CARTESIAN_POINT('Ctrl Pts',(221.275,-8.64458019562942,7.01784412483079));
#35095=CARTESIAN_POINT('Ctrl Pts',(221.275,-8.77497710607317,6.86859149109764));
#35096=CARTESIAN_POINT('Ctrl Pts',(221.275,-8.90140380117501,6.71578979350078));
#35097=CARTESIAN_POINT('Ctrl Pts',(221.275,-9.02375731675049,6.55962514529613));
#35098=CARTESIAN_POINT('Ctrl Pts',(221.275,-9.08203163297198,6.48524732256424));
#35099=CARTESIAN_POINT('Ctrl Pts',(221.275,-9.13938181707504,6.41010649667514));
#35100=CARTESIAN_POINT('Ctrl Pts',(221.275,-9.19579578858202,6.33422202283415));
#35101=CARTESIAN_POINT('Ctrl Pts',(221.275,-9.2319037344147,6.28565191869511));
#35102=CARTESIAN_POINT('Ctrl Pts',(221.275,-9.26762813104671,6.23677715628016));
#35103=CARTESIAN_POINT('Ctrl Pts',(221.275,-9.3029656706437,6.18760271728134));
#35104=CARTESIAN_POINT('Ctrl Pts',(221.275,-9.32534005840804,6.15646733041508));
#35105=CARTESIAN_POINT('Ctrl Pts',(221.275,-9.34755483887619,6.12521804388268));
#35106=CARTESIAN_POINT('Ctrl Pts',(221.275,-9.36960501376276,6.0938625344152));
#35107=CARTESIAN_POINT('Ctrl Pts',(221.275,-9.52517147372286,5.87264589403949));
#35108=CARTESIAN_POINT('Ctrl Pts',(221.275,-9.67261677905937,5.64604914273315));
#35109=CARTESIAN_POINT('Ctrl Pts',(221.275,-9.81172575201428,5.41457759690167));
#35110=CARTESIAN_POINT('Ctrl Pts',(221.275,-9.95180673910459,5.18148865997232));
#35111=CARTESIAN_POINT('Ctrl Pts',(221.275,-10.0834348779947,4.94345606619207));
#35112=CARTESIAN_POINT('Ctrl Pts',(221.275,-10.2063511861488,4.70096086776407));
#35113=CARTESIAN_POINT('Ctrl Pts',(221.275,-10.3288938920592,4.45920272979267));
#35114=CARTESIAN_POINT('Ctrl Pts',(221.275,-10.4427779783649,4.2130085234756));
#35115=CARTESIAN_POINT('Ctrl Pts',(221.275,-10.5477026047267,3.96282829554833));
#35116=CARTESIAN_POINT('Ctrl Pts',(221.275,-10.5846533860096,3.87472357500786));
#35117=CARTESIAN_POINT('Ctrl Pts',(221.275,-10.6204925884416,3.78612430462181));
#35118=CARTESIAN_POINT('Ctrl Pts',(221.275,-10.6552056411817,3.69704954625496));
#35119=CARTESIAN_POINT('Ctrl Pts',(221.275,-10.6674074915966,3.6657392237237));
#35120=CARTESIAN_POINT('Ctrl Pts',(221.275,-10.6794701918223,3.63437014916719));
#35121=CARTESIAN_POINT('Ctrl Pts',(221.275,-10.6913930859635,3.60294314311006));
#35122=CARTESIAN_POINT('Ctrl Pts',(221.275,-10.7027210784224,3.57308421092436));
#35123=CARTESIAN_POINT('Ctrl Pts',(221.275,-10.7139193143212,3.54318233971434));
#35124=CARTESIAN_POINT('Ctrl Pts',(221.275,-10.7249869794359,3.51323966015309));
#35125=CARTESIAN_POINT('Ctrl Pts',(221.275,-10.8016902710256,3.30572506176606));
#35126=CARTESIAN_POINT('Ctrl Pts',(221.275,-10.8721314855905,3.09623078013545));
#35127=CARTESIAN_POINT('Ctrl Pts',(221.275,-10.9361958062775,2.88502070154648));
#35128=CARTESIAN_POINT('Ctrl Pts',(221.275,-11.0146129270476,2.62649167848104));
#35129=CARTESIAN_POINT('Ctrl Pts',(221.275,-11.0834775056231,2.36539239768169));
#35130=CARTESIAN_POINT('Ctrl Pts',(221.275,-11.1428711824738,2.1022680602064));
#35131=CARTESIAN_POINT('Ctrl Pts',(221.275,-11.2028866308757,1.83638916641912));
#35132=CARTESIAN_POINT('Ctrl Pts',(221.275,-11.2532319736341,1.5684420208977));
#35133=CARTESIAN_POINT('Ctrl Pts',(221.275,-11.2939421486287,1.2989679208318));
#35134=CARTESIAN_POINT('Ctrl Pts',(221.275,-11.3348323955048,1.02830186548141));
#35135=CARTESIAN_POINT('Ctrl Pts',(221.275,-11.3660021414784,0.756094696820204));
#35136=CARTESIAN_POINT('Ctrl Pts',(221.275,-11.3874357123412,0.48288270138544));
#35137=CARTESIAN_POINT('Ctrl Pts',(221.275,-11.4083854089844,0.21583861151868));
#35138=CARTESIAN_POINT('Ctrl Pts',(221.275,-11.4200334438198,-0.0521660484121864));
#35139=CARTESIAN_POINT('Ctrl Pts',(221.275,-11.4223170737475,-0.320633072357773));
#35140=CARTESIAN_POINT('Ctrl Pts',(221.275,-11.4231734349703,-0.421308206337368));
#35141=CARTESIAN_POINT('Ctrl Pts',(221.275,-11.422712443048,-0.52204834128742));
#35142=CARTESIAN_POINT('Ctrl Pts',(221.275,-11.4209290367306,-0.622827041307124));
#35143=CARTESIAN_POINT('Ctrl Pts',(221.275,-11.4203696826865,-0.654435639336831));
#35144=CARTESIAN_POINT('Ctrl Pts',(221.275,-11.4196802325306,-0.686048029947425));
#35145=CARTESIAN_POINT('Ctrl Pts',(221.275,-11.4188605105267,-0.717663393991851));
#35146=CARTESIAN_POINT('Ctrl Pts',(221.275,-11.4181715705133,-0.744234706244506));
#35147=CARTESIAN_POINT('Ctrl Pts',(221.275,-11.4173906777833,-0.770804808474893));
#35148=CARTESIAN_POINT('Ctrl Pts',(221.275,-11.4165181156319,-0.797365069739118));
#35149=CARTESIAN_POINT('Ctrl Pts',(221.275,-11.4074380154237,-1.07375779827223));
#35150=CARTESIAN_POINT('Ctrl Pts',(221.275,-11.3884286589653,-1.34934424762446));
#35151=CARTESIAN_POINT('Ctrl Pts',(221.275,-11.3595511416112,-1.62357568033119));
#35152=CARTESIAN_POINT('Ctrl Pts',(221.275,-11.3305314725491,-1.89915703748129));
#35153=CARTESIAN_POINT('Ctrl Pts',(221.275,-11.2915463274116,-2.17337064059582));
#35154=CARTESIAN_POINT('Ctrl Pts',(221.275,-11.2426061724809,-2.44566894539353));
#35155=CARTESIAN_POINT('Ctrl Pts',(221.275,-11.2262195730029,-2.53684240542007));
#35156=CARTESIAN_POINT('Ctrl Pts',(221.275,-11.2087164795845,-2.62780117488787));
#35157=CARTESIAN_POINT('Ctrl Pts',(221.275,-11.1900959790274,-2.71852474022907));
#35158=CARTESIAN_POINT('Ctrl Pts',(221.275,-11.1347258388575,-2.98830140462323));
#35159=CARTESIAN_POINT('Ctrl Pts',(221.275,-11.0694790694482,-3.25599891097075));
#35160=CARTESIAN_POINT('Ctrl Pts',(221.275,-10.9946391192961,-3.52115447789874));
#35161=CARTESIAN_POINT('Ctrl Pts',(221.275,-10.9195190595718,-3.7873024641462));
#35162=CARTESIAN_POINT('Ctrl Pts',(221.275,-10.8347336613073,-4.05089003348519));
#35163=CARTESIAN_POINT('Ctrl Pts',(221.275,-10.7405185355667,-4.31143640220764));
#35164=CARTESIAN_POINT('Ctrl Pts',(221.275,-10.6822414940986,-4.47259812029723));
#35165=CARTESIAN_POINT('Ctrl Pts',(221.275,-10.6203555744656,-4.63259596628076));
#35166=CARTESIAN_POINT('Ctrl Pts',(221.275,-10.5549073629548,-4.79131221473031));
#35167=CARTESIAN_POINT('Ctrl Pts',(221.275,-10.5245062780325,-4.86503685954903));
#35168=CARTESIAN_POINT('Ctrl Pts',(221.275,-10.4933364763593,-4.93848492990648));
#35169=CARTESIAN_POINT('Ctrl Pts',(221.275,-10.4614021367911,-5.01164434495921));
#35170=CARTESIAN_POINT('Ctrl Pts',(221.275,-10.4433416048742,-5.05301980374264));
#35171=CARTESIAN_POINT('Ctrl Pts',(221.275,-10.4250335284866,-5.09430943985858));
#35172=CARTESIAN_POINT('Ctrl Pts',(221.275,-10.4064946029195,-5.13547602864041));
#35173=CARTESIAN_POINT('Ctrl Pts',(221.275,-10.2918858808873,-5.38997028795609));
#35174=CARTESIAN_POINT('Ctrl Pts',(221.275,-10.1683769645976,-5.63995820398864));
#35175=CARTESIAN_POINT('Ctrl Pts',(221.275,-10.0363041119217,-5.88498543783887));
#35176=CARTESIAN_POINT('Ctrl Pts',(221.275,-9.90348589380986,-6.13139550568774));
#35177=CARTESIAN_POINT('Ctrl Pts',(221.275,-9.76200657895998,-6.37278932900673));
#35178=CARTESIAN_POINT('Ctrl Pts',(221.275,-9.61215625301232,-6.60869368572787));
#35179=CARTESIAN_POINT('Ctrl Pts',(221.275,-9.46256785038424,-6.84418570532644));
#35180=CARTESIAN_POINT('Ctrl Pts',(221.275,-9.30463739618173,-7.07420800749294));
#35181=CARTESIAN_POINT('Ctrl Pts',(221.275,-9.13860575860143,-7.29827005837135));
#35182=CARTESIAN_POINT('Ctrl Pts',(221.275,-8.99754065062552,-7.48863942327735));
#35183=CARTESIAN_POINT('Ctrl Pts',(221.275,-8.85062667997815,-7.67470614113694));
#35184=CARTESIAN_POINT('Ctrl Pts',(221.275,-8.69798665733386,-7.85615340033203));
#35185=CARTESIAN_POINT('Ctrl Pts',(221.275,-8.54074929178595,-8.04306564344805));
#35186=CARTESIAN_POINT('Ctrl Pts',(221.275,-8.37743562834725,-8.22507625757405));
#35187=CARTESIAN_POINT('Ctrl Pts',(221.275,-8.20833061687298,-8.40198138569603));
#35188=CARTESIAN_POINT('Ctrl Pts',(221.275,-8.13434717435299,-8.4793773792494));
#35189=CARTESIAN_POINT('Ctrl Pts',(221.275,-8.05925495617845,-8.55579586853935));
#35190=CARTESIAN_POINT('Ctrl Pts',(221.275,-7.98307662016529,-8.6312183975156));
#35191=CARTESIAN_POINT('Ctrl Pts',(221.275,-7.93597560161412,-8.67785210103825));
#35192=CARTESIAN_POINT('Ctrl Pts',(221.275,-7.88845935284263,-8.72410503762538));
#35193=CARTESIAN_POINT('Ctrl Pts',(221.275,-7.84053310373852,-8.76997267154632));
#35194=CARTESIAN_POINT('Ctrl Pts',(221.275,-7.81857910575888,-8.79098366158319));
#35195=CARTESIAN_POINT('Ctrl Pts',(221.275,-7.7965450915264,-8.81190802326766));
#35196=CARTESIAN_POINT('Ctrl Pts',(221.275,-7.77443510921182,-8.83274228022652));
#35197=CARTESIAN_POINT('Ctrl Pts',(221.275,-7.571503372549,-9.02396504497532));
#35198=CARTESIAN_POINT('Ctrl Pts',(221.275,-7.36208531361138,-9.2076861345953));
#35199=CARTESIAN_POINT('Ctrl Pts',(221.275,-7.14669153075602,-9.3836868656952));
#35200=CARTESIAN_POINT('Ctrl Pts',(221.275,-6.9288281416759,-9.56170554037418));
#35201=CARTESIAN_POINT('Ctrl Pts',(221.275,-6.70485080477499,-9.73182622056391));
#35202=CARTESIAN_POINT('Ctrl Pts',(221.275,-6.47524434022513,-9.89379202155816));
#35203=CARTESIAN_POINT('Ctrl Pts',(221.275,-6.24426165088319,-10.0567286199175));
#35204=CARTESIAN_POINT('Ctrl Pts',(221.275,-6.00758168644788,-10.2114127023956));
#35205=CARTESIAN_POINT('Ctrl Pts',(221.275,-5.76566089151908,-10.3575457161937));
#35206=CARTESIAN_POINT('Ctrl Pts',(221.275,-5.52454223046687,-10.5031941985115));
#35207=CARTESIAN_POINT('Ctrl Pts',(221.275,-5.27821692212139,-10.6403485865904));
#35208=CARTESIAN_POINT('Ctrl Pts',(221.275,-5.02710751503102,-10.7686708798398));
#35209=CARTESIAN_POINT('Ctrl Pts',(221.275,-4.7793067248221,-10.8953023988939));
#35210=CARTESIAN_POINT('Ctrl Pts',(221.275,-4.52684655678323,-11.0133333108478));
#35211=CARTESIAN_POINT('Ctrl Pts',(221.275,-4.27011214160444,-11.1223927977311));
#35212=CARTESIAN_POINT('Ctrl Pts',(221.275,-4.17276935738525,-11.1637435223363));
#35213=CARTESIAN_POINT('Ctrl Pts',(221.275,-4.07481192872072,-11.2038040128707));
#35214=CARTESIAN_POINT('Ctrl Pts',(221.275,-3.97626028075543,-11.2425521648639));
#35215=CARTESIAN_POINT('',(221.275,-11.925,-1.46039130798322E-15));
#35216=CARTESIAN_POINT('Origin',(221.275,0.,0.));
#35217=CARTESIAN_POINT('',(221.275,6.22722261202592,-10.1702729013571));
#35218=CARTESIAN_POINT('Origin',(221.275,0.,0.));
#35219=CARTESIAN_POINT('Ctrl Pts',(221.275,6.22722261202635,-10.1702729013569));
#35220=CARTESIAN_POINT('Ctrl Pts',(221.275,6.46356696607157,-10.0143948603033));
#35221=CARTESIAN_POINT('Ctrl Pts',(221.275,6.6940404968013,-9.85028067913405));
#35222=CARTESIAN_POINT('Ctrl Pts',(221.275,6.91815274221079,-9.67814574681644));
#35223=CARTESIAN_POINT('Ctrl Pts',(221.275,6.98507843449569,-9.62674181977657));
#35224=CARTESIAN_POINT('Ctrl Pts',(221.275,7.05143664808183,-9.57462233097456));
#35225=CARTESIAN_POINT('Ctrl Pts',(221.275,7.11721378651107,-9.52179228723434));
#35226=CARTESIAN_POINT('Ctrl Pts',(221.275,7.33799317947798,-9.34446950813644));
#35227=CARTESIAN_POINT('Ctrl Pts',(221.275,7.55222908968855,-9.15914444417878));
#35228=CARTESIAN_POINT('Ctrl Pts',(221.275,7.75959855762187,-8.96626918346592));
#35229=CARTESIAN_POINT('Ctrl Pts',(221.275,7.91210843984702,-8.82441906643268));
#35230=CARTESIAN_POINT('Ctrl Pts',(221.275,8.06090364990992,-8.67848428279718));
#35231=CARTESIAN_POINT('Ctrl Pts',(221.275,8.20584177038155,-8.5286333250904));
#35232=CARTESIAN_POINT('Ctrl Pts',(221.275,8.28008388987517,-8.45187468718273));
#35233=CARTESIAN_POINT('Ctrl Pts',(221.275,8.35331377497516,-8.37408837062628));
#35234=CARTESIAN_POINT('Ctrl Pts',(221.275,8.42551096529891,-8.29529620810303));
#35235=CARTESIAN_POINT('Ctrl Pts',(221.275,8.46652945203915,-8.25053081959966));
#35236=CARTESIAN_POINT('Ctrl Pts',(221.275,8.50721457956437,-8.20544074571969));
#35237=CARTESIAN_POINT('Ctrl Pts',(221.275,8.54756245993294,-8.16002992098362));
#35238=CARTESIAN_POINT('Ctrl Pts',(221.275,8.57124988608984,-8.13337014238227));
#35239=CARTESIAN_POINT('Ctrl Pts',(221.275,8.59481865970039,-8.10660248462503));
#35240=CARTESIAN_POINT('Ctrl Pts',(221.275,8.61826163420111,-8.07973528909513));
#35241=CARTESIAN_POINT('Ctrl Pts',(221.275,8.80345110972847,-7.86749593146063));
#35242=CARTESIAN_POINT('Ctrl Pts',(221.275,8.98091389215197,-7.64891279700364));
#35243=CARTESIAN_POINT('Ctrl Pts',(221.275,9.15034475193748,-7.42443969561466));
#35244=CARTESIAN_POINT('Ctrl Pts',(221.275,9.31956880282469,-7.20024058820088));
#35245=CARTESIAN_POINT('Ctrl Pts',(221.275,9.48078087434829,-6.97016535470833));
#35246=CARTESIAN_POINT('Ctrl Pts',(221.275,9.63363482555217,-6.73463614949089));
#35247=CARTESIAN_POINT('Ctrl Pts',(221.275,9.7853763664071,-6.50082103228556));
#35248=CARTESIAN_POINT('Ctrl Pts',(221.275,9.92888129444408,-6.26163051176708));
#35249=CARTESIAN_POINT('Ctrl Pts',(221.275,10.0637647993104,-6.01745591892541));
#35250=CARTESIAN_POINT('Ctrl Pts',(221.275,10.1139092789555,-5.92668123218567));
#35251=CARTESIAN_POINT('Ctrl Pts',(221.275,10.1628617382439,-5.83521753754474));
#35252=CARTESIAN_POINT('Ctrl Pts',(221.275,10.2106006333088,-5.74308439237998));
#35253=CARTESIAN_POINT('Ctrl Pts',(221.275,10.2334904992998,-5.69890835220816));
#35254=CARTESIAN_POINT('Ctrl Pts',(221.275,10.2561013503811,-5.65457840069286));
#35255=CARTESIAN_POINT('Ctrl Pts',(221.275,10.2784307291743,-5.61009667518484));
#35256=CARTESIAN_POINT('Ctrl Pts',(221.275,10.2929037296767,-5.58126541921545));
#35257=CARTESIAN_POINT('Ctrl Pts',(221.275,10.3072539409162,-5.55237943416662));
#35258=CARTESIAN_POINT('Ctrl Pts',(221.275,10.3214803464741,-5.52344057897386));
#35259=CARTESIAN_POINT('Ctrl Pts',(221.275,10.4226344459013,-5.31767645791328));
#35260=CARTESIAN_POINT('Ctrl Pts',(221.275,10.5175408384123,-5.10922085610939));
#35261=CARTESIAN_POINT('Ctrl Pts',(221.275,10.606035053905,-4.89831200280797));
#35262=CARTESIAN_POINT('Ctrl Pts',(221.275,10.7133779963714,-4.64248085294634));
#35263=CARTESIAN_POINT('Ctrl Pts',(221.275,10.8112879352375,-4.38304038856547));
#35264=CARTESIAN_POINT('Ctrl Pts',(221.275,10.8997452377967,-4.12053919019108));
#35265=CARTESIAN_POINT('Ctrl Pts',(221.275,10.9887274077414,-3.85648042320802));
#35266=CARTESIAN_POINT('Ctrl Pts',(221.275,11.0681445478099,-3.58932386836834));
#35267=CARTESIAN_POINT('Ctrl Pts',(221.275,11.1379262532868,-3.31961183526273));
#35268=CARTESIAN_POINT('Ctrl Pts',(221.275,11.20763433117,-3.05018437886434));
#35269=CARTESIAN_POINT('Ctrl Pts',(221.275,11.2677273629663,-2.77820619727043));
#35270=CARTESIAN_POINT('Ctrl Pts',(221.275,11.3180837281662,-2.50421136753778));
#35271=CARTESIAN_POINT('Ctrl Pts',(221.275,11.3669567537033,-2.23828756113564));
#35272=CARTESIAN_POINT('Ctrl Pts',(221.275,11.4066581240996,-1.97046360811415));
#35273=CARTESIAN_POINT('Ctrl Pts',(221.275,11.4370292709931,-1.70123038134001));
#35274=CARTESIAN_POINT('Ctrl Pts',(221.275,11.4484184510781,-1.60026792129971));
#35275=CARTESIAN_POINT('Ctrl Pts',(221.275,11.4584950926119,-1.49910735081375));
#35276=CARTESIAN_POINT('Ctrl Pts',(221.275,11.4672491072449,-1.39777489293779));
#35277=CARTESIAN_POINT('Ctrl Pts',(221.275,11.4701007059261,-1.36476609464781));
#35278=CARTESIAN_POINT('Ctrl Pts',(221.275,11.4728119512237,-1.33173905908973));
#35279=CARTESIAN_POINT('Ctrl Pts',(221.275,11.4753824725815,-1.29869469870299));
#35280=CARTESIAN_POINT('Ctrl Pts',(221.275,11.4775999226471,-1.27018911212607));
#35281=CARTESIAN_POINT('Ctrl Pts',(221.275,11.4797125453341,-1.24167159445729));
#35282=CARTESIAN_POINT('Ctrl Pts',(221.275,11.4817193140495,-1.21315549880311));
#35283=CARTESIAN_POINT('Ctrl Pts',(221.275,11.5011350170463,-0.937259208618942));
#35284=CARTESIAN_POINT('Ctrl Pts',(221.275,11.5106714848227,-0.661179693776942));
#35285=CARTESIAN_POINT('Ctrl Pts',(221.275,11.5102874958201,-0.385443059455608));
#35286=CARTESIAN_POINT('Ctrl Pts',(221.275,11.5099042811777,-0.110262481327592));
#35287=CARTESIAN_POINT('Ctrl Pts',(221.275,11.4996406157499,0.164577224029352));
#35288=CARTESIAN_POINT('Ctrl Pts',(221.275,11.4794039795718,0.438556636957472));
#35289=CARTESIAN_POINT('Ctrl Pts',(221.275,11.4722347702517,0.535619001641185));
#35290=CARTESIAN_POINT('Ctrl Pts',(221.275,11.4638134144713,0.63257338158797));
#35291=CARTESIAN_POINT('Ctrl Pts',(221.275,11.4541342279419,0.729396561550147));
#35292=CARTESIAN_POINT('Ctrl Pts',(221.275,11.4267205290986,1.00362224037745));
#35293=CARTESIAN_POINT('Ctrl Pts',(221.275,11.3892207871223,1.27679647484803));
#35294=CARTESIAN_POINT('Ctrl Pts',(221.275,11.3418252254633,1.54840422003022));
#35295=CARTESIAN_POINT('Ctrl Pts',(221.275,11.2945164335928,1.81951471724761));
#35296=CARTESIAN_POINT('Ctrl Pts',(221.275,11.2373477738928,2.08906505227169));
#35297=CARTESIAN_POINT('Ctrl Pts',(221.275,11.1704599346459,2.35652492196683));
#35298=CARTESIAN_POINT('Ctrl Pts',(221.275,11.1300498473678,2.51810999930639));
#35299=CARTESIAN_POINT('Ctrl Pts',(221.275,11.0860914022179,2.67893168126456));
#35300=CARTESIAN_POINT('Ctrl Pts',(221.275,11.0386075900197,2.83886842734617));
#35301=CARTESIAN_POINT('Ctrl Pts',(221.275,11.0163604629247,2.91380203003167));
#35302=CARTESIAN_POINT('Ctrl Pts',(221.275,10.9933393942903,2.98854132328388));
#35303=CARTESIAN_POINT('Ctrl Pts',(221.275,10.969546312832,3.06307348804126));
#35304=CARTESIAN_POINT('Ctrl Pts',(221.275,10.9562808923639,3.1046276055958));
#35305=CARTESIAN_POINT('Ctrl Pts',(221.275,10.9427733197184,3.14612368453342));
#35306=CARTESIAN_POINT('Ctrl Pts',(221.275,10.9290355953377,3.18752479983685));
#35307=CARTESIAN_POINT('Ctrl Pts',(221.275,10.8428356196636,3.44730400585014));
#35308=CARTESIAN_POINT('Ctrl Pts',(221.275,10.747516265156,3.70354978717551));
#35309=CARTESIAN_POINT('Ctrl Pts',(221.275,10.6433125138665,3.95577833042948));
#35310=CARTESIAN_POINT('Ctrl Pts',(221.275,10.5390186962296,4.20822488218407));
#35311=CARTESIAN_POINT('Ctrl Pts',(221.275,10.4258248653737,4.45664784193506));
#35312=CARTESIAN_POINT('Ctrl Pts',(221.275,10.3039170603746,4.70054559637153));
#35313=CARTESIAN_POINT('Ctrl Pts',(221.275,10.1831215214782,4.94221806913078));
#35314=CARTESIAN_POINT('Ctrl Pts',(221.275,10.0537699862449,5.17944806618623));
#35315=CARTESIAN_POINT('Ctrl Pts',(221.275,9.91599909542756,5.41172300983443));
#35316=CARTESIAN_POINT('Ctrl Pts',(221.275,9.80028461062045,5.60681193811528));
#35317=CARTESIAN_POINT('Ctrl Pts',(221.275,9.67862993840671,5.79840511634343));
#35318=CARTESIAN_POINT('Ctrl Pts',(221.275,9.55109377146823,5.98618112170417));
#35319=CARTESIAN_POINT('Ctrl Pts',(221.275,9.42138382955108,6.17715765278124));
#35320=CARTESIAN_POINT('Ctrl Pts',(221.275,9.28558990525997,6.36418593019245));
#35321=CARTESIAN_POINT('Ctrl Pts',(221.275,9.14393690820591,6.54702634593604));
#35322=CARTESIAN_POINT('Ctrl Pts',(221.275,9.08196372199475,6.62701902782386));
#35323=CARTESIAN_POINT('Ctrl Pts',(221.275,9.01886886064511,6.70620985440605));
#35324=CARTESIAN_POINT('Ctrl Pts',(221.275,8.95467023937287,6.7845774279421));
#35325=CARTESIAN_POINT('Ctrl Pts',(221.275,8.91563048444777,6.83223344927547));
#35326=CARTESIAN_POINT('Ctrl Pts',(221.275,8.87618255274118,6.87958501825374));
#35327=CARTESIAN_POINT('Ctrl Pts',(221.275,8.836330383554,6.92662716602368));
#35328=CARTESIAN_POINT('Ctrl Pts',(221.275,8.81794772954525,6.94832634937858));
#35329=CARTESIAN_POINT('Ctrl Pts',(221.275,8.79947934272416,6.96995931363031));
#35330=CARTESIAN_POINT('Ctrl Pts',(221.275,8.78093454974258,6.99151534017595));
#35331=CARTESIAN_POINT('Ctrl Pts',(221.275,8.60557477544427,7.1953493734579));
#35332=CARTESIAN_POINT('Ctrl Pts',(221.275,8.4231845219114,7.39254607125566));
#35333=CARTESIAN_POINT('Ctrl Pts',(221.275,8.2342075818506,7.5828128355903));
#35334=CARTESIAN_POINT('Ctrl Pts',(221.275,8.04385731241664,7.77446230268281));
#35335=CARTESIAN_POINT('Ctrl Pts',(221.275,7.84682381483834,7.9590811824017));
#35336=CARTESIAN_POINT('Ctrl Pts',(221.275,7.64352068799585,8.13633604943754));
#35337=CARTESIAN_POINT('Ctrl Pts',(221.275,7.44061961337772,8.31324037728258));
#35338=CARTESIAN_POINT('Ctrl Pts',(221.275,7.23147317562663,8.48281017305945));
#35339=CARTESIAN_POINT('Ctrl Pts',(221.275,7.01646024296744,8.64467378549681));
#35340=CARTESIAN_POINT('Ctrl Pts',(221.275,6.80309809964125,8.80529466931544));
#35341=CARTESIAN_POINT('Ctrl Pts',(221.275,6.58395869341164,8.95832757843745));
#35342=CARTESIAN_POINT('Ctrl Pts',(221.275,6.35938798073357,9.10336446350721));
#35343=CARTESIAN_POINT('Ctrl Pts',(221.275,6.13874862336006,9.24586231968636));
#35344=CARTESIAN_POINT('Ctrl Pts',(221.275,5.91286597430829,9.38064188928147));
#35345=CARTESIAN_POINT('Ctrl Pts',(221.275,5.68205195455429,9.50726865664796));
#35346=CARTESIAN_POINT('Ctrl Pts',(221.275,5.60434579241614,9.54989899654888));
#35347=CARTESIAN_POINT('Ctrl Pts',(221.275,5.52608059861463,9.59160487181287));
#35348=CARTESIAN_POINT('Ctrl Pts',(221.275,5.44726799658347,9.63236838871404));
#35349=CARTESIAN_POINT('Ctrl Pts',(203.504027251253,-4.76011662834041,9.98982177454118));
#35350=CARTESIAN_POINT('Ctrl Pts',(203.543518301805,-6.41263020639832,9.20240458742794));
#35351=CARTESIAN_POINT('Ctrl Pts',(203.622500402911,-9.31767905895346,6.7923303895484));
#35352=CARTESIAN_POINT('Ctrl Pts',(203.740973554569,-11.4278517756257,1.53578666224697));
#35353=CARTESIAN_POINT('Ctrl Pts',(203.859446706228,-10.780545153515,-4.09039060373519));
#35354=CARTESIAN_POINT('Ctrl Pts',(203.977919857886,-7.53249900452806,-8.73016539923752));
#35355=CARTESIAN_POINT('Ctrl Pts',(204.096393009544,-2.46707396923755,-11.263487531142));
#35356=CARTESIAN_POINT('Ctrl Pts',(204.214866161202,3.19351689060185,-11.0794786062488));
#35357=CARTESIAN_POINT('Ctrl Pts',(204.333339312861,8.08365868074054,-8.22238332192522));
#35358=CARTESIAN_POINT('Ctrl Pts',(204.451812464519,11.0235253467705,-3.38157672049597));
#35359=CARTESIAN_POINT('Ctrl Pts',(204.570285616177,11.303857784602,2.27508107448027));
#35360=CARTESIAN_POINT('Ctrl Pts',(204.688758767836,8.85701624610765,7.38284688961676));
#35361=CARTESIAN_POINT('Ctrl Pts',(204.807231919494,4.27332958062524,10.7094275823243));
#35362=CARTESIAN_POINT('Ctrl Pts',(204.925705071152,-1.34134224161475,11.4522476363554));
#35363=CARTESIAN_POINT('Ctrl Pts',(205.044178222811,-6.63240123149158,9.43209587689214));
#35364=CARTESIAN_POINT('Ctrl Pts',(205.162651374469,-10.3233254010507,5.13635381066313));
#35365=CARTESIAN_POINT('Ctrl Pts',(205.281124526127,-11.5236412090866,-0.398586246501114));
#35366=CARTESIAN_POINT('Ctrl Pts',(205.399597677786,-9.94376021587458,-5.83736334058754));
#35367=CARTESIAN_POINT('Ctrl Pts',(205.518070829444,-5.96484490322095,-9.86781652946403));
#35368=CARTESIAN_POINT('Ctrl Pts',(205.636543981102,-0.546849485135998,
-11.5175576204352));
#35369=CARTESIAN_POINT('Ctrl Pts',(205.755017132761,5.00307899201479,-10.3885696055));
#35370=CARTESIAN_POINT('Ctrl Pts',(205.873490284419,9.3459632629926,-6.75323245198365));
#35371=CARTESIAN_POINT('Ctrl Pts',(205.991963436077,11.4340378838074,-1.4886085900372));
#35372=CARTESIAN_POINT('Ctrl Pts',(206.110436587736,10.7635333998672,4.13515738637055));
#35373=CARTESIAN_POINT('Ctrl Pts',(206.228909739394,7.49621590665812,8.76127416208841));
#35374=CARTESIAN_POINT('Ctrl Pts',(206.347382891052,2.42035931523562,11.2736435390796));
#35375=CARTESIAN_POINT('Ctrl Pts',(206.46585604271,-3.23943382596151,11.0661305951517));
#35376=CARTESIAN_POINT('Ctrl Pts',(206.584329194369,-8.1176802770788,8.18879995973997));
#35377=CARTESIAN_POINT('Ctrl Pts',(206.702802346027,-11.0374529662102,3.33583720829552));
#35378=CARTESIAN_POINT('Ctrl Pts',(206.821275497686,-11.2943267364968,-2.32193053962052));
#35379=CARTESIAN_POINT('Ctrl Pts',(206.939748649344,-8.82632815191763,-7.41950869102601));
#35380=CARTESIAN_POINT('Ctrl Pts',(207.058221801002,-4.22888722542433,-10.7270541480969));
#35381=CARTESIAN_POINT('Ctrl Pts',(207.17669495266,1.3888161887093,-11.4465875899995));
#35382=CARTESIAN_POINT('Ctrl Pts',(207.295168104319,6.67145342963094,-9.40451418191398));
#35383=CARTESIAN_POINT('Ctrl Pts',(207.413641255977,10.3445339930023,-5.09350511231458));
#35384=CARTESIAN_POINT('Ctrl Pts',(207.532114407635,11.5218894583563,0.446364392591136));
#35385=CARTESIAN_POINT('Ctrl Pts',(207.650587559294,9.91947072438404,5.87854390216176));
#35386=CARTESIAN_POINT('Ctrl Pts',(207.769060710952,5.92387777273893,9.89246430345869));
#35387=CARTESIAN_POINT('Ctrl Pts',(207.88753386261,0.499088450816281,11.5197260635753));
#35388=CARTESIAN_POINT('Ctrl Pts',(208.006007014269,-5.04611108713692,10.3677355655817));
#35389=CARTESIAN_POINT('Ctrl Pts',(208.124480165927,-9.37388448524946,6.71442235183001));
#35390=CARTESIAN_POINT('Ctrl Pts',(208.242953317585,-11.4401119508359,1.44118576661595));
#35391=CARTESIAN_POINT('Ctrl Pts',(208.361426469244,-10.7462948809079,-4.17975169048676));
#35392=CARTESIAN_POINT('Ctrl Pts',(208.479899620902,-7.45982377135673,-8.79228111253593));
#35393=CARTESIAN_POINT('Ctrl Pts',(208.59837277256,-2.37359354017129,-11.2835823906954));
#35394=CARTESIAN_POINT('Ctrl Pts',(208.716845924218,3.28529051715118,-11.0526034977951));
#35395=CARTESIAN_POINT('Ctrl Pts',(208.835319075877,8.15156448652971,-8.15507046465587));
#35396=CARTESIAN_POINT('Ctrl Pts',(208.953792227535,11.0511897802984,-3.29004290266605));
#35397=CARTESIAN_POINT('Ctrl Pts',(209.072265379193,11.2846020076979,2.3687413090957));
#35398=CARTESIAN_POINT('Ctrl Pts',(209.190738530852,8.79548807096082,7.4560423453157));
#35399=CARTESIAN_POINT('Ctrl Pts',(209.30921168251,4.18437227866815,10.7444965677815));
#35400=CARTESIAN_POINT('Ctrl Pts',(209.427684834168,-1.43626631304541,11.4407306121404));
#35401=CARTESIAN_POINT('Ctrl Pts',(209.546157985827,-6.71039090158305,9.37677086258944));
#35402=CARTESIAN_POINT('Ctrl Pts',(209.664631137485,-10.3655647474466,5.05056881232662));
#35403=CARTESIAN_POINT('Ctrl Pts',(209.783104289143,-11.5199396097286,-0.494134849774289));
#35404=CARTESIAN_POINT('Ctrl Pts',(209.901577440802,-9.89501069369702,-5.91962340298576));
#35405=CARTESIAN_POINT('Ctrl Pts',(210.02005059246,-5.88280879368037,-9.9169419963289));
#35406=CARTESIAN_POINT('Ctrl Pts',(210.138523744118,-0.451318836496845,
-11.5216964536208));
#35407=CARTESIAN_POINT('Ctrl Pts',(210.256996895777,5.08905642651245,-10.3467232759617));
#35408=CARTESIAN_POINT('Ctrl Pts',(210.375470047435,9.40164454536766,-6.67549681328017));
#35409=CARTESIAN_POINT('Ctrl Pts',(210.493943199093,11.4459893320066,-1.39373816520411));
#35410=CARTESIAN_POINT('Ctrl Pts',(210.612416350752,10.7288716045437,4.2242741334779));
#35411=CARTESIAN_POINT('Ctrl Pts',(210.73088950241,7.42330338187457,8.82313690034356));
#35412=CARTESIAN_POINT('Ctrl Pts',(210.849362654068,2.32678695671764,11.2933272475212));
#35413=CARTESIAN_POINT('Ctrl Pts',(210.967835805727,-3.33109072546143,11.0388863768181));
#35414=CARTESIAN_POINT('Ctrl Pts',(211.086308957385,-8.18530854892373,8.1212007622316));
#35415=CARTESIAN_POINT('Ctrl Pts',(211.204782109043,-11.0647365950617,3.24419203245698));
#35416=CARTESIAN_POINT('Ctrl Pts',(211.323255260701,-11.2746832665987,-2.41551135361317));
#35417=CARTESIAN_POINT('Ctrl Pts',(211.44172841236,-8.7644967721873,-7.4924478104204));
#35418=CARTESIAN_POINT('Ctrl Pts',(211.560201564018,-4.13978539143139,-10.7617542610137));
#35419=CARTESIAN_POINT('Ctrl Pts',(211.678674715676,1.48369174414633,-11.4346769377148));
#35420=CARTESIAN_POINT('Ctrl Pts',(211.797147867335,6.74921300408072,-9.34886633165234));
#35421=CARTESIAN_POINT('Ctrl Pts',(211.915621018993,10.3864172902835,-5.00754567963735));
#35422=CARTESIAN_POINT('Ctrl Pts',(212.034094170651,11.5177917027214,0.541896811466134));
#35423=CARTESIAN_POINT('Ctrl Pts',(212.15256732231,9.87038054147729,5.96060112975038));
#35424=CARTESIAN_POINT('Ctrl Pts',(212.271040473968,5.84163867350336,9.94124919060903));
#35425=CARTESIAN_POINT('Ctrl Pts',(212.389513625626,0.403541462807075,11.523468755082));
#35426=CARTESIAN_POINT('Ctrl Pts',(212.507986777285,-5.13191427148244,10.325533098669));
#35427=CARTESIAN_POINT('Ctrl Pts',(212.626459928943,-9.42924296622852,6.636456505198));
#35428=CARTESIAN_POINT('Ctrl Pts',(212.744933080601,-11.4516699261996,1.34626660172895));
#35429=CARTESIAN_POINT('Ctrl Pts',(212.863406232259,-10.7112638703615,-4.26872394996941));
#35430=CARTESIAN_POINT('Ctrl Pts',(212.981879383918,-7.3866553660777,-8.85384099497784));
#35431=CARTESIAN_POINT('Ctrl Pts',(213.100352535576,-2.27994036961207,-11.3028779420362));
#35432=CARTESIAN_POINT('Ctrl Pts',(213.218825687235,3.37683366346876,-11.0249794680452));
#35433=CARTESIAN_POINT('Ctrl Pts',(213.337298838893,8.21891188410895,-8.08719143478177));
#35434=CARTESIAN_POINT('Ctrl Pts',(213.455771990551,11.0780931775952,-3.1982853859645));
#35435=CARTESIAN_POINT('Ctrl Pts',(213.574245142209,11.2645706837284,2.46223986907059));
#35436=CARTESIAN_POINT('Ctrl Pts',(213.692718293868,8.73335478842003,7.52872446043392));
#35437=CARTESIAN_POINT('Ctrl Pts',(213.811191445526,4.09512733028103,10.7788269310876));
#35438=CARTESIAN_POINT('Ctrl Pts',(213.929664597184,-1.53109166664286,11.4284266708017));
#35439=CARTESIAN_POINT('Ctrl Pts',(214.048137748843,-6.78791906966887,9.32080106885565));
#35440=CARTESIAN_POINT('Ctrl Pts',(214.166610900501,-10.4070912630023,4.96443645392882));
#35441=CARTESIAN_POINT('Ctrl Pts',(214.285084052159,-11.515445774263,-0.589649456511533));
#35442=CARTESIAN_POINT('Ctrl Pts',(214.403557203818,-9.84558069118264,-6.00147637793954));
#35443=CARTESIAN_POINT('Ctrl Pts',(214.522030355476,-5.80036812003173,-9.96538546839381));
#35444=CARTESIAN_POINT('Ctrl Pts',(214.640503507134,-0.355757151167077,
-11.5250429374883));
#35445=CARTESIAN_POINT('Ctrl Pts',(214.758976658793,5.17468388520643,-10.3041653980194));
#35446=CARTESIAN_POINT('Ctrl Pts',(214.877449810451,9.4566792733418,-6.59730209879029));
#35447=CARTESIAN_POINT('Ctrl Pts',(214.995922962109,11.4571536357504,-1.29877189235286));
#35448=CARTESIAN_POINT('Ctrl Pts',(215.114396113768,10.6934719810851,4.31310037575084));
#35449=CARTESIAN_POINT('Ctrl Pts',(215.232869265426,7.34988035404288,8.88439286855379));
#35450=CARTESIAN_POINT('Ctrl Pts',(215.351342417084,2.23305458427189,11.3122343100387));
#35451=CARTESIAN_POINT('Ctrl Pts',(215.469815568742,-3.42251854473055,11.0108830105732));
#35452=CARTESIAN_POINT('Ctrl Pts',(215.588288720401,-8.25237391435474,8.05304306701711));
#35453=CARTESIAN_POINT('Ctrl Pts',(215.706761872059,-11.0912592982637,3.15232375244584));
#35454=CARTESIAN_POINT('Ctrl Pts',(215.825235023717,-11.2542644329493,-2.50892605208056));
#35455=CARTESIAN_POINT('Ctrl Pts',(215.943708175376,-8.70206265507251,-7.56487167166418));
#35456=CARTESIAN_POINT('Ctrl Pts',(216.062181327034,-4.05039886300789,-10.7957142844788));
#35457=CARTESIAN_POINT('Ctrl Pts',(216.180654478693,1.57846526560428,-11.4219799188598));
#35458=CARTESIAN_POINT('Ctrl Pts',(216.299127630351,6.8265084328873,-9.29257555671587));
#35459=CARTESIAN_POINT('Ctrl Pts',(216.417600782009,10.4275863101622,-4.92124187636331));
#35460=CARTESIAN_POINT('Ctrl Pts',(216.536073933668,11.512901864686,0.637391963915507));
#35461=CARTESIAN_POINT('Ctrl Pts',(216.654547085325,9.82061156918846,6.04224844479904));
#35462=CARTESIAN_POINT('Ctrl Pts',(216.773020236984,5.75899784281591,9.98935041471651));
#35463=CARTESIAN_POINT('Ctrl Pts',(216.891493388642,0.307966723115988,11.5264189737753));
#35464=CARTESIAN_POINT('Ctrl Pts',(217.009966540301,-5.21736453236138,10.2826205413801));
#35465=CARTESIAN_POINT('Ctrl Pts',(217.128439691959,-9.48395299500455,6.55803426722514));
#35466=CARTESIAN_POINT('Ctrl Pts',(217.246912843617,-11.4624403663795,1.25125485363602));
#35467=CARTESIAN_POINT('Ctrl Pts',(217.365385995275,-10.6754962426044,-4.35740264787347));
#35468=CARTESIAN_POINT('Ctrl Pts',(217.483859146934,-7.31297897803034,-8.91479199580349));
#35469=CARTESIAN_POINT('Ctrl Pts',(217.602332298592,-2.18613040678854,-11.3213961906678));
#35470=CARTESIAN_POINT('Ctrl Pts',(217.720805450251,3.46814458380223,-10.9965972467579));
#35471=CARTESIAN_POINT('Ctrl Pts',(217.839278601909,8.28569406435969,-8.01875624603833));
#35472=CARTESIAN_POINT('Ctrl Pts',(217.957751753567,11.104234730707,-3.1063079221047));
#35473=CARTESIAN_POINT('Ctrl Pts',(218.076224905225,11.2437646914523,2.55556909998565));
#35474=CARTESIAN_POINT('Ctrl Pts',(218.194698056884,8.6706209101412,7.60088882263999));
#35475=CARTESIAN_POINT('Ctrl Pts',(218.313171208542,4.00560075861009,10.8124160308581));
#35476=CARTESIAN_POINT('Ctrl Pts',(218.4316443602,-1.62581172654604,11.4153367927059));
#35477=CARTESIAN_POINT('Ctrl Pts',(218.550117511859,-6.86498043029599,9.26419028054612));
#35478=CARTESIAN_POINT('Ctrl Pts',(218.668590663517,-10.4479020793708,4.87796268948343));
#35479=CARTESIAN_POINT('Ctrl Pts',(218.787063815175,-11.5101600177867,-0.685123512676105));
#35480=CARTESIAN_POINT('Ctrl Pts',(218.905536966834,-9.79547360465598,-6.08291662972795));
#35481=CARTESIAN_POINT('Ctrl Pts',(219.024010118492,-5.71752855338079,-10.0131436167636));
#35482=CARTESIAN_POINT('Ctrl Pts',(219.14248327015,-0.260170999755849,-11.5275968419408));
#35483=CARTESIAN_POINT('Ctrl Pts',(219.260956421809,5.25995547801919,-10.260898895706));
#35484=CARTESIAN_POINT('Ctrl Pts',(219.379429573467,9.51106366467834,-6.51865369284798));
#35485=CARTESIAN_POINT('Ctrl Pts',(219.497902725125,11.4675300222433,-1.2037162874228));
#35486=CARTESIAN_POINT('Ctrl Pts',(219.616375876784,10.657336974314,4.40162997311355));
#35487=CARTESIAN_POINT('Ctrl Pts',(219.734849028442,7.27595185085969,8.94503792000617));
#35488=CARTESIAN_POINT('Ctrl Pts',(219.8533221801,2.13916868907181,11.3303632886701));
#35489=CARTESIAN_POINT('Ctrl Pts',(219.971795331758,-3.51371109060621,10.9821227099977));
#35490=CARTESIAN_POINT('Ctrl Pts',(220.090268483417,-8.31887156411482,7.98433096001791));
#35491=CARTESIAN_POINT('Ctrl Pts',(220.208741635075,-11.1170196637652,3.06023994245929));
#35492=CARTESIAN_POINT('Ctrl Pts',(220.327214786733,-11.2330707790818,-2.60217083598129));
#35493=CARTESIAN_POINT('Ctrl Pts',(220.445687938392,-8.639031892527,-7.6367698092379));
#35494=CARTESIAN_POINT('Ctrl Pts',(220.56416109005,-3.96073003010559,-10.828943343905));
#35495=CARTESIAN_POINT('Ctrl Pts',(220.682634241709,1.67312238226268,-11.4084734661502));
#35496=CARTESIAN_POINT('Ctrl Pts',(220.801107393367,6.9033507794017,-9.23569581394894));
#35497=CARTESIAN_POINT('Ctrl Pts',(220.919580545025,10.4680037040556,-4.83449558382035));
#35498=CARTESIAN_POINT('Ctrl Pts',(221.038053696683,11.5072892832615,0.732618747333446));
#35499=CARTESIAN_POINT('Ctrl Pts',(221.156526848342,9.7699936824466,6.12389733841086));
#35500=CARTESIAN_POINT('Ctrl Pts',(221.235508949447,7.04065173359568,8.73128281072966));
#35501=CARTESIAN_POINT('Ctrl Pts',(221.275,5.44726799658334,9.63236838871412));
#35502=CARTESIAN_POINT('Ctrl Pts',(203.669351500835,-4.88329262285739,10.2483251533871));
#35503=CARTESIAN_POINT('Ctrl Pts',(203.708842551388,-6.57856775894483,9.44053222704407));
#35504=CARTESIAN_POINT('Ctrl Pts',(203.787824652493,-9.55878961869132,6.96809332061598));
#35505=CARTESIAN_POINT('Ctrl Pts',(203.906297804152,-11.7235665905264,1.57552771572495));
#35506=CARTESIAN_POINT('Ctrl Pts',(204.02477095581,-11.0595098248454,-4.19623631507308));
#35507=CARTESIAN_POINT('Ctrl Pts',(204.143244107468,-7.72741503884474,-8.95607305850505));
#35508=CARTESIAN_POINT('Ctrl Pts',(204.261717259127,-2.53091364238729,-11.5549491457836));
#35509=CARTESIAN_POINT('Ctrl Pts',(204.380190410785,3.27615449167754,-11.3661786816061));
#35510=CARTESIAN_POINT('Ctrl Pts',(204.498663562443,8.29283689528426,-8.43515126902723));
#35511=CARTESIAN_POINT('Ctrl Pts',(204.617136714102,11.3087775377752,-3.4690806848112));
#35512=CARTESIAN_POINT('Ctrl Pts',(204.73560986576,11.5963640472022,2.33395260974631));
#35513=CARTESIAN_POINT('Ctrl Pts',(204.854083017418,9.08620638360809,7.57389042468078));
#35514=CARTESIAN_POINT('Ctrl Pts',(204.972556169076,4.38390914454991,10.986551967325));
#35515=CARTESIAN_POINT('Ctrl Pts',(205.091029320735,-1.37605171986887,11.7485937350338));
#35516=CARTESIAN_POINT('Ctrl Pts',(205.209502472393,-6.80402572759336,9.676167163528));
#35517=CARTESIAN_POINT('Ctrl Pts',(205.327975624052,-10.5904587451008,5.26926557275166));
#35518=CARTESIAN_POINT('Ctrl Pts',(205.44644877571,-11.8218347360971,-0.408900333559652));
#35519=CARTESIAN_POINT('Ctrl Pts',(205.564921927368,-10.2010716747024,-5.98841489897856));
#35520=CARTESIAN_POINT('Ctrl Pts',(205.683395079026,-6.11919526067218,-10.1231628181434));
#35521=CARTESIAN_POINT('Ctrl Pts',(205.801868230685,-0.561000131946154,
-11.8155937243948));
#35522=CARTESIAN_POINT('Ctrl Pts',(205.920341382343,5.13254204483568,-10.6573912526731));
#35523=CARTESIAN_POINT('Ctrl Pts',(206.038814534001,9.58780572390719,-6.92798365839843));
#35524=CARTESIAN_POINT('Ctrl Pts',(206.15728768566,11.7299127746237,-1.52712883183816));
#35525=CARTESIAN_POINT('Ctrl Pts',(206.275760837318,11.0420578635646,4.24216151322699));
#35526=CARTESIAN_POINT('Ctrl Pts',(206.394233988976,7.69019305501607,8.98798681272517));
#35527=CARTESIAN_POINT('Ctrl Pts',(206.512707140635,2.48299016843104,11.5653679574455));
#35528=CARTESIAN_POINT('Ctrl Pts',(206.631180292293,-3.32325960468488,11.3524852683539));
#35529=CARTESIAN_POINT('Ctrl Pts',(206.749653443951,-8.32773885743942,8.40069888106815));
#35530=CARTESIAN_POINT('Ctrl Pts',(206.86812659561,-11.323065557707,3.42215758608464));
#35531=CARTESIAN_POINT('Ctrl Pts',(206.986599747268,-11.5865863672557,-2.38201438330499));
#35532=CARTESIAN_POINT('Ctrl Pts',(207.105072898926,-9.05472418355536,-7.61150091163746));
#35533=CARTESIAN_POINT('Ctrl Pts',(207.223546050585,-4.33831676893397,-11.0046346500247));
#35534=CARTESIAN_POINT('Ctrl Pts',(207.342019202243,1.4247541348989,-11.7427872254937));
#35535=CARTESIAN_POINT('Ctrl Pts',(207.460492353901,6.84408846680124,-9.6478717459723));
#35536=CARTESIAN_POINT('Ctrl Pts',(207.578965505559,10.6122161449094,-5.2253080925297));
#35537=CARTESIAN_POINT('Ctrl Pts',(207.697438657218,11.8200376558811,0.457914819243914));
#35538=CARTESIAN_POINT('Ctrl Pts',(207.815911808876,10.1761536519165,6.03066107659177));
#35539=CARTESIAN_POINT('Ctrl Pts',(207.934384960534,6.07716803703832,10.1484483945937));
#35540=CARTESIAN_POINT('Ctrl Pts',(208.052858112193,0.512003200827929,11.8178182796349));
#35541=CARTESIAN_POINT('Ctrl Pts',(208.171331263851,-5.17668766753006,10.6360180970593));
#35542=CARTESIAN_POINT('Ctrl Pts',(208.289804415509,-9.6164494545789,6.88816928186734));
#35543=CARTESIAN_POINT('Ctrl Pts',(208.408277567168,-11.7361440183151,1.47847886339215));
#35544=CARTESIAN_POINT('Ctrl Pts',(208.526750718826,-11.0243732690398,-4.28790976969105));
#35545=CARTESIAN_POINT('Ctrl Pts',(208.645223870484,-7.65285921222969,-9.01979611997538));
#35546=CARTESIAN_POINT('Ctrl Pts',(208.763697022143,-2.43501425056925,-11.5755639935018));
#35547=CARTESIAN_POINT('Ctrl Pts',(208.882170173801,3.37030291460337,-11.3386081346851));
#35548=CARTESIAN_POINT('Ctrl Pts',(209.000643325459,8.36249987759127,-8.3660965787766));
#35549=CARTESIAN_POINT('Ctrl Pts',(209.119116477118,11.3371578348792,-3.37517827605727));
#35550=CARTESIAN_POINT('Ctrl Pts',(209.237589628776,11.5766099948028,2.43003645988342));
#35551=CARTESIAN_POINT('Ctrl Pts',(209.356062780434,9.02308606382359,7.6489799354531));
#35552=CARTESIAN_POINT('Ctrl Pts',(209.474535932093,4.2926499233346,11.0225284215477));
#35553=CARTESIAN_POINT('Ctrl Pts',(209.593009083751,-1.47343211071668,11.7367786885176));
#35554=CARTESIAN_POINT('Ctrl Pts',(209.711482235409,-6.88403351108953,9.6194105217694));
#35555=CARTESIAN_POINT('Ctrl Pts',(209.829955387068,-10.6337911053672,5.1812607438291));
#35556=CARTESIAN_POINT('Ctrl Pts',(209.948428538726,-11.8180373516528,-0.506921417057956));
#35557=CARTESIAN_POINT('Ctrl Pts',(210.066901690384,-10.1510606769466,-6.07280357833852));
#35558=CARTESIAN_POINT('Ctrl Pts',(210.185374842043,-6.03503632932535,-10.1735594887854));
#35559=CARTESIAN_POINT('Ctrl Pts',(210.303847993701,-0.462997467688116,
-11.8198396568247));
#35560=CARTESIAN_POINT('Ctrl Pts',(210.422321145359,5.22074428952753,-10.614462079234));
#35561=CARTESIAN_POINT('Ctrl Pts',(210.540794297017,9.64492785277154,-6.84823647977811));
#35562=CARTESIAN_POINT('Ctrl Pts',(210.659267448676,11.7421734865726,-1.42980347578353));
#35563=CARTESIAN_POINT('Ctrl Pts',(210.777740600334,11.0064991362026,4.33358430550301));
#35564=CARTESIAN_POINT('Ctrl Pts',(210.896213751992,7.61539379647069,9.05145035299908));
#35565=CARTESIAN_POINT('Ctrl Pts',(211.014686903651,2.38699646833266,11.5855610148278));
#35566=CARTESIAN_POINT('Ctrl Pts',(211.133160055309,-3.41728828005328,11.3245360602164));
#35567=CARTESIAN_POINT('Ctrl Pts',(211.251633206967,-8.3971171241463,8.33135044104499));
#35568=CARTESIAN_POINT('Ctrl Pts',(211.370106358626,-11.3510551961755,3.32814093774701));
#35569=CARTESIAN_POINT('Ctrl Pts',(211.488579510284,-11.5664345896564,-2.47801675767762));
#35570=CARTESIAN_POINT('Ctrl Pts',(211.607052661942,-8.99129281326067,-7.68632745297379));
#35571=CARTESIAN_POINT('Ctrl Pts',(211.725525813601,-4.24690927567419,-11.0402326865118));
#35572=CARTESIAN_POINT('Ctrl Pts',(211.843998965259,1.52208475432044,-11.7305683651218));
#35573=CARTESIAN_POINT('Ctrl Pts',(211.962472116917,6.9238602005454,-9.59078391433333));
#35574=CARTESIAN_POINT('Ctrl Pts',(212.080945268576,10.6551832426936,-5.13712431548555));
#35575=CARTESIAN_POINT('Ctrl Pts',(212.199418420234,11.8158338639524,0.555919299545619));
#35576=CARTESIAN_POINT('Ctrl Pts',(212.317891571892,10.1257931782642,6.11484167245154));
#35577=CARTESIAN_POINT('Ctrl Pts',(212.43636472355,5.99280086329799,10.1984956724502));
#35578=CARTESIAN_POINT('Ctrl Pts',(212.554837875209,0.413983774391252,11.8216578195561));
#35579=CARTESIAN_POINT('Ctrl Pts',(212.673311026867,-5.26471115305508,10.5927235705945));
#35580=CARTESIAN_POINT('Ctrl Pts',(212.791784178525,-9.67324042902019,6.80818593830257));
#35581=CARTESIAN_POINT('Ctrl Pts',(212.910257330184,-11.7480010756596,1.38110350605304));
#35582=CARTESIAN_POINT('Ctrl Pts',(213.028730481842,-10.9884357723924,-4.37918433548295));
#35583=CARTESIAN_POINT('Ctrl Pts',(213.1472036335,-7.5777974518522,-9.08294896753436));
#35584=CARTESIAN_POINT('Ctrl Pts',(213.265676785159,-2.33893764728264,-11.595358849568));
#35585=CARTESIAN_POINT('Ctrl Pts',(213.384149936817,3.46421489323522,-11.3102692868746));
#35586=CARTESIAN_POINT('Ctrl Pts',(213.502623088475,8.43159000194017,-8.29646106525633));
#35587=CARTESIAN_POINT('Ctrl Pts',(213.621096240134,11.3647574026644,-3.28104637984854));
#35588=CARTESIAN_POINT('Ctrl Pts',(213.739569391792,11.5560603267582,2.52595445177774));
#35589=CARTESIAN_POINT('Ctrl Pts',(213.85804254345,8.9593449784773,7.72354282209696));
#35590=CARTESIAN_POINT('Ctrl Pts',(213.976515695109,4.20109561235587,11.0577471405335));
#35591=CARTESIAN_POINT('Ctrl Pts',(214.094988846767,-1.57071122924191,11.7241563620785));
#35592=CARTESIAN_POINT('Ctrl Pts',(214.213461998425,-6.96356785044228,9.56199241583145));
#35593=CARTESIAN_POINT('Ctrl Pts',(214.331935150084,-10.6763921891008,5.09289956632158));
#35594=CARTESIAN_POINT('Ctrl Pts',(214.450408301742,-11.8134272306639,-0.604907624302995));
#35595=CARTESIAN_POINT('Ctrl Pts',(214.5688814534,-10.1003515902849,-6.15677463618423));
#35596=CARTESIAN_POINT('Ctrl Pts',(214.687354605058,-5.95046236509621,-10.223256516869));
#35597=CARTESIAN_POINT('Ctrl Pts',(214.805827756717,-0.364962963613078,
-11.8232727365701));
#35598=CARTESIAN_POINT('Ctrl Pts',(214.924300908375,5.3085875022053,-10.5708029448837));
#35599=CARTESIAN_POINT('Ctrl Pts',(215.042774060034,9.70138669655638,-6.76801834601613));
#35600=CARTESIAN_POINT('Ctrl Pts',(215.161247211692,11.7536266853844,-1.33237979148266));
#35601=CARTESIAN_POINT('Ctrl Pts',(215.27972036335,10.9701834881662,4.42470907564521));
#35602=CARTESIAN_POINT('Ctrl Pts',(215.398193515008,7.54007082475531,9.11429142203635));
#35603=CARTESIAN_POINT('Ctrl Pts',(215.516666666667,2.290838613678,11.6049573292716));
#35604=CARTESIAN_POINT('Ctrl Pts',(215.635139818325,-3.51108194735603,11.2958080599434));
#35605=CARTESIAN_POINT('Ctrl Pts',(215.753612969983,-8.46591791829252,8.26142905125167));
#35606=CARTESIAN_POINT('Ctrl Pts',(215.872086121641,-11.3782642187683,3.23389541204245));
#35607=CARTESIAN_POINT('Ctrl Pts',(215.9905592733,-11.5454873844695,-2.5738487180074));
#35608=CARTESIAN_POINT('Ctrl Pts',(216.109032424958,-8.92724310874166,-7.76062540299144));
#35609=CARTESIAN_POINT('Ctrl Pts',(216.227505576617,-4.15520972103837,-11.0750714824926));
#35610=CARTESIAN_POINT('Ctrl Pts',(216.345978728275,1.6193106994627,-11.7175427896269));
#35611=CARTESIAN_POINT('Ctrl Pts',(216.464451879933,7.00315577810006,-9.5330365212662));
#35612=CARTESIAN_POINT('Ctrl Pts',(216.582925031591,10.6974175799506,-5.04858725667831));
#35613=CARTESIAN_POINT('Ctrl Pts',(216.70139818325,11.8108174931637,0.653885549090481));
#35614=CARTESIAN_POINT('Ctrl Pts',(216.819871334908,10.0747363504171,6.19860174859746));
#35615=CARTESIAN_POINT('Ctrl Pts',(216.938344486567,5.90802156263124,10.2478415963371));
#35616=CARTESIAN_POINT('Ctrl Pts',(217.056817638225,0.315935878151426,11.824684380102));
#35617=CARTESIAN_POINT('Ctrl Pts',(217.175290789883,-5.35237258262742,10.5487005789751));
#35618=CARTESIAN_POINT('Ctrl Pts',(217.293763941541,-9.72936617147105,6.72773439350622));
#35619=CARTESIAN_POINT('Ctrl Pts',(217.4122370932,-11.7590502190278,1.28363316976241));
#35620=CARTESIAN_POINT('Ctrl Pts',(217.530710244858,-10.9517425973294,-4.47015774329848));
#35621=CARTESIAN_POINT('Ctrl Pts',(217.649183396516,-7.50221456380103,-9.14547717764492));
#35622=CARTESIAN_POINT('Ctrl Pts',(217.767656548175,-2.24270019446914,-11.6143562889149));
#35623=CARTESIAN_POINT('Ctrl Pts',(217.886129699833,3.55788863664646,-11.28115262805));
#35624=CARTESIAN_POINT('Ctrl Pts',(218.004602851491,8.50010028301504,-8.22625500132398));
#35625=CARTESIAN_POINT('Ctrl Pts',(218.12307600315,11.3915754122696,-3.18668884498026));
#35626=CARTESIAN_POINT('Ctrl Pts',(218.241549154808,11.5347159445663,2.62169873293905));
#35627=CARTESIAN_POINT('Ctrl Pts',(218.360022306466,8.8949877559718,7.79757455810444));
#35628=CARTESIAN_POINT('Ctrl Pts',(218.478495458124,4.10925239061891,11.0922054145474));
#35629=CARTESIAN_POINT('Ctrl Pts',(218.596968609783,-1.66788232942209,11.7107277614516));
#35630=CARTESIAN_POINT('Ctrl Pts',(218.715441761441,-7.0426233029111,9.50391672850897));
#35631=CARTESIAN_POINT('Ctrl Pts',(218.8339149131,-10.7182590537316,5.00418814831287));
#35632=CARTESIAN_POINT('Ctrl Pts',(218.952388064758,-11.8080046963812,-0.702852231661334));
#35633=CARTESIAN_POINT('Ctrl Pts',(219.070861216416,-10.0489478989274,-6.24032229096106));
#35634=CARTESIAN_POINT('Ctrl Pts',(219.189334368075,-5.86547918583989,-10.2722504873586));
#35635=CARTESIAN_POINT('Ctrl Pts',(219.307807519733,-0.266903360355729,
-11.8258927275801));
#35636=CARTESIAN_POINT('Ctrl Pts',(219.426280671391,5.39606564037585,-10.5264168493191));
#35637=CARTESIAN_POINT('Ctrl Pts',(219.544753823049,9.75717837515331,-6.68733478077511));
#35638=CARTESIAN_POINT('Ctrl Pts',(219.663226974708,11.764271578266,-1.23486446348573));
#35639=CARTESIAN_POINT('Ctrl Pts',(219.781700126366,10.9331134275417,4.51552952469302));
#35640=CARTESIAN_POINT('Ctrl Pts',(219.900173278024,7.46422929766668,9.17650576582092));
#35641=CARTESIAN_POINT('Ctrl Pts',(220.018646429683,2.19452326361045,11.6235554256046));
#35642=CARTESIAN_POINT('Ctrl Pts',(220.137119581341,-3.604634253172,11.2663035383954));
#35643=CARTESIAN_POINT('Ctrl Pts',(220.255592732999,-8.5341363061735,8.19093890333965));
#35644=CARTESIAN_POINT('Ctrl Pts',(220.374065884658,-11.404691176895,3.13942877916317));
#35645=CARTESIAN_POINT('Ctrl Pts',(220.492539036316,-11.5237453092929,-2.66950636694637));
#35646=CARTESIAN_POINT('Ctrl Pts',(220.611012187974,-8.86258131959157,-7.83438402535808));
#35647=CARTESIAN_POINT('Ctrl Pts',(220.729485339632,-4.06322055682231,-11.109160399515));
#35648=CARTESIAN_POINT('Ctrl Pts',(220.847958491291,1.71641722763616,-11.7036868348201));
#35649=CARTESIAN_POINT('Ctrl Pts',(220.966431642949,7.08198654909897,-9.47468491983902));
#35650=CARTESIAN_POINT('Ctrl Pts',(221.084904794608,10.7388808416404,-4.95959625845083));
#35651=CARTESIAN_POINT('Ctrl Pts',(221.203377946266,11.8050596767895,0.751576485105512));
#35652=CARTESIAN_POINT('Ctrl Pts',(221.321851097924,10.022808641033,6.2823634441545));
#35653=CARTESIAN_POINT('Ctrl Pts',(221.40083319903,7.22284039556463,8.95721938489205));
#35654=CARTESIAN_POINT('Ctrl Pts',(221.440324249582,5.58822518424655,9.88162206219974));
#35655=CARTESIAN_POINT('Ctrl Pts',(203.834675750418,-5.00646861737437,10.506828532233));
#35656=CARTESIAN_POINT('Ctrl Pts',(203.87416680097,-6.74450531149134,9.6786598666602));
#35657=CARTESIAN_POINT('Ctrl Pts',(203.953148902076,-9.79990017842918,7.14385625168357));
#35658=CARTESIAN_POINT('Ctrl Pts',(204.071622053734,-12.0192814054271,1.61526876920292));
#35659=CARTESIAN_POINT('Ctrl Pts',(204.190095205392,-11.3384744961758,-4.30208202641095));
#35660=CARTESIAN_POINT('Ctrl Pts',(204.308568357051,-7.92233107316142,-9.18198071777258));
#35661=CARTESIAN_POINT('Ctrl Pts',(204.427041508709,-2.59475331553703,-11.8464107604251));
#35662=CARTESIAN_POINT('Ctrl Pts',(204.545514660367,3.35879209275325,-11.6528787569633));
#35663=CARTESIAN_POINT('Ctrl Pts',(204.663987812026,8.50201510982795,-8.64791921612924));
#35664=CARTESIAN_POINT('Ctrl Pts',(204.782460963684,11.5940297287798,-3.55658464912643));
#35665=CARTESIAN_POINT('Ctrl Pts',(204.900934115342,11.8888703098024,2.39282414501235));
#35666=CARTESIAN_POINT('Ctrl Pts',(205.019407267001,9.31539652110854,7.76493395974479));
#35667=CARTESIAN_POINT('Ctrl Pts',(205.137880418659,4.49448870847458,11.2636763523257));
#35668=CARTESIAN_POINT('Ctrl Pts',(205.256353570317,-1.41076119812299,12.0449398337123));
#35669=CARTESIAN_POINT('Ctrl Pts',(205.374826721975,-6.97565022369513,9.92023845016386));
#35670=CARTESIAN_POINT('Ctrl Pts',(205.493299873634,-10.8575920891509,5.40217733484019));
#35671=CARTESIAN_POINT('Ctrl Pts',(205.611773025292,-12.1200282631076,-0.419214420618188));
#35672=CARTESIAN_POINT('Ctrl Pts',(205.730246176951,-10.4583831335302,-6.13946645736958));
#35673=CARTESIAN_POINT('Ctrl Pts',(205.848719328609,-6.27354561812342,-10.3785091068229));
#35674=CARTESIAN_POINT('Ctrl Pts',(205.967192480267,-0.575150778756315,
-12.1136298283544));
#35675=CARTESIAN_POINT('Ctrl Pts',(206.085665631925,5.26200509765657,-10.9262128998462));
#35676=CARTESIAN_POINT('Ctrl Pts',(206.204138783584,9.82964818482179,-7.10273486481322));
#35677=CARTESIAN_POINT('Ctrl Pts',(206.322611935242,12.02578766544,-1.56564907363911));
#35678=CARTESIAN_POINT('Ctrl Pts',(206.441085086901,11.320582327262,4.34916564008343));
#35679=CARTESIAN_POINT('Ctrl Pts',(206.559558238559,7.88417020337402,9.21469946336195));
#35680=CARTESIAN_POINT('Ctrl Pts',(206.678031390217,2.54562102162646,11.8570923758113));
#35681=CARTESIAN_POINT('Ctrl Pts',(206.796504541875,-3.40708538340826,11.6388399415561));
#35682=CARTESIAN_POINT('Ctrl Pts',(206.914977693534,-8.53779743780001,8.61259780239634));
#35683=CARTESIAN_POINT('Ctrl Pts',(207.033450845192,-11.6086781492038,3.50847796387377));
#35684=CARTESIAN_POINT('Ctrl Pts',(207.15192399685,-11.8788459980145,-2.44209822698946));
#35685=CARTESIAN_POINT('Ctrl Pts',(207.270397148509,-9.28312021519312,-7.8034931322489));
#35686=CARTESIAN_POINT('Ctrl Pts',(207.388870300167,-4.4477463124436,-11.2822151519525));
#35687=CARTESIAN_POINT('Ctrl Pts',(207.507343451825,1.46069208108849,-12.0389868609878));
#35688=CARTESIAN_POINT('Ctrl Pts',(207.625816603484,7.01672350397154,-9.89122931003062));
#35689=CARTESIAN_POINT('Ctrl Pts',(207.744289755142,10.8798982968165,-5.35711107274481));
#35690=CARTESIAN_POINT('Ctrl Pts',(207.8627629068,12.118185853406,0.469465245896696));
#35691=CARTESIAN_POINT('Ctrl Pts',(207.981236058459,10.4328365794489,6.18277825102179));
#35692=CARTESIAN_POINT('Ctrl Pts',(208.099709210117,6.23045830133773,10.4044324857287));
#35693=CARTESIAN_POINT('Ctrl Pts',(208.218182361775,0.524917950839583,12.1159104956945));
#35694=CARTESIAN_POINT('Ctrl Pts',(208.336655513434,-5.30726424792321,10.9043006285369));
#35695=CARTESIAN_POINT('Ctrl Pts',(208.455128665092,-9.85901442390833,7.06191621190467));
#35696=CARTESIAN_POINT('Ctrl Pts',(208.57360181675,-12.0321760857944,1.51577196016836));
#35697=CARTESIAN_POINT('Ctrl Pts',(208.692074968408,-11.3024516571717,-4.39606784889534));
#35698=CARTESIAN_POINT('Ctrl Pts',(208.810548120067,-7.84589465310265,-9.24731112741483));
#35699=CARTESIAN_POINT('Ctrl Pts',(208.929021271725,-2.49643496096719,-11.8675455963083));
#35700=CARTESIAN_POINT('Ctrl Pts',(209.047494423383,3.45531531205556,-11.6246127715752));
#35701=CARTESIAN_POINT('Ctrl Pts',(209.165967575042,8.57343526865283,-8.57712269289734));
#35702=CARTESIAN_POINT('Ctrl Pts',(209.2844407267,11.62312588946,-3.46031364944849));
#35703=CARTESIAN_POINT('Ctrl Pts',(209.402913878358,11.8686179819078,2.49133161067114));
#35704=CARTESIAN_POINT('Ctrl Pts',(209.521387030017,9.25068405668635,7.84191752559052));
#35705=CARTESIAN_POINT('Ctrl Pts',(209.639860181675,4.40092756800106,11.3005602753139));
#35706=CARTESIAN_POINT('Ctrl Pts',(209.758333333333,-1.51059790838795,12.0328267648948));
#35707=CARTESIAN_POINT('Ctrl Pts',(209.876806484992,-7.05767612059601,9.86205018094938));
#35708=CARTESIAN_POINT('Ctrl Pts',(209.99527963665,-10.9020174632878,5.31195267533158));
#35709=CARTESIAN_POINT('Ctrl Pts',(210.113752788308,-12.1161350935769,-0.519707984341627));
#35710=CARTESIAN_POINT('Ctrl Pts',(210.232225939967,-10.4071106601961,-6.22598375369127));
#35711=CARTESIAN_POINT('Ctrl Pts',(210.350699091625,-6.18726386497032,-10.4301769812418));
#35712=CARTESIAN_POINT('Ctrl Pts',(210.469172243283,-0.474676098879385,
-12.1179828600286));
#35713=CARTESIAN_POINT('Ctrl Pts',(210.587645394941,5.3524321525426,-10.8822008825064));
#35714=CARTESIAN_POINT('Ctrl Pts',(210.7061185466,9.88821116017542,-7.02097614627605));
#35715=CARTESIAN_POINT('Ctrl Pts',(210.824591698258,12.0383576411386,-1.46586878636295));
#35716=CARTESIAN_POINT('Ctrl Pts',(210.943064849916,11.2841266678616,4.44289447752812));
#35717=CARTESIAN_POINT('Ctrl Pts',(211.061538001575,7.8074842110668,9.27976380565459));
#35718=CARTESIAN_POINT('Ctrl Pts',(211.180011153233,2.44720597994769,11.8777947821346));
#35719=CARTESIAN_POINT('Ctrl Pts',(211.298484304891,-3.50348583464514,11.6101857436148));
#35720=CARTESIAN_POINT('Ctrl Pts',(211.41695745655,-8.60892569936886,8.54150011985839));
#35721=CARTESIAN_POINT('Ctrl Pts',(211.535430608208,-11.6373737972894,3.41208984303704));
#35722=CARTESIAN_POINT('Ctrl Pts',(211.653903759866,-11.8581859127141,-2.54052216174207));
#35723=CARTESIAN_POINT('Ctrl Pts',(211.772376911525,-9.21808885433405,-7.88020709552718));
#35724=CARTESIAN_POINT('Ctrl Pts',(211.890850063183,-4.35403315991698,-11.31871111201));
#35725=CARTESIAN_POINT('Ctrl Pts',(212.009323214841,1.56047776449454,-12.0264597925288));
#35726=CARTESIAN_POINT('Ctrl Pts',(212.1277963665,7.09850739701008,-9.83270149701432));
#35727=CARTESIAN_POINT('Ctrl Pts',(212.246269518158,10.9239491951037,-5.26670295133374));
#35728=CARTESIAN_POINT('Ctrl Pts',(212.364742669816,12.1138760251834,0.569941787625099));
#35729=CARTESIAN_POINT('Ctrl Pts',(212.483215821475,10.3812058150511,6.2690822151527));
#35730=CARTESIAN_POINT('Ctrl Pts',(212.601688973133,6.14396305309261,10.4557421542915));
#35731=CARTESIAN_POINT('Ctrl Pts',(212.720162124791,0.424426085975434,12.1198468840303));
#35732=CARTESIAN_POINT('Ctrl Pts',(212.83863527645,-5.39750803462773,10.85991404252));
#35733=CARTESIAN_POINT('Ctrl Pts',(212.957108428108,-9.91723789181186,6.97991537140715));
#35734=CARTESIAN_POINT('Ctrl Pts',(213.075581579766,-12.0443322251196,1.41594041037714));
#35735=CARTESIAN_POINT('Ctrl Pts',(213.194054731424,-11.2656076744232,-4.48964472099649));
#35736=CARTESIAN_POINT('Ctrl Pts',(213.312527883083,-7.76893953762672,-9.31205694009088));
#35737=CARTESIAN_POINT('Ctrl Pts',(213.431001034741,-2.3979349249532,-11.8878397570999));
#35738=CARTESIAN_POINT('Ctrl Pts',(213.5494741864,3.55159612300168,-11.595559105704));
#35739=CARTESIAN_POINT('Ctrl Pts',(213.667947338058,8.6442681197714,-8.50573069573088));
#35740=CARTESIAN_POINT('Ctrl Pts',(213.786420489716,11.6514216277335,-3.36380737373258));
#35741=CARTESIAN_POINT('Ctrl Pts',(213.904893641374,11.847549969788,2.58966903448489));
#35742=CARTESIAN_POINT('Ctrl Pts',(214.023366793033,9.18533516853456,7.91836118376));
#35743=CARTESIAN_POINT('Ctrl Pts',(214.141839944691,4.30706389443071,11.3366673499793));
#35744=CARTESIAN_POINT('Ctrl Pts',(214.260313096349,-1.61033079184096,12.0198860533552));
#35745=CARTESIAN_POINT('Ctrl Pts',(214.378786248007,-7.1392166312157,9.80318376280727));
#35746=CARTESIAN_POINT('Ctrl Pts',(214.497259399666,-10.9456931151994,5.22136267871434));
#35747=CARTESIAN_POINT('Ctrl Pts',(214.615732551324,-12.1114086870649,-0.620165792094453));
#35748=CARTESIAN_POINT('Ctrl Pts',(214.734205702983,-10.3551224893871,-6.31207289442892));
#35749=CARTESIAN_POINT('Ctrl Pts',(214.852678854641,-6.10055661016068,-10.4811275653443));
#35750=CARTESIAN_POINT('Ctrl Pts',(214.971152006299,-0.374168776059084,
-12.121502535652));
#35751=CARTESIAN_POINT('Ctrl Pts',(215.089625157957,5.44249111920418,-10.837440491748));
#35752=CARTESIAN_POINT('Ctrl Pts',(215.208098309616,9.94609411977095,-6.93873459324197));
#35753=CARTESIAN_POINT('Ctrl Pts',(215.326571461274,12.0500997350184,-1.36598769061246));
#35754=CARTESIAN_POINT('Ctrl Pts',(215.445044612933,11.2468949952473,4.53631777553957));
#35755=CARTESIAN_POINT('Ctrl Pts',(215.563517764591,7.73026129546775,9.3441899755189));
#35756=CARTESIAN_POINT('Ctrl Pts',(215.681990916249,2.34862264308409,11.8976803485044));
#35757=CARTESIAN_POINT('Ctrl Pts',(215.800464067907,-3.59964534998152,11.5807331093136));
#35758=CARTESIAN_POINT('Ctrl Pts',(215.918937219566,-8.67946192223031,8.46981503548623));
#35759=CARTESIAN_POINT('Ctrl Pts',(216.037410371224,-11.6652691392729,3.31546707163905));
#35760=CARTESIAN_POINT('Ctrl Pts',(216.155883522882,-11.8367103359897,-2.63877138393424));
#35761=CARTESIAN_POINT('Ctrl Pts',(216.27435667454,-9.15242356241081,-7.95637913431871));
#35762=CARTESIAN_POINT('Ctrl Pts',(216.392829826199,-4.26002057906886,-11.3544286805063));
#35763=CARTESIAN_POINT('Ctrl Pts',(216.511302977857,1.66015613332113,-12.013105660394));
#35764=CARTESIAN_POINT('Ctrl Pts',(216.629776129516,7.17980312331282,-9.77349748581652));
#35765=CARTESIAN_POINT('Ctrl Pts',(216.748249281174,10.967248849739,-5.17593263699331));
#35766=CARTESIAN_POINT('Ctrl Pts',(216.866722432832,12.1087331216414,0.670379134265463));
#35767=CARTESIAN_POINT('Ctrl Pts',(216.98519558449,10.3288611316458,6.35495505239587));
#35768=CARTESIAN_POINT('Ctrl Pts',(217.103668736149,6.05704528244657,10.5063327779576));
#35769=CARTESIAN_POINT('Ctrl Pts',(217.222141887807,0.323905033186873,12.1229497864287));
#35770=CARTESIAN_POINT('Ctrl Pts',(217.340615039465,-5.48738063289348,10.8147806165701));
#35771=CARTESIAN_POINT('Ctrl Pts',(217.459088191124,-9.97477934793755,6.89743451978729));
#35772=CARTESIAN_POINT('Ctrl Pts',(217.577561342782,-12.055660071676,1.31601148588881));
#35773=CARTESIAN_POINT('Ctrl Pts',(217.69603449444,-11.2279889520545,-4.5829128387235));
#35774=CARTESIAN_POINT('Ctrl Pts',(217.814507646099,-7.69145014957172,-9.37616235948635));
#35775=CARTESIAN_POINT('Ctrl Pts',(217.932980797757,-2.29926998214972,-11.907316387162));
#35776=CARTESIAN_POINT('Ctrl Pts',(218.051453949415,3.64763268949068,-11.5657080093421));
#35777=CARTESIAN_POINT('Ctrl Pts',(218.169927101074,8.71450650167041,-8.43375375660963));
#35778=CARTESIAN_POINT('Ctrl Pts',(218.288400252732,11.6789160938322,-3.26706976785583));
#35779=CARTESIAN_POINT('Ctrl Pts',(218.40687340439,11.8256671976804,2.68782836589246));
#35780=CARTESIAN_POINT('Ctrl Pts',(218.525346556049,9.11935460180238,7.9942602935689));
#35781=CARTESIAN_POINT('Ctrl Pts',(218.643819707707,4.21290402262775,11.3719947982367));
#35782=CARTESIAN_POINT('Ctrl Pts',(218.762292859365,-1.70995293229815,12.0061187301973));
#35783=CARTESIAN_POINT('Ctrl Pts',(218.880766011024,-7.2202661755262,9.74364317647182));
#35784=CARTESIAN_POINT('Ctrl Pts',(218.999239162682,-10.9886160280923,5.13041360714233));
#35785=CARTESIAN_POINT('Ctrl Pts',(219.11771231434,-12.1058493749757,-0.720580950646571));
#35786=CARTESIAN_POINT('Ctrl Pts',(219.236185465999,-10.3024221931989,-6.39772795219415));
#35787=CARTESIAN_POINT('Ctrl Pts',(219.354658617657,-6.01342981829898,-10.5313573579535));
#35788=CARTESIAN_POINT('Ctrl Pts',(219.473131769315,-0.273635720955611,
-12.1241886132193));
#35789=CARTESIAN_POINT('Ctrl Pts',(219.591604920973,5.5321758027325,-10.7919348029323));
#35790=CARTESIAN_POINT('Ctrl Pts',(219.710078072632,10.0032930856283,-6.85601586870224));
#35791=CARTESIAN_POINT('Ctrl Pts',(219.82855122429,12.0610131342887,-1.26601263954867));
#35792=CARTESIAN_POINT('Ctrl Pts',(219.947024375948,11.2088898807694,4.6294290762725));
#35793=CARTESIAN_POINT('Ctrl Pts',(220.065497527607,7.65250674447366,9.40797361163566));
#35794=CARTESIAN_POINT('Ctrl Pts',(220.183970679265,2.24987783814909,11.9167475625392));
#35795=CARTESIAN_POINT('Ctrl Pts',(220.302443830923,-3.69555741573779,11.5504843667932));
#35796=CARTESIAN_POINT('Ctrl Pts',(220.420916982582,-8.74940104823217,8.39754684666139));
#35797=CARTESIAN_POINT('Ctrl Pts',(220.53939013424,-11.6923626900249,3.21861761586706));
#35798=CARTESIAN_POINT('Ctrl Pts',(220.657863285898,-11.8144198395041,-2.73684189791147));
#35799=CARTESIAN_POINT('Ctrl Pts',(220.776336437557,-9.08613074665614,-8.03199824147826));
#35800=CARTESIAN_POINT('Ctrl Pts',(220.894809589215,-4.16571108353903,-11.3893774551249));
#35801=CARTESIAN_POINT('Ctrl Pts',(221.013282740873,1.75971207300965,-11.9989002034899));
#35802=CARTESIAN_POINT('Ctrl Pts',(221.131755892532,7.26062231879625,-9.71367402572911));
#35803=CARTESIAN_POINT('Ctrl Pts',(221.25022904419,11.0097579792252,-5.0846969330813));
#35804=CARTESIAN_POINT('Ctrl Pts',(221.368702195848,12.1028300703176,0.770534222877572));
#35805=CARTESIAN_POINT('Ctrl Pts',(221.487175347506,10.2756235996193,6.44082954989814));
#35806=CARTESIAN_POINT('Ctrl Pts',(221.566157448612,7.40502905753358,9.18315595905444));
#35807=CARTESIAN_POINT('Ctrl Pts',(221.605648499165,5.72918237190977,10.1308757356854));
#35808=CARTESIAN_POINT('Ctrl Pts',(204.,-5.12964461189134,10.7653319110789));
#35809=CARTESIAN_POINT('Ctrl Pts',(204.039491050553,-6.91044286403785,9.91678750627633));
#35810=CARTESIAN_POINT('Ctrl Pts',(204.118473151658,-10.041010738167,7.31961918275114));
#35811=CARTESIAN_POINT('Ctrl Pts',(204.236946303317,-12.3149962203278,1.65500982268089));
#35812=CARTESIAN_POINT('Ctrl Pts',(204.355419454975,-11.6174391675063,-4.40792773774884));
#35813=CARTESIAN_POINT('Ctrl Pts',(204.473892606633,-8.11724710747811,-9.40788837704011));
#35814=CARTESIAN_POINT('Ctrl Pts',(204.592365758292,-2.65859298868677,-12.1378723750666));
#35815=CARTESIAN_POINT('Ctrl Pts',(204.71083890995,3.44142969382895,-11.9395788323205));
#35816=CARTESIAN_POINT('Ctrl Pts',(204.829312061608,8.71119332437167,-8.86068716323123));
#35817=CARTESIAN_POINT('Ctrl Pts',(204.947785213267,11.8792819197844,-3.64408861344167));
#35818=CARTESIAN_POINT('Ctrl Pts',(205.066258364925,12.1813765724026,2.4516956802784));
#35819=CARTESIAN_POINT('Ctrl Pts',(205.184731516583,9.54458665860898,7.9559774948088));
#35820=CARTESIAN_POINT('Ctrl Pts',(205.303204668241,4.60506827239925,11.5408007373264));
#35821=CARTESIAN_POINT('Ctrl Pts',(205.4216778199,-1.44547067637712,12.3412859323907));
#35822=CARTESIAN_POINT('Ctrl Pts',(205.540150971558,-7.14727471979692,10.1643097367997));
#35823=CARTESIAN_POINT('Ctrl Pts',(205.658624123217,-11.1247254332009,5.53508909692871));
#35824=CARTESIAN_POINT('Ctrl Pts',(205.777097274875,-12.4182217901181,-0.429528507676729));
#35825=CARTESIAN_POINT('Ctrl Pts',(205.895570426533,-10.715694592358,-6.2905180157606));
#35826=CARTESIAN_POINT('Ctrl Pts',(206.014043578191,-6.42789597557465,-10.6338553955023));
#35827=CARTESIAN_POINT('Ctrl Pts',(206.13251672985,-0.589301425566469,-12.4116659323139));
#35828=CARTESIAN_POINT('Ctrl Pts',(206.250989881508,5.39146815047745,-11.1950345470193));
#35829=CARTESIAN_POINT('Ctrl Pts',(206.369463033166,10.0714906457364,-7.27748607122799));
#35830=CARTESIAN_POINT('Ctrl Pts',(206.487936184825,12.3216625562562,-1.60416931544008));
#35831=CARTESIAN_POINT('Ctrl Pts',(206.606409336483,11.5991067909594,4.45616976693988));
#35832=CARTESIAN_POINT('Ctrl Pts',(206.724882488141,8.07814735173198,9.44141211399871));
#35833=CARTESIAN_POINT('Ctrl Pts',(206.8433556398,2.60825187482188,12.1488167941771));
#35834=CARTESIAN_POINT('Ctrl Pts',(206.961828791458,-3.49091116213162,11.9251946147582));
#35835=CARTESIAN_POINT('Ctrl Pts',(207.080301943116,-8.74785601816062,8.82449672372453));
#35836=CARTESIAN_POINT('Ctrl Pts',(207.198775094774,-11.8942907407006,3.5947983416629));
#35837=CARTESIAN_POINT('Ctrl Pts',(207.317248246433,-12.1711056287734,-2.50218207067393));
#35838=CARTESIAN_POINT('Ctrl Pts',(207.435721398091,-9.51151624683086,-7.99548535286034));
#35839=CARTESIAN_POINT('Ctrl Pts',(207.554194549749,-4.55717585595323,-11.5597956538802));
#35840=CARTESIAN_POINT('Ctrl Pts',(207.672667701408,1.49663002727809,-12.335186496482));
#35841=CARTESIAN_POINT('Ctrl Pts',(207.791140853066,7.18935854114184,-10.1345868740889));
#35842=CARTESIAN_POINT('Ctrl Pts',(207.909614004724,11.1475804487235,-5.48891405295993));
#35843=CARTESIAN_POINT('Ctrl Pts',(208.028087156383,12.4163340509309,0.481015672549472));
#35844=CARTESIAN_POINT('Ctrl Pts',(208.146560308041,10.6895195069813,6.33489542545181));
#35845=CARTESIAN_POINT('Ctrl Pts',(208.265033459699,6.38374856563713,10.6604165768637));
#35846=CARTESIAN_POINT('Ctrl Pts',(208.383506611358,0.537832700851228,12.4140027117541));
#35847=CARTESIAN_POINT('Ctrl Pts',(208.501979763016,-5.43784082831635,11.1725831600145));
#35848=CARTESIAN_POINT('Ctrl Pts',(208.620452914674,-10.1015793932378,7.23566314194201));
#35849=CARTESIAN_POINT('Ctrl Pts',(208.738926066333,-12.3282081532736,1.55306505694456));
#35850=CARTESIAN_POINT('Ctrl Pts',(208.857399217991,-11.5805300453036,-4.50422592809963));
#35851=CARTESIAN_POINT('Ctrl Pts',(208.975872369649,-8.03893009397561,-9.47482613485428));
#35852=CARTESIAN_POINT('Ctrl Pts',(209.094345521308,-2.55785567136515,-12.1595271991147));
#35853=CARTESIAN_POINT('Ctrl Pts',(209.212818672966,3.54032770950775,-11.9106174084653));
#35854=CARTESIAN_POINT('Ctrl Pts',(209.331291824624,8.78437065971439,-8.78814880701806));
#35855=CARTESIAN_POINT('Ctrl Pts',(209.449764976283,11.9090939440408,-3.54544902283972));
#35856=CARTESIAN_POINT('Ctrl Pts',(209.568238127941,12.1606259690128,2.55262676145886));
#35857=CARTESIAN_POINT('Ctrl Pts',(209.686711279599,9.47828204954912,8.03485511572791));
#35858=CARTESIAN_POINT('Ctrl Pts',(209.805184431257,4.50920521266752,11.5785921290801));
#35859=CARTESIAN_POINT('Ctrl Pts',(209.923657582916,-1.54776370605922,12.328874841272));
#35860=CARTESIAN_POINT('Ctrl Pts',(210.042130734574,-7.23131873010248,10.1046898401293));
#35861=CARTESIAN_POINT('Ctrl Pts',(210.160603886232,-11.1702438212084,5.44264460683406));
#35862=CARTESIAN_POINT('Ctrl Pts',(210.279077037891,-12.4142328355011,-0.532494551625294));
#35863=CARTESIAN_POINT('Ctrl Pts',(210.397550189549,-10.6631606434456,-6.37916392904402));
#35864=CARTESIAN_POINT('Ctrl Pts',(210.516023341207,-6.3394914006153,-10.6867944736983));
#35865=CARTESIAN_POINT('Ctrl Pts',(210.634496492866,-0.486354730070657,
-12.4161260632325));
#35866=CARTESIAN_POINT('Ctrl Pts',(210.752969644524,5.48412001555769,-11.1499396857787));
#35867=CARTESIAN_POINT('Ctrl Pts',(210.871442796182,10.1314944675793,-7.193715812774));
#35868=CARTESIAN_POINT('Ctrl Pts',(210.989915947841,12.3345417957047,-1.50193409694237));
#35869=CARTESIAN_POINT('Ctrl Pts',(211.108389099499,11.5617541995205,4.55220464955323));
#35870=CARTESIAN_POINT('Ctrl Pts',(211.226862251157,7.99957462566292,9.5080772583101));
#35871=CARTESIAN_POINT('Ctrl Pts',(211.345335402815,2.50741549156271,12.1700285494413));
#35872=CARTESIAN_POINT('Ctrl Pts',(211.463808554474,-3.58968338923699,11.8958354270131));
#35873=CARTESIAN_POINT('Ctrl Pts',(211.582281706132,-8.82073427459143,8.75164979867179));
#35874=CARTESIAN_POINT('Ctrl Pts',(211.700754857791,-11.9236923984033,3.49603874832707));
#35875=CARTESIAN_POINT('Ctrl Pts',(211.819228009449,-12.1499372357718,-2.60302756580651));
#35876=CARTESIAN_POINT('Ctrl Pts',(211.937701161107,-9.44488489540743,-8.07408673808059));
#35877=CARTESIAN_POINT('Ctrl Pts',(212.056174312765,-4.46115704415977,-11.5971895375081));
#35878=CARTESIAN_POINT('Ctrl Pts',(212.174647464424,1.59887077466865,-12.3223512199359));
#35879=CARTESIAN_POINT('Ctrl Pts',(212.293120616082,7.27315459347477,-10.0746190796953));
#35880=CARTESIAN_POINT('Ctrl Pts',(212.41159376774,11.1927151475138,-5.39628158718193));
#35881=CARTESIAN_POINT('Ctrl Pts',(212.530066919399,12.4119181864144,0.583964275704583));
#35882=CARTESIAN_POINT('Ctrl Pts',(212.648540071057,10.636618451838,6.42332275785386));
#35883=CARTESIAN_POINT('Ctrl Pts',(212.767013222715,6.29512524288724,10.7129886361327));
#35884=CARTESIAN_POINT('Ctrl Pts',(212.885486374374,0.434868397559615,12.4180359485044));
#35885=CARTESIAN_POINT('Ctrl Pts',(213.003959526032,-5.53030491620038,11.1271045144455));
#35886=CARTESIAN_POINT('Ctrl Pts',(213.12243267769,-10.1612353546035,7.15164480451173));
#35887=CARTESIAN_POINT('Ctrl Pts',(213.240905829348,-12.3406633745797,1.45077731470124));
#35888=CARTESIAN_POINT('Ctrl Pts',(213.359378981007,-11.542779576454,-4.60010510651003));
#35889=CARTESIAN_POINT('Ctrl Pts',(213.477852132665,-7.96008162340124,-9.5411649126474));
#35890=CARTESIAN_POINT('Ctrl Pts',(213.596325284324,-2.45693220262376,-12.1803206646317));
#35891=CARTESIAN_POINT('Ctrl Pts',(213.714798435982,3.63897735276813,-11.8808489245333));
#35892=CARTESIAN_POINT('Ctrl Pts',(213.83327158764,8.85694623760263,-8.71500032620544));
#35893=CARTESIAN_POINT('Ctrl Pts',(213.951744739299,11.9380858528027,-3.44656836761662));
#35894=CARTESIAN_POINT('Ctrl Pts',(214.070217890957,12.1390396128179,2.65338361719204));
#35895=CARTESIAN_POINT('Ctrl Pts',(214.188691042615,9.41132535859182,8.11317954542305));
#35896=CARTESIAN_POINT('Ctrl Pts',(214.307164194273,4.41303217650556,11.6155875594251));
#35897=CARTESIAN_POINT('Ctrl Pts',(214.425637345932,-1.64995035444002,12.315615744632));
#35898=CARTESIAN_POINT('Ctrl Pts',(214.54411049759,-7.31486541198911,10.0443751097831));
#35899=CARTESIAN_POINT('Ctrl Pts',(214.662583649248,-11.214994041298,5.3498257911071));
#35900=CARTESIAN_POINT('Ctrl Pts',(214.781056800907,-12.4093901434658,-0.635423959885912));
#35901=CARTESIAN_POINT('Ctrl Pts',(214.899529952565,-10.6098933884893,-6.46737115267362));
#35902=CARTESIAN_POINT('Ctrl Pts',(215.018003104223,-6.25065085522515,-10.7389986138195));
#35903=CARTESIAN_POINT('Ctrl Pts',(215.136476255882,-0.383374588505087,
-12.4197323347338));
#35904=CARTESIAN_POINT('Ctrl Pts',(215.25494940754,5.57639473620306,-11.1040780386123));
#35905=CARTESIAN_POINT('Ctrl Pts',(215.373422559198,10.1908015429855,-7.1094508404678));
#35906=CARTESIAN_POINT('Ctrl Pts',(215.491895710857,12.3465727846524,-1.39959558974226));
#35907=CARTESIAN_POINT('Ctrl Pts',(215.610368862515,11.5236065023283,4.64792647543395));
#35908=CARTESIAN_POINT('Ctrl Pts',(215.728842014173,7.92045176618019,9.57408852900145));
#35909=CARTESIAN_POINT('Ctrl Pts',(215.847315165832,2.40640667249019,12.1904033677372));
#35910=CARTESIAN_POINT('Ctrl Pts',(215.96578831749,-3.68820875260699,11.8656581586837));
#35911=CARTESIAN_POINT('Ctrl Pts',(216.084261469148,-8.8930059261681,8.67820101972081));
#35912=CARTESIAN_POINT('Ctrl Pts',(216.202734620806,-11.9522740597775,3.39703873123564));
#35913=CARTESIAN_POINT('Ctrl Pts',(216.321207772465,-12.1279332875099,-2.70369404986107));
#35914=CARTESIAN_POINT('Ctrl Pts',(216.439680924123,-9.37760401607995,-8.15213286564597));
#35915=CARTESIAN_POINT('Ctrl Pts',(216.558154075782,-4.36483143709935,-11.6337858785201));
#35916=CARTESIAN_POINT('Ctrl Pts',(216.67662722744,1.70100156717955,-12.3086685311612));
#35917=CARTESIAN_POINT('Ctrl Pts',(216.795100379098,7.35645046852558,-10.0139584503668));
#35918=CARTESIAN_POINT('Ctrl Pts',(216.913573530756,11.2370801195274,-5.30327801730832));
#35919=CARTESIAN_POINT('Ctrl Pts',(217.032046682415,12.4066487501191,0.686872719440438));
#35920=CARTESIAN_POINT('Ctrl Pts',(217.150519834073,10.5829859128744,6.51130835619429));
#35921=CARTESIAN_POINT('Ctrl Pts',(217.268992985731,6.20606900226191,10.7648239595782));
#35922=CARTESIAN_POINT('Ctrl Pts',(217.38746613739,0.331874188222308,12.4212151927553));
#35923=CARTESIAN_POINT('Ctrl Pts',(217.505939289048,-5.62238868315952,11.0808606541651));
#35924=CARTESIAN_POINT('Ctrl Pts',(217.624412440706,-10.220192524404,7.06713464606836));
#35925=CARTESIAN_POINT('Ctrl Pts',(217.742885592365,-12.3522699243242,1.3483898020152));
#35926=CARTESIAN_POINT('Ctrl Pts',(217.861358744023,-11.5042353067796,-4.69566793414851));
#35927=CARTESIAN_POINT('Ctrl Pts',(217.979831895681,-7.8806857353424,-9.60684754132778));
#35928=CARTESIAN_POINT('Ctrl Pts',(218.098305047339,-2.35583976983032,-12.2002764854091));
#35929=CARTESIAN_POINT('Ctrl Pts',(218.216778198998,3.73737674233492,-11.8502633906342));
#35930=CARTESIAN_POINT('Ctrl Pts',(218.335251350656,8.92891272032577,-8.64125251189527));
#35931=CARTESIAN_POINT('Ctrl Pts',(218.453724502314,11.9662567753948,-3.34745069073139));
#35932=CARTESIAN_POINT('Ctrl Pts',(218.572197653973,12.1166184507944,2.75395799884586));
#35933=CARTESIAN_POINT('Ctrl Pts',(218.690670805631,9.34372144763298,8.19094602903335));
#35934=CARTESIAN_POINT('Ctrl Pts',(218.80914395729,4.31655565463659,11.6517841819259));
#35935=CARTESIAN_POINT('Ctrl Pts',(218.927617108948,-1.75202353517421,12.301509698943));
#35936=CARTESIAN_POINT('Ctrl Pts',(219.046090260606,-7.39790904814131,9.98336962443466));
#35937=CARTESIAN_POINT('Ctrl Pts',(219.164563412264,-11.2589730024531,5.25663906597177));
#35938=CARTESIAN_POINT('Ctrl Pts',(219.283036563923,-12.4036940535703,-0.738309669631802));
#35939=CARTESIAN_POINT('Ctrl Pts',(219.401509715581,-10.5558964874704,-6.55513361342726));
#35940=CARTESIAN_POINT('Ctrl Pts',(219.519982867239,-6.16138045075807,-10.7904642285485));
#35941=CARTESIAN_POINT('Ctrl Pts',(219.638456018898,-0.28036808155549,-12.4224844988586));
#35942=CARTESIAN_POINT('Ctrl Pts',(219.756929170556,5.66828596508916,-11.0574527565455));
#35943=CARTESIAN_POINT('Ctrl Pts',(219.875402322214,10.2494077961033,-7.02469695662936));
#35944=CARTESIAN_POINT('Ctrl Pts',(219.993875473873,12.3577546903114,-1.29716081561161));
#35945=CARTESIAN_POINT('Ctrl Pts',(220.112348625531,11.4846663339971,4.74332862785197));
#35946=CARTESIAN_POINT('Ctrl Pts',(220.230821777189,7.84078419128066,9.6394414574504));
#35947=CARTESIAN_POINT('Ctrl Pts',(220.349294928848,2.30523241268773,12.2099396994737));
#35948=CARTESIAN_POINT('Ctrl Pts',(220.467768080506,-3.78648057830359,11.8346651951909));
#35949=CARTESIAN_POINT('Ctrl Pts',(220.586241232164,-8.96466579029084,8.60415478998313));
#35950=CARTESIAN_POINT('Ctrl Pts',(220.704714383822,-11.9800342031547,3.29780645257095));
#35951=CARTESIAN_POINT('Ctrl Pts',(220.823187535481,-12.1050943697152,-2.80417742887655));
#35952=CARTESIAN_POINT('Ctrl Pts',(220.941660687139,-9.30968017372072,-8.22961245759845));
#35953=CARTESIAN_POINT('Ctrl Pts',(221.060133838797,-4.26820161025575,-11.6695945107349));
#35954=CARTESIAN_POINT('Ctrl Pts',(221.178606990456,1.80300691838314,-12.2941135721597));
#35955=CARTESIAN_POINT('Ctrl Pts',(221.297080142114,7.43925808849352,-9.95266313161919));
#35956=CARTESIAN_POINT('Ctrl Pts',(221.415553293772,11.2806351168099,-5.20979760771178));
#35957=CARTESIAN_POINT('Ctrl Pts',(221.534026445431,12.4006004638457,0.789491960649636));
#35958=CARTESIAN_POINT('Ctrl Pts',(221.652499597089,10.5284385582057,6.59929565564178));
#35959=CARTESIAN_POINT('Ctrl Pts',(221.731481698195,7.58721771950252,9.40909253321683));
#35960=CARTESIAN_POINT('Ctrl Pts',(221.770972748747,5.87013955957299,10.380129409171));
#35961=CARTESIAN_POINT('Ctrl Pts',(220.768843152848,-11.9240373570162,-7.43698370121595E-5));
#35962=CARTESIAN_POINT('Ctrl Pts',(220.786957947059,-11.924234503617,-0.905127068583988));
#35963=CARTESIAN_POINT('Ctrl Pts',(220.80507274127,-11.8225000180031,-1.81013598156214));
#35964=CARTESIAN_POINT('Ctrl Pts',(220.823187535481,-11.6183486426227,-2.69141928675563));
#35965=CARTESIAN_POINT('Ctrl Pts',(220.862678586033,-11.1732896377171,-4.61265577178385));
#35966=CARTESIAN_POINT('Ctrl Pts',(220.902169636586,-10.2414849057189,-6.42113411469115));
#35967=CARTESIAN_POINT('Ctrl Pts',(220.941660687139,-8.93533611247564,-7.89870362833421));
#35968=CARTESIAN_POINT('Ctrl Pts',(220.981151737692,-7.6291873192324,-9.37627314197726));
#35969=CARTESIAN_POINT('Ctrl Pts',(221.020642788245,-5.94869446474407,-10.5229338263561));
#35970=CARTESIAN_POINT('Ctrl Pts',(221.060133838797,-4.09657994939343,-11.200350678783));
#35971=CARTESIAN_POINT('Ctrl Pts',(221.09962488935,-2.24446543404284,-11.8777675312098));
#35972=CARTESIAN_POINT('Ctrl Pts',(221.139115939903,-0.220729257829941,
-12.0859405516848));
#35973=CARTESIAN_POINT('Ctrl Pts',(221.178606990456,1.73051402529489,-11.7997853218322));
#35974=CARTESIAN_POINT('Ctrl Pts',(221.210737993637,3.31809914294103,-11.5669615688028));
#35975=CARTESIAN_POINT('Ctrl Pts',(221.242868996819,4.85769471604154,-11.0068976329263));
#35976=CARTESIAN_POINT('Ctrl Pts',(221.275,6.22722261202592,-10.1702729013571));
#35977=CARTESIAN_POINT('Ctrl Pts',(204.,-6.42465676560637,-9.01028147758817));
#35978=CARTESIAN_POINT('Ctrl Pts',(204.032131003181,-5.21120775505585,-9.87363627182968));
#35979=CARTESIAN_POINT('Ctrl Pts',(204.103753056916,-2.11541440506495,-11.252056127613));
#35980=CARTESIAN_POINT('Ctrl Pts',(204.214866161202,3.19351689060185,-11.0794786062488));
#35981=CARTESIAN_POINT('Ctrl Pts',(204.333339312861,8.08365868074054,-8.22238332192522));
#35982=CARTESIAN_POINT('Ctrl Pts',(204.451812464519,11.0235253467705,-3.38157672049597));
#35983=CARTESIAN_POINT('Ctrl Pts',(204.570285616177,11.303857784602,2.27508107448027));
#35984=CARTESIAN_POINT('Ctrl Pts',(204.688758767836,8.85701624610765,7.38284688961676));
#35985=CARTESIAN_POINT('Ctrl Pts',(204.807231919494,4.27332958062524,10.7094275823243));
#35986=CARTESIAN_POINT('Ctrl Pts',(204.925705071152,-1.34134224161475,11.4522476363554));
#35987=CARTESIAN_POINT('Ctrl Pts',(205.044178222811,-6.63240123149158,9.43209587689214));
#35988=CARTESIAN_POINT('Ctrl Pts',(205.15990000046,-10.2376088257201,5.23611643961605));
#35989=CARTESIAN_POINT('Ctrl Pts',(205.236130727557,-11.0657697006446,1.70247381065806));
#35990=CARTESIAN_POINT('Ctrl Pts',(205.272870404101,-11.066766136903,-0.000127008754821131));
#35991=CARTESIAN_POINT('Origin',(201.227129595899,0.,0.));
#35992=CARTESIAN_POINT('Ctrl Pts',(204.,6.42428395783811,-9.01020671414169));
#35993=CARTESIAN_POINT('Ctrl Pts',(204.039491050553,7.91474988128163,-7.9475034238105));
#35994=CARTESIAN_POINT('Ctrl Pts',(204.118473151658,10.3565945407743,-5.06910807865537));
#35995=CARTESIAN_POINT('Ctrl Pts',(204.236946303317,11.5208305663343,0.474233997127887));
#35996=CARTESIAN_POINT('Ctrl Pts',(204.355419454975,9.90531651320884,5.90221595067179));
#35997=CARTESIAN_POINT('Ctrl Pts',(204.473892606633,5.90014038006902,9.90669837751048));
#35998=CARTESIAN_POINT('Ctrl Pts',(204.592365758292,0.471446650502101,11.5208655173499));
#35999=CARTESIAN_POINT('Ctrl Pts',(204.71083890995,-5.07096553594642,10.3556122261992));
#36000=CARTESIAN_POINT('Ctrl Pts',(204.829312061608,-9.38996616253539,6.69191003627886));
#36001=CARTESIAN_POINT('Ctrl Pts',(204.918075623591,-10.9285607524451,2.73735033409805));
#36002=CARTESIAN_POINT('Ctrl Pts',(204.967348135022,-11.0663132288553,0.45368304064905));
#36003=CARTESIAN_POINT('Ctrl Pts',(204.977129595899,-11.0658620952239,0.000280741946515339));
#36004=CARTESIAN_POINT('Ctrl Pts',(203.504027251253,6.92300129651942,-9.70966930685028));
#36005=CARTESIAN_POINT('Ctrl Pts',(203.543518301805,8.52917213020871,-8.56446833113655));
#36006=CARTESIAN_POINT('Ctrl Pts',(203.622500402911,11.1605772571476,-5.46262307691302));
#36007=CARTESIAN_POINT('Ctrl Pts',(203.740973554569,12.4151929570924,0.511048795245736));
#36008=CARTESIAN_POINT('Ctrl Pts',(203.859446706228,10.6742665040069,6.36040513573264));
#36009=CARTESIAN_POINT('Ctrl Pts',(203.977919857886,6.35816843852751,10.6757556424719));
#36010=CARTESIAN_POINT('Ctrl Pts',(204.096393009544,0.508045066825541,12.4152306213563));
#36011=CARTESIAN_POINT('Ctrl Pts',(204.214866161202,-5.46462472866412,11.1595186854654));
#36012=CARTESIAN_POINT('Ctrl Pts',(204.333339312861,-10.1189094915696,7.21140319472127));
#36013=CARTESIAN_POINT('Ctrl Pts',(204.451812464519,-12.3318977278251,1.52348893979719));
#36014=CARTESIAN_POINT('Ctrl Pts',(204.570285616177,-11.5696916564292,-4.53199528109509));
#36015=CARTESIAN_POINT('Ctrl Pts',(204.688758767836,-8.01617731810691,-9.49408304713466));
#36016=CARTESIAN_POINT('Ctrl Pts',(204.807231919494,-2.52867846986942,-12.1656286313568));
#36017=CARTESIAN_POINT('Ctrl Pts',(204.925705071153,3.56889033400025,-11.9020899448289));
#36018=CARTESIAN_POINT('Ctrl Pts',(205.044178222811,8.80542753846537,-8.76705044750802));
#36019=CARTESIAN_POINT('Ctrl Pts',(205.162651374469,11.9175649567678,-3.51686964666669));
#36020=CARTESIAN_POINT('Ctrl Pts',(205.281124526127,12.1544673643034,2.58179193456698));
#36021=CARTESIAN_POINT('Ctrl Pts',(205.399597677786,9.45897966964662,8.05756976071132));
#36022=CARTESIAN_POINT('Ctrl Pts',(205.518070829444,4.48141594756073,11.5893760697451));
#36023=CARTESIAN_POINT('Ctrl Pts',(205.636543981102,-1.57733540710525,12.325126357774));
#36024=CARTESIAN_POINT('Ctrl Pts',(205.755017132761,-7.25553839212175,10.0873132846628));
#36025=CARTESIAN_POINT('Ctrl Pts',(205.873490284419,-11.1832682011054,5.41583225572877));
#36026=CARTESIAN_POINT('Ctrl Pts',(205.991963436077,-12.4129196682143,-0.562273945038027));
#36027=CARTESIAN_POINT('Ctrl Pts',(206.110436587736,-10.647826743886,-6.40472577929877));
#36028=CARTESIAN_POINT('Ctrl Pts',(206.228909739394,-6.31383622967067,-10.7019717222351));
#36029=CARTESIAN_POINT('Ctrl Pts',(206.347382891052,-0.456567861250994,
-12.4172570427219));
#36030=CARTESIAN_POINT('Ctrl Pts',(206.46585604271,5.51085219412049,-11.1367515358957));
#36031=CARTESIAN_POINT('Ctrl Pts',(206.584329194369,10.1487225431899,-7.16939031011746));
#36032=CARTESIAN_POINT('Ctrl Pts',(206.702802346027,12.3381093181286,-1.4723400189527));
#36033=CARTESIAN_POINT('Ctrl Pts',(206.821275497686,11.5508004673251,4.57992742754356));
#36034=CARTESIAN_POINT('Ctrl Pts',(206.939748649344,7.97674233926988,9.52724033130231));
#36035=CARTESIAN_POINT('Ctrl Pts',(207.058221801002,2.47821317462715,12.1760086292109));
#36036=CARTESIAN_POINT('Ctrl Pts',(207.17669495266,-3.61821037775123,11.8871897578796));
#36037=CARTESIAN_POINT('Ctrl Pts',(207.295168104319,-8.84170350563972,8.73046423713344));
#36038=CARTESIAN_POINT('Ctrl Pts',(207.413641255977,-11.9320448295726,3.46742452874975));
#36039=CARTESIAN_POINT('Ctrl Pts',(207.532114407635,-12.1436577572359,-2.63216696898803));
#36040=CARTESIAN_POINT('Ctrl Pts',(207.650587559294,-9.42548849587364,-8.09672114449177));
#36041=CARTESIAN_POINT('Ctrl Pts',(207.769060710952,-4.43332330428022,-11.6078581640728));
#36042=CARTESIAN_POINT('Ctrl Pts',(207.88753386261,1.62842667920446,-12.3184801508937));
#36043=CARTESIAN_POINT('Ctrl Pts',(208.006007014269,7.29730199706176,-10.0571422502212));
#36044=CARTESIAN_POINT('Ctrl Pts',(208.124480165927,11.2056282409638,-5.36941546193074));
#36045=CARTESIAN_POINT('Ctrl Pts',(208.242953317585,12.4104815532728,0.613737968013001));
#36046=CARTESIAN_POINT('Ctrl Pts',(208.361426469244,10.6211786946092,6.44882080807686));
#36047=CARTESIAN_POINT('Ctrl Pts',(208.479899620902,6.26940736161951,10.7280593777056));
#36048=CARTESIAN_POINT('Ctrl Pts',(208.59837277256,0.405077095315529,12.419043410197));
#36049=CARTESIAN_POINT('Ctrl Pts',(208.716845924218,-5.55698218170029,11.1138056357744));
#36050=CARTESIAN_POINT('Ctrl Pts',(208.835319075877,-10.1783624189946,7.12724807657941));
#36051=CARTESIAN_POINT('Ctrl Pts',(208.953792227535,-12.3441081576266,1.42116869875556));
#36052=CARTESIAN_POINT('Ctrl Pts',(209.072265379193,-11.5317109888576,-4.6277822276949));
#36053=CARTESIAN_POINT('Ctrl Pts',(209.190738530852,-7.93717007562952,-9.560233149251));
#36054=CARTESIAN_POINT('Ctrl Pts',(209.30921168251,-2.42770534095333,-12.1861796086802));
#36055=CARTESIAN_POINT('Ctrl Pts',(209.427684834168,3.66746824770378,-11.8720850455845));
#36056=CARTESIAN_POINT('Ctrl Pts',(209.546157985827,8.87782744470561,-8.69372800008941));
#36057=CARTESIAN_POINT('Ctrl Pts',(209.664631137485,11.9463195663411,-3.41791976154524));
#36058=CARTESIAN_POINT('Ctrl Pts',(209.783104289143,12.1326393648134,2.68249673268913));
#36059=CARTESIAN_POINT('Ctrl Pts',(209.901577440802,9.391835274627,8.1357333321452));
#36060=CARTESIAN_POINT('Ctrl Pts',(210.02005059246,4.38515443956386,11.6261406846245));
#36061=CARTESIAN_POINT('Ctrl Pts',(210.138523744118,-1.6794899539259,12.3116221584391));
#36062=CARTESIAN_POINT('Ctrl Pts',(210.256996895776,-7.33894014217483,10.0267983058941));
#36063=CARTESIAN_POINT('Ctrl Pts',(210.375470047435,-11.2277956262,5.32290635403163));
#36064=CARTESIAN_POINT('Ctrl Pts',(210.493943199093,-12.4078300692124,-0.665191439402797));
#36065=CARTESIAN_POINT('Ctrl Pts',(210.612416350752,-10.5943480390211,-6.49280496438909));
#36066=CARTESIAN_POINT('Ctrl Pts',(210.73088950241,-6.22487070580297,-10.7539625893687));
#36067=CARTESIAN_POINT('Ctrl Pts',(210.849362654068,-0.353579365023488,
-12.4206162612866));
#36068=CARTESIAN_POINT('Ctrl Pts',(210.967835805727,5.60301662998475,-11.0906686598068));
#36069=CARTESIAN_POINT('Ctrl Pts',(211.086308957385,10.2078273016985,-7.08498330669916));
#36070=CARTESIAN_POINT('Ctrl Pts',(211.204782109043,12.3498947690968,-1.36997294489374));
#36071=CARTESIAN_POINT('Ctrl Pts',(211.323255260701,11.5124232496295,4.67555746397121));
#36072=CARTESIAN_POINT('Ctrl Pts',(211.44172841236,7.89746135094013,9.59306160138219));
#36073=CARTESIAN_POINT('Ctrl Pts',(211.560201564018,2.37715576857242,12.196141075334));
#36074=CARTESIAN_POINT('Ctrl Pts',(211.678674715676,-3.71666306412984,11.8567762205938));
#36075=CARTESIAN_POINT('Ctrl Pts',(211.797147867335,-8.91379875032231,8.65684229475499));
#36076=CARTESIAN_POINT('Ctrl Pts',(211.915621018993,-11.9603889141255,3.36835623121586));
#36077=CARTESIAN_POINT('Ctrl Pts',(212.034094170651,-12.1214123800741,-2.7327803771419));
#36078=CARTESIAN_POINT('Ctrl Pts',(212.15256732231,-9.35802058277042,-8.17460564491962));
#36079=CARTESIAN_POINT('Ctrl Pts',(212.271040473968,-4.33691018238782,-11.6442233209179));
#36080=CARTESIAN_POINT('Ctrl Pts',(212.389513625626,1.73052435375133,-12.3045524964779));
#36081=CARTESIAN_POINT('Ctrl Pts',(212.507986777285,7.38045211140153,-9.99628197425497));
#36082=CARTESIAN_POINT('Ctrl Pts',(212.626459928943,11.2497699757883,-5.27630573122507));
#36083=CARTESIAN_POINT('Ctrl Pts',(212.744933080601,12.4049652615757,0.716633474383855));
#36084=CARTESIAN_POINT('Ctrl Pts',(212.86340623226,10.5673352384327,6.53667749212747));
#36085=CARTESIAN_POINT('Ctrl Pts',(212.981879383918,6.18022702791458,10.7796809118332));
#36086=CARTESIAN_POINT('Ctrl Pts',(213.100352535576,0.302075555762362,12.4219755689712));
#36087=CARTESIAN_POINT('Ctrl Pts',(213.218825687234,-5.64895474752174,11.0673410057682));
#36088=CARTESIAN_POINT('Ctrl Pts',(213.337298838893,-10.2371166847208,7.04259672712543));
#36089=CARTESIAN_POINT('Ctrl Pts',(213.455771990551,-12.3554690530526,1.31875363755592));
#36090=CARTESIAN_POINT('Ctrl Pts',(213.57424514221,-11.4929375812482,-4.72325231498802));
#36091=CARTESIAN_POINT('Ctrl Pts',(213.692718293868,-7.85761684790037,-9.62572512328807));
#36092=CARTESIAN_POINT('Ctrl Pts',(213.811191445526,-2.32656532656588,-12.2058928579079));
#36093=CARTESIAN_POINT('Ctrl Pts',(213.929664597184,3.76579398123967,-11.8412635461071));
#36094=CARTESIAN_POINT('Ctrl Pts',(214.048137748843,8.94961680404746,-8.6198077552935));
#36095=CARTESIAN_POINT('Ctrl Pts',(214.166610900501,11.9742526310362,-3.31873478989055));
#36096=CARTESIAN_POINT('Ctrl Pts',(214.285084052159,12.1099769960399,2.78301703783682));
#36097=CARTESIAN_POINT('Ctrl Pts',(214.403557203818,9.32404500166837,8.21333741449657));
#36098=CARTESIAN_POINT('Ctrl Pts',(214.522030355476,4.2885913621992,11.6621057620645));
#36099=CARTESIAN_POINT('Ctrl Pts',(214.640503507134,-1.78152900126369,12.2972712865563));
#36100=CARTESIAN_POINT('Ctrl Pts',(214.758976658793,-7.42183719104071,9.9655937799607));
#36101=CARTESIAN_POINT('Ctrl Pts',(214.877449810451,-11.2715509119312,5.22961439469969));
#36102=CARTESIAN_POINT('Ctrl Pts',(214.995922962109,-12.4018871796163,-0.768063188530766));
#36103=CARTESIAN_POINT('Ctrl Pts',(215.114396113768,-10.5401407572657,-6.58043763700659));
#36104=CARTESIAN_POINT('Ctrl Pts',(215.232869265426,-6.13547709549785,-10.8052139029326));
#36105=CARTESIAN_POINT('Ctrl Pts',(215.351342417084,-0.25056655301961,-12.4231213098808));
#36106=CARTESIAN_POINT('Ctrl Pts',(215.469815568742,5.69479574451283,-11.043823074723));
#36107=CARTESIAN_POINT('Ctrl Pts',(215.588288720401,10.2662300644991,-7.00008906659626));
#36108=CARTESIAN_POINT('Ctrl Pts',(215.706761872059,12.360830913657,-1.2675116573381));
#36109=CARTESIAN_POINT('Ctrl Pts',(215.825235023717,11.473254318724,4.77086596074414));
#36110=CARTESIAN_POINT('Ctrl Pts',(215.943708175376,7.81763725154309,9.65822315339587));
#36111=CARTESIAN_POINT('Ctrl Pts',(216.062181327034,2.27593488471799,12.2154347887429));
#36112=CARTESIAN_POINT('Ctrl Pts',(216.180654478692,-3.8148601543422,11.8255472888285));
#36113=CARTESIAN_POINT('Ctrl Pts',(216.299127630351,-8.98528099007356,8.58262501842705));
#36114=CARTESIAN_POINT('Ctrl Pts',(216.417600782009,-11.9879104787191,3.2690562906936));
#36115=CARTESIAN_POINT('Ctrl Pts',(216.536073933667,-12.0983334093154,-2.83320585107222));
#36116=CARTESIAN_POINT('Ctrl Pts',(216.654547085326,-9.28990911545137,-8.25192797497408));
#36117=CARTESIAN_POINT('Ctrl Pts',(216.773020236984,-4.24019880972685,-11.6797877006176));
#36118=CARTESIAN_POINT('Ctrl Pts',(216.891493388642,1.83250301955755,-12.2897786538578));
#36119=CARTESIAN_POINT('Ctrl Pts',(217.009966540301,7.46309466957279,-9.93473425062294));
#36120=CARTESIAN_POINT('Ctrl Pts',(217.128439691959,11.2931380601564,-5.18283314720375));
#36121=CARTESIAN_POINT('Ctrl Pts',(217.246912843617,12.3985958762547,0.819479697630158));
#36122=CARTESIAN_POINT('Ctrl Pts',(217.365385995275,10.5127650630656,6.62408464667336));
#36123=CARTESIAN_POINT('Ctrl Pts',(217.483859146934,6.09062167792295,10.8305611236871));
#36124=CARTESIAN_POINT('Ctrl Pts',(217.602332298592,0.199053242371885,12.4240534643169));
#36125=CARTESIAN_POINT('Ctrl Pts',(217.720805450251,-5.74053883282964,11.0201152710073));
#36126=CARTESIAN_POINT('Ctrl Pts',(217.839278601909,-10.2951669404969,6.95746105593078));
#36127=CARTESIAN_POINT('Ctrl Pts',(217.957751753567,-12.3659802587261,1.21624788522728));
#36128=CARTESIAN_POINT('Ctrl Pts',(218.076224905225,-11.4533738004635,-4.81839758263655));
#36129=CARTESIAN_POINT('Ctrl Pts',(218.194698056884,-7.77752324922622,-9.69055513297366));
#36130=CARTESIAN_POINT('Ctrl Pts',(218.313171208542,-2.2252653134951,-12.2247667037974));
#36131=CARTESIAN_POINT('Ctrl Pts',(218.4316443602,3.86386073984913,-11.8096277189421));
#36132=CARTESIAN_POINT('Ctrl Pts',(218.550117511859,9.02079069526072,-8.54529472346733));
#36133=CARTESIAN_POINT('Ctrl Pts',(218.668590663517,12.0013622223129,-3.2193215876436));
#36134=CARTESIAN_POINT('Ctrl Pts',(218.787063815175,12.086481820182,2.88334595378683));
#36135=CARTESIAN_POINT('Ctrl Pts',(218.905536966834,9.25561351080288,8.29037666325784));
#36136=CARTESIAN_POINT('Ctrl Pts',(219.024010118492,4.19173335739202,11.6972688317836));
#36137=CARTESIAN_POINT('Ctrl Pts',(219.14248327015,-1.88344553314147,12.2820747288597));
#36138=CARTESIAN_POINT('Ctrl Pts',(219.260956421808,-7.50422383581897,9.90370391333251));
#36139=CARTESIAN_POINT('Ctrl Pts',(219.379429573467,-11.3145310531959,5.13596280027263));
#36140=CARTESIAN_POINT('Ctrl Pts',(219.497902725125,-12.3950913999872,-0.870882132825059));
#36141=CARTESIAN_POINT('Ctrl Pts',(219.616375876784,-10.4852086433947,-6.66761773911089));
#36142=CARTESIAN_POINT('Ctrl Pts',(219.734849028442,-6.04566151106375,-10.8557222043472));
#36143=CARTESIAN_POINT('Ctrl Pts',(219.8533221801,-0.147536583240307,-12.4247718782891));
#36144=CARTESIAN_POINT('Ctrl Pts',(219.971795331759,5.78618338014802,-10.9962182904565));
#36145=CARTESIAN_POINT('Ctrl Pts',(220.090268483417,10.3239264932221,-6.91471282583509));
#36146=CARTESIAN_POINT('Ctrl Pts',(220.208741635075,12.3709176724325,-1.16496446066495));
#36147=CARTESIAN_POINT('Ctrl Pts',(220.327214786733,11.4332949628521,4.86584899186587));
#36148=CARTESIAN_POINT('Ctrl Pts',(220.445687938392,7.73727846682914,9.72271501496135));
#36149=CARTESIAN_POINT('Ctrl Pts',(220.56416109005,2.17455134987996,12.2338999155263));
#36150=CARTESIAN_POINT('Ctrl Pts',(220.682634241708,-3.91278207789302,11.7934811477489));
#36151=CARTESIAN_POINT('Ctrl Pts',(220.801107393367,-9.05617206812273,8.50786764724348));
#36152=CARTESIAN_POINT('Ctrl Pts',(220.919580545025,-12.0145515263405,3.16942747355545));
#36153=CARTESIAN_POINT('Ctrl Pts',(221.038053696683,-12.0745376864656,-2.9332109864585));
#36154=CARTESIAN_POINT('Ctrl Pts',(221.156526848342,-9.22089667210347,-8.32909359747953));
#36155=CARTESIAN_POINT('Ctrl Pts',(221.235508949447,-5.83600017639687,-10.5848002797816));
#36156=CARTESIAN_POINT('Ctrl Pts',(221.275,-3.97626028075542,-11.2425521648639));
#36157=CARTESIAN_POINT('Ctrl Pts',(203.669351500835,6.75676218362565,-9.47651510928075));
#36158=CARTESIAN_POINT('Ctrl Pts',(203.708842551388,8.32436471389968,-8.35881336202787));
#36159=CARTESIAN_POINT('Ctrl Pts',(203.787824652493,10.8925830183565,-5.33145141082714));
#36160=CARTESIAN_POINT('Ctrl Pts',(203.906297804152,12.117072160173,0.498777195873124));
#36161=CARTESIAN_POINT('Ctrl Pts',(204.02477095581,10.4179498404076,6.20767540737902));
#36162=CARTESIAN_POINT('Ctrl Pts',(204.143244107468,6.20549241904135,10.4194032208181));
#36163=CARTESIAN_POINT('Ctrl Pts',(204.261717259127,0.495845594717724,12.1171089200209));
#36164=CARTESIAN_POINT('Ctrl Pts',(204.380190410785,-5.33340499775821,10.89154986571));
#36165=CARTESIAN_POINT('Ctrl Pts',(204.498663562443,-9.87592838189151,7.0382388085738));
#36166=CARTESIAN_POINT('Ctrl Pts',(204.617136714102,-12.0357770641469,1.48690604185916));
#36167=CARTESIAN_POINT('Ctrl Pts',(204.73560986576,-11.2918735259622,-4.42317038811887));
#36168=CARTESIAN_POINT('Ctrl Pts',(204.854083017418,-7.82368823005323,-9.26610563157517));
#36169=CARTESIAN_POINT('Ctrl Pts',(204.972556169076,-2.46795837931619,-11.873500517429));
#36170=CARTESIAN_POINT('Ctrl Pts',(205.091029320735,3.48319207428195,-11.6162900743298));
#36171=CARTESIAN_POINT('Ctrl Pts',(205.209502472393,8.59398651744738,-8.5565309594037));
#36172=CARTESIAN_POINT('Ctrl Pts',(205.327975624052,11.6313934913279,-3.43242053779264));
#36173=CARTESIAN_POINT('Ctrl Pts',(205.44644877571,11.8626072611781,2.51979645276714));
#36174=CARTESIAN_POINT('Ctrl Pts',(205.564921927368,9.23184517669876,7.86408673337551));
#36175=CARTESIAN_POINT('Ctrl Pts',(205.683395079026,4.37380559480734,11.3110852657559));
#36176=CARTESIAN_POINT('Ctrl Pts',(205.801868230685,-1.53945951663779,12.0291682921515));
#36177=CARTESIAN_POINT('Ctrl Pts',(205.920341382343,-7.08131420607698,9.84509088138708));
#36178=CARTESIAN_POINT('Ctrl Pts',(206.038814534001,-10.9147290942386,5.28578415791509));
#36179=CARTESIAN_POINT('Ctrl Pts',(206.15728768566,-12.1148534588228,-0.548772297728888));
#36180=CARTESIAN_POINT('Ctrl Pts',(206.275760837318,-10.3921449671051,-6.2509317980072));
#36181=CARTESIAN_POINT('Ctrl Pts',(206.394233988976,-6.16222474083492,-10.4449897849049));
#36182=CARTESIAN_POINT('Ctrl Pts',(206.512707140635,-0.44560448958899,-12.119086681784));
#36183=CARTESIAN_POINT('Ctrl Pts',(206.631180292293,5.37852242256608,-10.8693294141092));
#36184=CARTESIAN_POINT('Ctrl Pts',(206.749653443951,9.90502554526596,-6.99723476166445));
#36185=CARTESIAN_POINT('Ctrl Pts',(206.868126595609,12.0418394981499,-1.43698533849758));
#36186=CARTESIAN_POINT('Ctrl Pts',(206.986599747268,11.2734359630216,4.4699515601325));
#36187=CARTESIAN_POINT('Ctrl Pts',(207.105072898926,7.78520018674576,9.29846672385004));
#36188=CARTESIAN_POINT('Ctrl Pts',(207.223546050585,2.41870488594333,11.8836312647686));
#36189=CARTESIAN_POINT('Ctrl Pts',(207.342019202243,-3.53132781660499,11.601747679291));
#36190=CARTESIAN_POINT('Ctrl Pts',(207.460492353901,-8.62939140510808,8.52082327828202));
#36191=CARTESIAN_POINT('Ctrl Pts',(207.578965505559,-11.6455256650487,3.38416272465686));
#36192=CARTESIAN_POINT('Ctrl Pts',(207.697438657218,-11.8520572206502,-2.56896185271385));
#36193=CARTESIAN_POINT('Ctrl Pts',(207.815911808876,-9.19915821236894,-7.902297991475));
#36194=CARTESIAN_POINT('Ctrl Pts',(207.934384960534,-4.32686777990447,-11.3291235573406));
#36195=CARTESIAN_POINT('Ctrl Pts',(208.052858112193,1.5893239555491,-12.0226816778364));
#36196=CARTESIAN_POINT('Ctrl Pts',(208.171331263851,7.12207495917007,-9.81564433128193));
#36197=CARTESIAN_POINT('Ctrl Pts',(208.28980441551,10.9365522118821,-5.24048195102726));
#36198=CARTESIAN_POINT('Ctrl Pts',(208.408277567168,12.1124738893081,0.599000536806266));
#36199=CARTESIAN_POINT('Ctrl Pts',(208.526750718826,10.3661368062066,6.29396799144016));
#36200=CARTESIAN_POINT('Ctrl Pts',(208.645223870484,6.11886272447068,10.4704510084976));
#36201=CARTESIAN_POINT('Ctrl Pts',(208.763697022143,0.395350149718566,12.1208301539697));
#36202=CARTESIAN_POINT('Ctrl Pts',(208.882170173801,-5.42354471019256,10.8469345042186));
#36203=CARTESIAN_POINT('Ctrl Pts',(209.000643325459,-9.93395369122276,6.95610447182229));
#36204=CARTESIAN_POINT('Ctrl Pts',(209.119116477118,-12.0476942900429,1.38704277364959));
#36205=CARTESIAN_POINT('Ctrl Pts',(209.237589628776,-11.2548048721566,-4.51665724313303));
#36206=CARTESIAN_POINT('Ctrl Pts',(209.356062780434,-7.7465781551971,-9.33066729916396));
#36207=CARTESIAN_POINT('Ctrl Pts',(209.474535932092,-2.36940987559633,-11.8935580127938));
#36208=CARTESIAN_POINT('Ctrl Pts',(209.593009083751,3.57940287808283,-11.5870056700874));
#36209=CARTESIAN_POINT('Ctrl Pts',(209.711482235409,8.66464791524722,-8.48496917301807));
#36210=CARTESIAN_POINT('Ctrl Pts',(209.829955387067,11.6594576285783,-3.33584669456673));
#36211=CARTESIAN_POINT('Ctrl Pts',(209.948428538726,11.8413034082419,2.61808306900733));
#36212=CARTESIAN_POINT('Ctrl Pts',(210.066901690384,9.16631309174318,7.9403733959054));
#36213=CARTESIAN_POINT('Ctrl Pts',(210.185374842042,4.27985557383898,11.3469670674301));
#36214=CARTESIAN_POINT('Ctrl Pts',(210.303847993701,-1.63916106937189,12.0159883634648));
#36215=CARTESIAN_POINT('Ctrl Pts',(210.422321145359,-7.16271326505017,9.78602902330351));
#36216=CARTESIAN_POINT('Ctrl Pts',(210.540794297018,-10.9581873010376,5.19508964673795));
#36217=CARTESIAN_POINT('Ctrl Pts',(210.659267448676,-12.1098860742171,-0.649218477669228));
#36218=CARTESIAN_POINT('Ctrl Pts',(210.777740600334,-10.3399504238451,-6.33689597474106));
#36219=CARTESIAN_POINT('Ctrl Pts',(210.896213751992,-6.07539550860324,-10.4957322172542));
#36220=CARTESIAN_POINT('Ctrl Pts',(211.014686903651,-0.345089012723726,
-12.1223652368489));
#36221=CARTESIAN_POINT('Ctrl Pts',(211.133160055309,5.46847375266852,-10.8243531067053));
#36222=CARTESIAN_POINT('Ctrl Pts',(211.251633206967,9.96271104611431,-6.9148545880515));
#36223=CARTESIAN_POINT('Ctrl Pts',(211.370106358626,12.0533419500502,-1.33707636185219));
#36224=CARTESIAN_POINT('Ctrl Pts',(211.488579510284,11.235980281283,4.56328527279234));
#36225=CARTESIAN_POINT('Ctrl Pts',(211.607052661942,7.70782293938106,9.3627074555075));
#36226=CARTESIAN_POINT('Ctrl Pts',(211.7255258136,2.32007412879624,11.9032802789464));
#36227=CARTESIAN_POINT('Ctrl Pts',(211.843998965259,-3.62741640011194,11.5720644494603));
#36228=CARTESIAN_POINT('Ctrl Pts',(211.962472116917,-8.69975545705987,8.44896918858282));
#36229=CARTESIAN_POINT('Ctrl Pts',(212.080945268576,-11.6731891350429,3.2874733124059));
#36230=CARTESIAN_POINT('Ctrl Pts',(212.199418420234,-11.8303460123564,-2.66715927349457));
#36231=CARTESIAN_POINT('Ctrl Pts',(212.317891571892,-9.1333103778332,-7.97831228421332));
#36232=CARTESIAN_POINT('Ctrl Pts',(212.43636472355,-4.23276978568116,-11.364615492998));
#36233=CARTESIAN_POINT('Ctrl Pts',(212.554837875209,1.68897000165938,-12.0090884623172));
#36234=CARTESIAN_POINT('Ctrl Pts',(212.673311026867,7.20322842485229,-9.75624546747695));
#36235=CARTESIAN_POINT('Ctrl Pts',(212.791784178525,10.9796339898288,-5.1496080250501));
#36236=CARTESIAN_POINT('Ctrl Pts',(212.910257330184,12.107090057999,0.699425256741116));
#36237=CARTESIAN_POINT('Ctrl Pts',(213.028730481842,10.3135862702544,6.37971500995803));
#36238=CARTESIAN_POINT('Ctrl Pts',(213.1472036335,6.03182384053987,10.5208329764786));
#36239=CARTESIAN_POINT('Ctrl Pts',(213.265676785159,0.294821942731522,12.1236919040509));
#36240=CARTESIAN_POINT('Ctrl Pts',(213.384149936817,-5.51330877754666,10.8015856097932));
#36241=CARTESIAN_POINT('Ctrl Pts',(213.502623088475,-9.99129711552418,6.87348581955205));
#36242=CARTESIAN_POINT('Ctrl Pts',(213.621096240133,-12.0587823810742,1.2870869621585));
#36243=CARTESIAN_POINT('Ctrl Pts',(213.739569391792,-11.2169625140456,-4.60983484744952));
#36244=CARTESIAN_POINT('Ctrl Pts',(213.85804254345,-7.66893520560297,-9.39458664202572));
#36245=CARTESIAN_POINT('Ctrl Pts',(213.976515695109,-2.27069849375563,-11.9127978960747));
#36246=CARTESIAN_POINT('Ctrl Pts',(214.094988846767,3.67536755721219,-11.5569242742893));
#36247=CARTESIAN_POINT('Ctrl Pts',(214.213461998425,8.73471342695404,-8.41282394391167));
#36248=CARTESIAN_POINT('Ctrl Pts',(214.331935150083,11.6867199483614,-3.23904340984146));
#36249=CARTESIAN_POINT('Ctrl Pts',(214.450408301742,11.8191852213803,2.71618962242513));
#36250=CARTESIAN_POINT('Ctrl Pts',(214.5688814534,9.10015063804339,8.01611400412836));
#36251=CARTESIAN_POINT('Ctrl Pts',(214.687354605058,4.18561122496097,11.3820685306207));
#36252=CARTESIAN_POINT('Ctrl Pts',(214.805827756717,-1.73874989606355,12.0019820930213));
#36253=CARTESIAN_POINT('Ctrl Pts',(214.924300908375,-7.24361974201309,9.72629417586076));
#36254=CARTESIAN_POINT('Ctrl Pts',(215.042774060033,-11.0008919095302,5.10403786791374));
#36255=CARTESIAN_POINT('Ctrl Pts',(215.161247211692,-12.1040858887246,-0.749620010833857));
#36256=CARTESIAN_POINT('Ctrl Pts',(215.27972036335,-10.2870447987044,-6.42242436091798));
#36257=CARTESIAN_POINT('Ctrl Pts',(215.398193515008,-5.98814846939336,-10.5457528546219));
#36258=CARTESIAN_POINT('Ctrl Pts',(215.516666666667,-0.244549803966582,
-12.1248101327668));
#36259=CARTESIAN_POINT('Ctrl Pts',(215.635139818325,5.55804901399366,-10.7786324049162));
#36260=CARTESIAN_POINT('Ctrl Pts',(215.753612969983,10.0197114079818,-6.83199887756314));
#36261=CARTESIAN_POINT('Ctrl Pts',(215.872086121641,12.0640154895794,-1.23707543401911));
#36262=CARTESIAN_POINT('Ctrl Pts',(215.9905592733,11.1977518974102,4.6563051667937));
#36263=CARTESIAN_POINT('Ctrl Pts',(216.109032424958,7.62991562244628,9.42630431063069));
#36264=CARTESIAN_POINT('Ctrl Pts',(216.227505576616,2.22128381937299,11.9221107005453));
#36265=CARTESIAN_POINT('Ctrl Pts',(216.345978728275,-3.72325552497568,11.5415854048741));
#36266=CARTESIAN_POINT('Ctrl Pts',(216.464451879933,-8.76952122390942,8.37653406043739));
#36267=CARTESIAN_POINT('Ctrl Pts',(216.582925031591,-11.7000498359031,3.19055781951202));
#36268=CARTESIAN_POINT('Ctrl Pts',(216.70139818325,-11.8078212271973,-2.76517327283705));
#36269=CARTESIAN_POINT('Ctrl Pts',(216.819871334908,-9.06683444247781,-8.05377790573855));
#36270=CARTESIAN_POINT('Ctrl Pts',(216.938344486566,-4.13838070245931,-11.3993258802342));
#36271=CARTESIAN_POINT('Ctrl Pts',(217.056817638225,1.78849989673574,-11.9946693777545));
#36272=CARTESIAN_POINT('Ctrl Pts',(217.175290789883,7.2838865220984,-9.69617566339728));
#36273=CARTESIAN_POINT('Ctrl Pts',(217.293763941541,11.0219606946616,-5.05837995880107));
#36274=CARTESIAN_POINT('Ctrl Pts',(217.4122370932,12.1008736180437,0.799801876966326));
#36275=CARTESIAN_POINT('Ctrl Pts',(217.530710244858,10.2603264655135,6.46502329333376));
#36276=CARTESIAN_POINT('Ctrl Pts',(217.649183396516,5.94437014605935,10.5704914232454));
#36277=CARTESIAN_POINT('Ctrl Pts',(217.767656548175,0.19427346074058,12.1257199037712));
#36278=CARTESIAN_POINT('Ctrl Pts',(217.886129699833,-5.60269369280611,10.755493886701));
#36279=CARTESIAN_POINT('Ctrl Pts',(218.004602851491,-10.0479534349698,6.79039447535502));
#36280=CARTESIAN_POINT('Ctrl Pts',(218.12307600315,-12.0690411855952,1.18704263726627));
#36281=CARTESIAN_POINT('Ctrl Pts',(218.241549154808,-11.1783487616574,-4.70269543187866));
#36282=CARTESIAN_POINT('Ctrl Pts',(218.360022306466,-7.59076486076366,-9.45785991600705));
#36283=CARTESIAN_POINT('Ctrl Pts',(218.478495458124,-2.17183095521254,-11.9312185322559));
#36284=CARTESIAN_POINT('Ctrl Pts',(218.596968609783,3.77107948007088,-11.5260481049111));
#36285=CARTESIAN_POINT('Ctrl Pts',(218.715441761441,8.80417824950912,-8.34010016212016));
#36286=CARTESIAN_POINT('Ctrl Pts',(218.833914913099,11.7131785684463,-3.14201737492898));
#36287=CARTESIAN_POINT('Ctrl Pts',(218.952388064758,11.7962542252798,2.8141093823934));
#36288=CARTESIAN_POINT('Ctrl Pts',(219.070861216416,9.03336236373215,8.0913033418722));
#36289=CARTESIAN_POINT('Ctrl Pts',(219.189334368074,4.09107903060885,11.4163872443638));
#36290=CARTESIAN_POINT('Ctrl Pts',(219.307807519733,-1.8382191492073,11.987150443861));
#36291=CARTESIAN_POINT('Ctrl Pts',(219.426280671391,-7.32402807100668,9.66589044452053));
#36292=CARTESIAN_POINT('Ctrl Pts',(219.544753823049,-11.0428399867738,5.01263508976042));
#36293=CARTESIAN_POINT('Ctrl Pts',(219.663226974708,-12.0974532932881,-0.849970007145037));
#36294=CARTESIAN_POINT('Ctrl Pts',(219.781700126366,-10.2334317465363,-6.50751104396671));
#36295=CARTESIAN_POINT('Ctrl Pts',(219.900173278024,-5.90048958874147,-10.5950483214781));
#36296=CARTESIAN_POINT('Ctrl Pts',(220.018646429683,-0.143993849436442,
-12.1264210667714));
#36297=CARTESIAN_POINT('Ctrl Pts',(220.137119581341,5.64724219684359,-10.7321707342743));
#36298=CARTESIAN_POINT('Ctrl Pts',(220.255592732999,10.0760223966742,-6.74867274049521));
#36299=CARTESIAN_POINT('Ctrl Pts',(220.374065884658,12.0738600392668,-1.13699065996796));
#36300=CARTESIAN_POINT('Ctrl Pts',(220.492539036316,11.1587520687127,4.74900741041341));
#36301=CARTESIAN_POINT('Ctrl Pts',(220.611012187974,7.55148645936778,9.48924755630021));
#36302=CARTESIAN_POINT('Ctrl Pts',(220.729485339633,2.12233476463566,11.9401324320201));
#36303=CARTESIAN_POINT('Ctrl Pts',(220.847958491291,-3.81882609063897,11.5102892545281));
#36304=CARTESIAN_POINT('Ctrl Pts',(220.966431642949,-8.83871002437373,8.30357180650651));
#36305=CARTESIAN_POINT('Ctrl Pts',(221.084904794608,-11.7260511632741,3.09332134717786));
#36306=CARTESIAN_POINT('Ctrl Pts',(221.203377946266,-11.7845969010132,-2.86277702704783));
#36307=CARTESIAN_POINT('Ctrl Pts',(221.321851097924,-8.99947916585132,-8.12909058266712));
#36308=CARTESIAN_POINT('Ctrl Pts',(221.40083319903,-5.69586276335608,-10.330631930925));
#36309=CARTESIAN_POINT('Ctrl Pts',(221.440324249582,-3.88078001816469,-10.9725894971567));
#36310=CARTESIAN_POINT('Ctrl Pts',(203.834675750418,6.59052307073188,-9.24336091171122));
#36311=CARTESIAN_POINT('Ctrl Pts',(203.87416680097,8.11955729759066,-8.15315839291918));
#36312=CARTESIAN_POINT('Ctrl Pts',(203.953148902076,10.6245887795654,-5.20027974474125));
#36313=CARTESIAN_POINT('Ctrl Pts',(204.071622053734,11.8189513632536,0.486505596500501));
#36314=CARTESIAN_POINT('Ctrl Pts',(204.190095205392,10.1616331768082,6.05494567902541));
#36315=CARTESIAN_POINT('Ctrl Pts',(204.308568357051,6.05281639955519,10.1630507991643));
#36316=CARTESIAN_POINT('Ctrl Pts',(204.427041508709,0.483646122609916,11.8189872186854));
#36317=CARTESIAN_POINT('Ctrl Pts',(204.545514660367,-5.20218526685233,10.6235810459546));
#36318=CARTESIAN_POINT('Ctrl Pts',(204.663987812026,-9.63294727221344,6.86507442242633));
#36319=CARTESIAN_POINT('Ctrl Pts',(204.782460963684,-11.7396564004687,1.45032314392112));
#36320=CARTESIAN_POINT('Ctrl Pts',(204.900934115342,-11.0140553954953,-4.31434549514265));
#36321=CARTESIAN_POINT('Ctrl Pts',(205.019407267001,-7.63119914199956,-9.03812821601569));
#36322=CARTESIAN_POINT('Ctrl Pts',(205.137880418659,-2.40723828876296,-11.5813724035012));
#36323=CARTESIAN_POINT('Ctrl Pts',(205.256353570317,3.39749381456364,-11.3304902038307));
#36324=CARTESIAN_POINT('Ctrl Pts',(205.374826721976,8.3825454964294,-8.34601147129938));
#36325=CARTESIAN_POINT('Ctrl Pts',(205.493299873634,11.3452220258881,-3.34797142891857));
#36326=CARTESIAN_POINT('Ctrl Pts',(205.611773025292,11.5707471580529,2.4578009709673));
#36327=CARTESIAN_POINT('Ctrl Pts',(205.730246176951,9.00471068375088,7.67060370603969));
#36328=CARTESIAN_POINT('Ctrl Pts',(205.848719328609,4.26619524205395,11.0327944617666));
#36329=CARTESIAN_POINT('Ctrl Pts',(205.967192480267,-1.50158362617033,11.733210226529));
#36330=CARTESIAN_POINT('Ctrl Pts',(206.085665631925,-6.9070900200322,9.60286847811134));
#36331=CARTESIAN_POINT('Ctrl Pts',(206.204138783584,-10.6461899873718,5.15573606010141));
#36332=CARTESIAN_POINT('Ctrl Pts',(206.322611935242,-11.8167872494313,-0.535270650419746));
#36333=CARTESIAN_POINT('Ctrl Pts',(206.441085086901,-10.1364631903243,-6.09713781671562));
#36334=CARTESIAN_POINT('Ctrl Pts',(206.559558238559,-6.01061325199916,-10.1880078475748));
#36335=CARTESIAN_POINT('Ctrl Pts',(206.678031390217,-0.43464111792699,-11.8209163208462));
#36336=CARTESIAN_POINT('Ctrl Pts',(206.796504541875,5.24619265101169,-10.6019072923227));
#36337=CARTESIAN_POINT('Ctrl Pts',(206.914977693534,9.66132854734208,-6.82507921321143));
#36338=CARTESIAN_POINT('Ctrl Pts',(207.033450845192,11.7455696781712,-1.40163065804246));
#36339=CARTESIAN_POINT('Ctrl Pts',(207.15192399685,10.9960714587182,4.35997569272144));
#36340=CARTESIAN_POINT('Ctrl Pts',(207.270397148509,7.59365803422165,9.06969311639776));
#36341=CARTESIAN_POINT('Ctrl Pts',(207.388870300167,2.3591965972595,11.5912539003263));
#36342=CARTESIAN_POINT('Ctrl Pts',(207.507343451825,-3.44444525545874,11.3163056007024));
#36343=CARTESIAN_POINT('Ctrl Pts',(207.625816603484,-8.41707930457644,8.31118231943059));
#36344=CARTESIAN_POINT('Ctrl Pts',(207.744289755142,-11.3590065005247,3.30090092056398));
#36345=CARTESIAN_POINT('Ctrl Pts',(207.8627629068,-11.5604566840645,-2.50575673643968));
#36346=CARTESIAN_POINT('Ctrl Pts',(207.981236058459,-8.97282792886425,-7.70787483845822));
#36347=CARTESIAN_POINT('Ctrl Pts',(208.099709210117,-4.22041225552873,-11.0503889506083));
#36348=CARTESIAN_POINT('Ctrl Pts',(208.218182361775,1.55022123189376,-11.7268832047791));
#36349=CARTESIAN_POINT('Ctrl Pts',(208.336655513433,6.94684792127837,-9.57414641234265));
#36350=CARTESIAN_POINT('Ctrl Pts',(208.455128665092,10.6674761828003,-5.11154844012378));
#36351=CARTESIAN_POINT('Ctrl Pts',(208.57360181675,11.8144662253433,0.584263105599529));
#36352=CARTESIAN_POINT('Ctrl Pts',(208.692074968409,10.111094917804,6.13911517480345));
#36353=CARTESIAN_POINT('Ctrl Pts',(208.810548120067,5.96831808732183,10.2128426392895));
#36354=CARTESIAN_POINT('Ctrl Pts',(208.929021271725,0.385623204121608,11.8226168977425));
#36355=CARTESIAN_POINT('Ctrl Pts',(209.047494423383,-5.29010723868483,10.5800633726627));
#36356=CARTESIAN_POINT('Ctrl Pts',(209.165967575042,-9.68954496345093,6.78496086706518));
#36357=CARTESIAN_POINT('Ctrl Pts',(209.2844407267,-11.7512804224591,1.3529168485436));
#36358=CARTESIAN_POINT('Ctrl Pts',(209.402913878358,-10.9778987554555,-4.40553225857115));
#36359=CARTESIAN_POINT('Ctrl Pts',(209.521387030017,-7.55598623476468,-9.10110144907693));
#36360=CARTESIAN_POINT('Ctrl Pts',(209.639860181675,-2.31111441023934,-11.6009364169073));
#36361=CARTESIAN_POINT('Ctrl Pts',(209.758333333333,3.49133750846188,-11.3019262945903));
#36362=CARTESIAN_POINT('Ctrl Pts',(209.876806484992,8.45146838578882,-8.27621034594672));
#36363=CARTESIAN_POINT('Ctrl Pts',(209.99527963665,11.3725956908155,-3.25377362758823));
#36364=CARTESIAN_POINT('Ctrl Pts',(210.113752788308,11.5499674516705,2.55366940532554));
#36365=CARTESIAN_POINT('Ctrl Pts',(210.232225939967,8.94079090885937,7.74501345966559));
#36366=CARTESIAN_POINT('Ctrl Pts',(210.350699091625,4.17455670811409,11.0677934502358));
#36367=CARTESIAN_POINT('Ctrl Pts',(210.469172243283,-1.59883218481789,11.7203545684904));
#36368=CARTESIAN_POINT('Ctrl Pts',(210.587645394941,-6.98648638792551,9.54525974071292));
#36369=CARTESIAN_POINT('Ctrl Pts',(210.7061185466,-10.6885789758751,5.06727293944427));
#36370=CARTESIAN_POINT('Ctrl Pts',(210.824591698258,-11.8119420792218,-0.633245515935656));
#36371=CARTESIAN_POINT('Ctrl Pts',(210.943064849916,-10.0855528086691,-6.18098698509304));
#36372=CARTESIAN_POINT('Ctrl Pts',(211.061538001575,-5.92592031140351,-10.2375018451397));
#36373=CARTESIAN_POINT('Ctrl Pts',(211.180011153233,-0.336598660423963,
-11.8241142124112));
#36374=CARTESIAN_POINT('Ctrl Pts',(211.298484304891,5.33393087535229,-10.5580375536038));
#36375=CARTESIAN_POINT('Ctrl Pts',(211.41695745655,9.71759479053014,-6.74472586940382));
#36376=CARTESIAN_POINT('Ctrl Pts',(211.535430608208,11.7567891310036,-1.30417977881064));
#36377=CARTESIAN_POINT('Ctrl Pts',(211.653903759866,10.9595373129366,4.45101308161348));
#36378=CARTESIAN_POINT('Ctrl Pts',(211.772376911525,7.518184527822,9.13235330963281));
#36379=CARTESIAN_POINT('Ctrl Pts',(211.890850063183,2.26299248902007,11.6104194825588));
#36380=CARTESIAN_POINT('Ctrl Pts',(212.009323214841,-3.53816973609404,11.2873526783268));
#36381=CARTESIAN_POINT('Ctrl Pts',(212.1277963665,-8.48571216379742,8.24109608241064));
#36382=CARTESIAN_POINT('Ctrl Pts',(212.246269518158,-11.3859893559603,3.20659039359594));
#36383=CARTESIAN_POINT('Ctrl Pts',(212.364742669816,-11.5392796446386,-2.60153816984724));
#36384=CARTESIAN_POINT('Ctrl Pts',(212.483215821474,-8.90860017289598,-7.78201892350702));
#36385=CARTESIAN_POINT('Ctrl Pts',(212.601688973133,-4.1286293889745,-11.0850076650781));
#36386=CARTESIAN_POINT('Ctrl Pts',(212.720162124791,1.64741564956743,-11.7136244281565));
#36387=CARTESIAN_POINT('Ctrl Pts',(212.838635276449,7.02600473830304,-9.51620896069891));
#36388=CARTESIAN_POINT('Ctrl Pts',(212.957108428108,10.7094980038693,-5.02291031887514));
#36389=CARTESIAN_POINT('Ctrl Pts',(213.075581579766,11.8092148544223,0.682217039098379));
#36390=CARTESIAN_POINT('Ctrl Pts',(213.194054731424,10.0598373020762,6.22275252778859));
#36391=CARTESIAN_POINT('Ctrl Pts',(213.312527883083,5.88342065316515,10.261985041124));
#36392=CARTESIAN_POINT('Ctrl Pts',(213.431001034741,0.287568329700688,11.8254082391305));
#36393=CARTESIAN_POINT('Ctrl Pts',(213.549474186399,-5.3776628075716,10.5358302138182));
#36394=CARTESIAN_POINT('Ctrl Pts',(213.667947338058,-9.74547754632755,6.70437491197867));
#36395=CARTESIAN_POINT('Ctrl Pts',(213.786420489716,-11.7620957090959,1.25542028676107));
#36396=CARTESIAN_POINT('Ctrl Pts',(213.904893641374,-10.9409874468431,-4.49641737991101));
#36397=CARTESIAN_POINT('Ctrl Pts',(214.023366793033,-7.48025356330558,-9.16344816076338));
#36398=CARTESIAN_POINT('Ctrl Pts',(214.141839944691,-2.21483166094538,-11.6197029342414));
#36399=CARTESIAN_POINT('Ctrl Pts',(214.260313096349,3.58494113318469,-11.2725850024714));
#36400=CARTESIAN_POINT('Ctrl Pts',(214.378786248008,8.51981004986064,-8.20584013252983));
#36401=CARTESIAN_POINT('Ctrl Pts',(214.497259399666,11.3991872656865,-3.15935202979238));
#36402=CARTESIAN_POINT('Ctrl Pts',(214.615732551324,11.5283934467207,2.64936220701343));
#36403=CARTESIAN_POINT('Ctrl Pts',(214.734205702982,8.87625627441841,7.81889059376015));
#36404=CARTESIAN_POINT('Ctrl Pts',(214.852678854641,4.08263108772274,11.1020312991769));
#36405=CARTESIAN_POINT('Ctrl Pts',(214.971152006299,-1.69597079086341,11.7066928994863));
#36406=CARTESIAN_POINT('Ctrl Pts',(215.089625157957,-7.06540229298547,9.48699457176081));
#36407=CARTESIAN_POINT('Ctrl Pts',(215.208098309616,-10.7302329071292,4.9784613411278));
#36408=CARTESIAN_POINT('Ctrl Pts',(215.326571461274,-11.8062845978329,-0.731176833136949));
#36409=CARTESIAN_POINT('Ctrl Pts',(215.445044612932,-10.0339488401432,-6.26441108482937));
#36410=CARTESIAN_POINT('Ctrl Pts',(215.563517764591,-5.84081984328888,-10.2862918063113));
#36411=CARTESIAN_POINT('Ctrl Pts',(215.681990916249,-0.238533054913557,
-11.8264989556528));
#36412=CARTESIAN_POINT('Ctrl Pts',(215.800464067907,5.42130228347449,-10.5134417351093));
#36413=CARTESIAN_POINT('Ctrl Pts',(215.918937219566,9.77319275146448,-6.66390868853002));
#36414=CARTESIAN_POINT('Ctrl Pts',(216.037410371224,11.7672000655017,-1.20663921070012));
#36415=CARTESIAN_POINT('Ctrl Pts',(216.155883522882,10.9222494760965,4.54174437284327));
#36416=CARTESIAN_POINT('Ctrl Pts',(216.274356674541,7.44219399334947,9.19438546786551));
#36417=CARTESIAN_POINT('Ctrl Pts',(216.392829826199,2.16663275402798,11.6287866123477));
#36418=CARTESIAN_POINT('Ctrl Pts',(216.511302977857,-3.63165089560916,11.2576235209197));
#36419=CARTESIAN_POINT('Ctrl Pts',(216.629776129516,-8.55376145774527,8.17044310244772));
#36420=CARTESIAN_POINT('Ctrl Pts',(216.748249281174,-11.412189193087,3.11205934833045));
#36421=CARTESIAN_POINT('Ctrl Pts',(216.866722432833,-11.5173090450793,-2.69714069460188));
#36422=CARTESIAN_POINT('Ctrl Pts',(216.98519558449,-8.84375976950426,-7.85562783650302));
#36423=CARTESIAN_POINT('Ctrl Pts',(217.103668736149,-4.03656259519177,-11.1188640598508));
#36424=CARTESIAN_POINT('Ctrl Pts',(217.222141887807,1.74449677391393,-11.6995601016511));
#36425=CARTESIAN_POINT('Ctrl Pts',(217.340615039466,7.10467837462401,-9.45761707617162));
#36426=CARTESIAN_POINT('Ctrl Pts',(217.459088191124,10.7507833291668,-4.93392677039839));
#36427=CARTESIAN_POINT('Ctrl Pts',(217.577561342782,11.8031513598328,0.780124056302488));
#36428=CARTESIAN_POINT('Ctrl Pts',(217.69603449444,10.0078878679614,6.30596193999415));
#36429=CARTESIAN_POINT('Ctrl Pts',(217.814507646099,5.79811861419576,10.3104217228036));
#36430=CARTESIAN_POINT('Ctrl Pts',(217.932980797757,0.189493679109268,11.8273863432255));
#36431=CARTESIAN_POINT('Ctrl Pts',(218.051453949416,-5.46484855278258,10.4908725023946));
#36432=CARTESIAN_POINT('Ctrl Pts',(218.169927101073,-9.80073992944261,6.62332789477926));
#36433=CARTESIAN_POINT('Ctrl Pts',(218.288400252732,-11.7721021124642,1.15783738930527));
#36434=CARTESIAN_POINT('Ctrl Pts',(218.40687340439,-10.9033237228513,-4.58699328112077));
#36435=CARTESIAN_POINT('Ctrl Pts',(218.525346556049,-7.4040064723011,-9.22516469904043));
#36436=CARTESIAN_POINT('Ctrl Pts',(218.643819707707,-2.11839659692998,-11.6376703607144));
#36437=CARTESIAN_POINT('Ctrl Pts',(218.762292859365,3.67829822029263,-11.2424684908802));
#36438=CARTESIAN_POINT('Ctrl Pts',(218.880766011023,8.58756580375752,-8.13490560077299));
#36439=CARTESIAN_POINT('Ctrl Pts',(218.999239162682,11.4249949145797,-3.06471316221435));
#36440=CARTESIAN_POINT('Ctrl Pts',(219.11771231434,11.5060266303775,2.74487281099996));
#36441=CARTESIAN_POINT('Ctrl Pts',(219.236185465999,8.81111121666141,7.89223002048656));
#36442=CARTESIAN_POINT('Ctrl Pts',(219.354658617657,3.99042470382567,11.135505656944));
#36443=CARTESIAN_POINT('Ctrl Pts',(219.473131769315,-1.79299276527314,11.6922261588623));
#36444=CARTESIAN_POINT('Ctrl Pts',(219.591604920974,-7.14383230619438,9.42807697570855));
#36445=CARTESIAN_POINT('Ctrl Pts',(219.710078072632,-10.7711489203518,4.8893073792482));
#36446=CARTESIAN_POINT('Ctrl Pts',(219.82855122429,-11.799815186589,-0.82905788146501));
#36447=CARTESIAN_POINT('Ctrl Pts',(219.947024375948,-9.98165484967794,-6.34740434882255));
#36448=CARTESIAN_POINT('Ctrl Pts',(220.065497527607,-5.75531766641918,-10.3343744386089));
#36449=CARTESIAN_POINT('Ctrl Pts',(220.183970679265,-0.140451115632587,
-11.8280702552538));
#36450=CARTESIAN_POINT('Ctrl Pts',(220.302443830923,5.50830101353917,-10.4681231780922));
#36451=CARTESIAN_POINT('Ctrl Pts',(220.420916982582,9.82811830012625,-6.58263265515534));
#36452=CARTESIAN_POINT('Ctrl Pts',(220.53939013424,11.7768024061011,-1.10901685927098));
#36453=CARTESIAN_POINT('Ctrl Pts',(220.657863285898,10.8842091745733,4.63216582896095));
#36454=CARTESIAN_POINT('Ctrl Pts',(220.776336437557,7.36569445190642,9.25578009763907));
#36455=CARTESIAN_POINT('Ctrl Pts',(220.894809589215,2.07011817939136,11.6463649485139));
#36456=CARTESIAN_POINT('Ctrl Pts',(221.013282740873,-3.72487010338492,11.2270973613073));
#36457=CARTESIAN_POINT('Ctrl Pts',(221.131755892532,-8.62124798062474,8.09927596576955));
#36458=CARTESIAN_POINT('Ctrl Pts',(221.25022904419,-11.4375508002076,3.01721522080027));
#36459=CARTESIAN_POINT('Ctrl Pts',(221.368702195848,-11.4946561155609,-2.79234306763717));
#36460=CARTESIAN_POINT('Ctrl Pts',(221.487175347506,-8.77806165959916,-7.92908756785469));
#36461=CARTESIAN_POINT('Ctrl Pts',(221.566157448612,-5.5557253503153,-10.0764635820684));
#36462=CARTESIAN_POINT('Ctrl Pts',(221.605648499165,-3.78529975557396,-10.7026268294495));
#36463=CARTESIAN_POINT('Ctrl Pts',(204.,6.42428395783811,-9.01020671414169));
#36464=CARTESIAN_POINT('Ctrl Pts',(204.039491050553,7.91474988128163,-7.9475034238105));
#36465=CARTESIAN_POINT('Ctrl Pts',(204.118473151658,10.3565945407743,-5.06910807865537));
#36466=CARTESIAN_POINT('Ctrl Pts',(204.236946303317,11.5208305663343,0.474233997127887));
#36467=CARTESIAN_POINT('Ctrl Pts',(204.355419454975,9.90531651320884,5.90221595067179));
#36468=CARTESIAN_POINT('Ctrl Pts',(204.473892606633,5.90014038006902,9.90669837751048));
#36469=CARTESIAN_POINT('Ctrl Pts',(204.592365758292,0.471446650502101,11.5208655173499));
#36470=CARTESIAN_POINT('Ctrl Pts',(204.71083890995,-5.07096553594642,10.3556122261992));
#36471=CARTESIAN_POINT('Ctrl Pts',(204.829312061608,-9.38996616253539,6.69191003627886));
#36472=CARTESIAN_POINT('Ctrl Pts',(204.947785213267,-11.4435357367905,1.41374024598308));
#36473=CARTESIAN_POINT('Ctrl Pts',(205.066258364925,-10.7362372650283,-4.20552060216643));
#36474=CARTESIAN_POINT('Ctrl Pts',(205.184731516583,-7.43871005394589,-8.8101508004562));
#36475=CARTESIAN_POINT('Ctrl Pts',(205.303204668241,-2.34651819820973,-11.2892442895734));
#36476=CARTESIAN_POINT('Ctrl Pts',(205.4216778199,3.31179555484533,-11.0446903333316));
#36477=CARTESIAN_POINT('Ctrl Pts',(205.540150971558,8.17110447541142,-8.13549198319505));
#36478=CARTESIAN_POINT('Ctrl Pts',(205.658624123217,11.0590505604482,-3.26352232004452));
#36479=CARTESIAN_POINT('Ctrl Pts',(205.777097274875,11.2788870549277,2.39580548916746));
#36480=CARTESIAN_POINT('Ctrl Pts',(205.895570426533,8.777576190803,7.47712067870388));
#36481=CARTESIAN_POINT('Ctrl Pts',(206.014043578191,4.15858488930056,10.7545036577774));
#36482=CARTESIAN_POINT('Ctrl Pts',(206.13251672985,-1.46370773570288,11.4372521609064));
#36483=CARTESIAN_POINT('Ctrl Pts',(206.250989881508,-6.73286583398743,9.36064607483558));
#36484=CARTESIAN_POINT('Ctrl Pts',(206.369463033166,-10.377650880505,5.02568796228774));
#36485=CARTESIAN_POINT('Ctrl Pts',(206.487936184825,-11.5187210400399,-0.521769003110613));
#36486=CARTESIAN_POINT('Ctrl Pts',(206.606409336483,-9.8807814135434,-5.94334383542404));
#36487=CARTESIAN_POINT('Ctrl Pts',(206.724882488141,-5.85900176316342,-9.93102591024465));
#36488=CARTESIAN_POINT('Ctrl Pts',(206.8433556398,-0.423677746264986,-11.5227459599084));
#36489=CARTESIAN_POINT('Ctrl Pts',(206.961828791458,5.11386287945728,-10.3344851705362));
#36490=CARTESIAN_POINT('Ctrl Pts',(207.080301943116,9.41763154941819,-6.65292366475841));
#36491=CARTESIAN_POINT('Ctrl Pts',(207.198775094774,11.4492998581925,-1.36627597758734));
#36492=CARTESIAN_POINT('Ctrl Pts',(207.317248246433,10.7187069544147,4.24999982531037));
#36493=CARTESIAN_POINT('Ctrl Pts',(207.435721398091,7.40211588169753,8.8409195089455));
#36494=CARTESIAN_POINT('Ctrl Pts',(207.554194549749,2.29968830857567,11.298876535884));
#36495=CARTESIAN_POINT('Ctrl Pts',(207.672667701408,-3.35756269431251,11.0308635221138));
#36496=CARTESIAN_POINT('Ctrl Pts',(207.791140853066,-8.20476720404479,8.10154136057916));
#36497=CARTESIAN_POINT('Ctrl Pts',(207.909614004724,-11.0724873360008,3.2176391164711));
#36498=CARTESIAN_POINT('Ctrl Pts',(208.028087156383,-11.2688561474788,-2.4425516201655));
#36499=CARTESIAN_POINT('Ctrl Pts',(208.146560308041,-8.74649764535955,-7.51345168544144));
#36500=CARTESIAN_POINT('Ctrl Pts',(208.265033459699,-4.11395673115298,-10.771654343876));
#36501=CARTESIAN_POINT('Ctrl Pts',(208.383506611358,1.51111850823841,-11.4310847317218));
#36502=CARTESIAN_POINT('Ctrl Pts',(208.501979763016,6.77162088338667,-9.33264849340337));
#36503=CARTESIAN_POINT('Ctrl Pts',(208.620452914674,10.3984001537186,-4.9826149292203));
#36504=CARTESIAN_POINT('Ctrl Pts',(208.738926066332,11.5164585613786,0.569525674392788));
#36505=CARTESIAN_POINT('Ctrl Pts',(208.857399217991,9.85605302940134,5.98426235816675));
#36506=CARTESIAN_POINT('Ctrl Pts',(208.975872369649,5.817773450173,9.95523427008149));
#36507=CARTESIAN_POINT('Ctrl Pts',(209.094345521308,0.375896258524645,11.5244036415153));
#36508=CARTESIAN_POINT('Ctrl Pts',(209.212818672966,-5.15666976717709,10.3131922411068));
#36509=CARTESIAN_POINT('Ctrl Pts',(209.331291824624,-9.44513623567911,6.61381726230806));
#36510=CARTESIAN_POINT('Ctrl Pts',(209.449764976282,-11.4548665548753,1.31879092343762));
#36511=CARTESIAN_POINT('Ctrl Pts',(209.568238127941,-10.7009926387546,-4.29440727400929));
#36512=CARTESIAN_POINT('Ctrl Pts',(209.686711279599,-7.36539431433226,-8.87153559898989));
#36513=CARTESIAN_POINT('Ctrl Pts',(209.805184431257,-2.25281894488235,-11.3083148210209));
#36514=CARTESIAN_POINT('Ctrl Pts',(209.923657582916,3.40327213884093,-11.0168469190931));
#36515=CARTESIAN_POINT('Ctrl Pts',(210.042130734574,8.23828885633043,-8.06745151887539));
#36516=CARTESIAN_POINT('Ctrl Pts',(210.160603886232,11.0857337530526,-3.17170056060973));
#36517=CARTESIAN_POINT('Ctrl Pts',(210.279077037891,11.2586314950991,2.48925574164375));
#36518=CARTESIAN_POINT('Ctrl Pts',(210.397550189549,8.71526872597554,7.54965352342579));
#36519=CARTESIAN_POINT('Ctrl Pts',(210.516023341207,4.0692578423892,10.7886198330415));
#36520=CARTESIAN_POINT('Ctrl Pts',(210.634496492866,-1.55850330026388,11.4247207735161));
#36521=CARTESIAN_POINT('Ctrl Pts',(210.752969644524,-6.81025951080084,9.30449045812232));
#36522=CARTESIAN_POINT('Ctrl Pts',(210.871442796182,-10.4189706507126,4.9394562321506));
#36523=CARTESIAN_POINT('Ctrl Pts',(210.989915947841,-11.5139980842265,-0.617272554202086));
#36524=CARTESIAN_POINT('Ctrl Pts',(211.108389099499,-9.83115519349314,-6.02507799544502));
#36525=CARTESIAN_POINT('Ctrl Pts',(211.226862251157,-5.77644511420377,-9.97927147302517));
#36526=CARTESIAN_POINT('Ctrl Pts',(211.345335402816,-0.328108308124205,
-11.5258631879735));
#36527=CARTESIAN_POINT('Ctrl Pts',(211.463808554474,5.19938799803607,-10.2917220005022));
#36528=CARTESIAN_POINT('Ctrl Pts',(211.582281706132,9.47247853494596,-6.57459715075616));
#36529=CARTESIAN_POINT('Ctrl Pts',(211.700754857791,11.460236311957,-1.27128319576909));
#36530=CARTESIAN_POINT('Ctrl Pts',(211.819228009449,10.6830943445901,4.33874089043461));
#36531=CARTESIAN_POINT('Ctrl Pts',(211.937701161107,7.32854611626294,8.90199916375812));
#36532=CARTESIAN_POINT('Ctrl Pts',(212.056174312765,2.2059108492439,11.3175586861713));
#36533=CARTESIAN_POINT('Ctrl Pts',(212.174647464424,-3.44892307207615,11.0026409071933));
#36534=CARTESIAN_POINT('Ctrl Pts',(212.293120616082,-8.27166887053497,8.03322297623846));
#36535=CARTESIAN_POINT('Ctrl Pts',(212.411593767741,-11.0987895768778,3.12570747478597));
#36536=CARTESIAN_POINT('Ctrl Pts',(212.530066919398,-11.2482132769208,-2.53591706619991));
#36537=CARTESIAN_POINT('Ctrl Pts',(212.648540071057,-8.68388996795875,-7.58572556280073));
#36538=CARTESIAN_POINT('Ctrl Pts',(212.767013222715,-4.02448899226784,-10.8053998371582));
#36539=CARTESIAN_POINT('Ctrl Pts',(212.885486374374,1.60586129747547,-11.4181603939958));
#36540=CARTESIAN_POINT('Ctrl Pts',(213.003959526032,6.84878105175381,-9.27617245392087));
#36541=CARTESIAN_POINT('Ctrl Pts',(213.12243267769,10.4393620179098,-4.89621261270018));
#36542=CARTESIAN_POINT('Ctrl Pts',(213.240905829349,11.5113396508456,0.665008821455645));
#36543=CARTESIAN_POINT('Ctrl Pts',(213.359378981007,9.806088333898,6.06579004561915));
#36544=CARTESIAN_POINT('Ctrl Pts',(213.477852132665,5.73501746579043,10.0031371057694));
#36545=CARTESIAN_POINT('Ctrl Pts',(213.596325284323,0.280314716669852,11.5271245742102));
#36546=CARTESIAN_POINT('Ctrl Pts',(213.714798435982,-5.24201683759653,10.2700748178432));
#36547=CARTESIAN_POINT('Ctrl Pts',(213.83327158764,-9.49965797713093,6.5352640044053));
#36548=CARTESIAN_POINT('Ctrl Pts',(213.951744739299,-11.4654090371176,1.22375361136365));
#36549=CARTESIAN_POINT('Ctrl Pts',(214.070217890957,-10.6650123796405,-4.38299991237251));
#36550=CARTESIAN_POINT('Ctrl Pts',(214.188691042615,-7.2915719210082,-8.93230967950104));
#36551=CARTESIAN_POINT('Ctrl Pts',(214.307164194274,-2.15896482813512,-11.3266079724081));
#36552=CARTESIAN_POINT('Ctrl Pts',(214.425637345932,3.4945147091572,-10.9882457306536));
#36553=CARTESIAN_POINT('Ctrl Pts',(214.54411049759,8.30490667276723,-7.99885632114799));
#36554=CARTESIAN_POINT('Ctrl Pts',(214.662583649248,11.1116545830117,-3.0796606497433));
#36555=CARTESIAN_POINT('Ctrl Pts',(214.781056800907,11.2376016720611,2.58253479160174));
#36556=CARTESIAN_POINT('Ctrl Pts',(214.899529952565,8.65236191079344,7.62166718339193));
#36557=CARTESIAN_POINT('Ctrl Pts',(215.018003104223,3.9796509504845,10.8219940677331));
#36558=CARTESIAN_POINT('Ctrl Pts',(215.136476255882,-1.65319168566326,11.4114037059512));
#36559=CARTESIAN_POINT('Ctrl Pts',(215.25494940754,-6.88718484395786,9.24769496766087));
#36560=CARTESIAN_POINT('Ctrl Pts',(215.373422559198,-10.4595739047283,4.85288481434185));
#36561=CARTESIAN_POINT('Ctrl Pts',(215.491895710856,-11.5084833069413,-0.712733655440043));
#36562=CARTESIAN_POINT('Ctrl Pts',(215.610368862515,-9.7808528815819,-6.10639780874076));
#36563=CARTESIAN_POINT('Ctrl Pts',(215.728842014173,-5.6934912171844,-10.0268307580006));
#36564=CARTESIAN_POINT('Ctrl Pts',(215.847315165831,-0.232516305860531,
-11.5281877785388));
#36565=CARTESIAN_POINT('Ctrl Pts',(215.96578831749,5.28455555295532,-10.2482510653024));
#36566=CARTESIAN_POINT('Ctrl Pts',(216.084261469148,9.52667409494713,-6.4958184994969));
#36567=CARTESIAN_POINT('Ctrl Pts',(216.202734620806,11.4703846414241,-1.17620298738114));
#36568=CARTESIAN_POINT('Ctrl Pts',(216.321207772465,10.6467470547827,4.42718357889284));
#36569=CARTESIAN_POINT('Ctrl Pts',(216.439680924123,7.25447236425265,8.96246662510033));
#36570=CARTESIAN_POINT('Ctrl Pts',(216.558154075782,2.11198168868298,11.3354625241501));
#36571=CARTESIAN_POINT('Ctrl Pts',(216.67662722744,-3.54004626624265,10.9736616369653));
#36572=CARTESIAN_POINT('Ctrl Pts',(216.795100379098,-8.33800169158112,7.96435214445806));
#36573=CARTESIAN_POINT('Ctrl Pts',(216.913573530756,-11.124328550271,3.03356087714887));
#36574=CARTESIAN_POINT('Ctrl Pts',(217.032046682415,-11.2267968629613,-2.62910811636671));
#36575=CARTESIAN_POINT('Ctrl Pts',(217.150519834073,-8.62068509653071,-7.65747776726749));
#36576=CARTESIAN_POINT('Ctrl Pts',(217.268992985731,-3.93474448792423,-10.8384022394674));
#36577=CARTESIAN_POINT('Ctrl Pts',(217.38746613739,1.70049365109212,-11.4044508255478));
#36578=CARTESIAN_POINT('Ctrl Pts',(217.505939289048,6.92547022714963,-9.21905848894597));
#36579=CARTESIAN_POINT('Ctrl Pts',(217.624412440706,10.4796059636719,-4.80947358199571));
#36580=CARTESIAN_POINT('Ctrl Pts',(217.742885592365,11.5054291016218,0.760446235638654));
#36581=CARTESIAN_POINT('Ctrl Pts',(217.861358744023,9.75544927040927,6.14690058665455));
#36582=CARTESIAN_POINT('Ctrl Pts',(217.979831895681,5.65186708233216,10.0503520223619));
#36583=CARTESIAN_POINT('Ctrl Pts',(218.098305047339,0.184713897477963,11.5290527826799));
#36584=CARTESIAN_POINT('Ctrl Pts',(218.216778198998,-5.32700341275905,10.2262511180883));
#36585=CARTESIAN_POINT('Ctrl Pts',(218.335251350656,-9.55352642391547,6.4562613142035));
#36586=CARTESIAN_POINT('Ctrl Pts',(218.453724502315,-11.4751630393333,1.12863214134426));
#36587=CARTESIAN_POINT('Ctrl Pts',(218.572197653973,-10.6282986840452,-4.47129113036288));
#36588=CARTESIAN_POINT('Ctrl Pts',(218.690670805631,-7.21724808383853,-8.99246948207381));
#36589=CARTESIAN_POINT('Ctrl Pts',(218.809143957289,-2.06496223864743,-11.3441221891729));
#36590=CARTESIAN_POINT('Ctrl Pts',(218.927617108948,3.58551696051438,-10.9588888768492));
#36591=CARTESIAN_POINT('Ctrl Pts',(219.046090260606,8.37095335800593,-7.92971103942582));
#36592=CARTESIAN_POINT('Ctrl Pts',(219.164563412264,11.1368112607131,-2.98740894949973));
#36593=CARTESIAN_POINT('Ctrl Pts',(219.283036563923,11.2157990354753,2.67563623960653));
#36594=CARTESIAN_POINT('Ctrl Pts',(219.401509715581,8.58886006959068,7.69315669910092));
#36595=CARTESIAN_POINT('Ctrl Pts',(219.519982867239,3.8897703770425,10.8546240695241));
#36596=CARTESIAN_POINT('Ctrl Pts',(219.638456018897,-1.74776638133898,11.3973018738637));
#36597=CARTESIAN_POINT('Ctrl Pts',(219.756929170556,-6.96363654138209,9.19026350689656));
#36598=CARTESIAN_POINT('Ctrl Pts',(219.875402322214,-10.4994578539298,4.76597966873598));
#36599=CARTESIAN_POINT('Ctrl Pts',(219.993875473873,-11.50217707989,-0.808145755784987));
#36600=CARTESIAN_POINT('Ctrl Pts',(220.112348625531,-9.72987795281957,-6.18729765367837));
#36601=CARTESIAN_POINT('Ctrl Pts',(220.230821777189,-5.61014574409689,-10.0737005557397));
#36602=CARTESIAN_POINT('Ctrl Pts',(220.349294928847,-0.136908381828727,
-11.5297194437361));
#36603=CARTESIAN_POINT('Ctrl Pts',(220.467768080506,5.36935983023475,-10.20407562191));
#36604=CARTESIAN_POINT('Ctrl Pts',(220.586241232164,9.58021420357832,-6.41659256981546));
#36605=CARTESIAN_POINT('Ctrl Pts',(220.704714383822,11.4797447729354,-1.08104305857399));
#36606=CARTESIAN_POINT('Ctrl Pts',(220.823187535481,10.6096662804338,4.51532424750848));
#36607=CARTESIAN_POINT('Ctrl Pts',(220.941660687139,7.17990244444507,9.02231263897793));
#36608=CARTESIAN_POINT('Ctrl Pts',(221.060133838797,2.01790159414706,11.3525974650078));
#36609=CARTESIAN_POINT('Ctrl Pts',(221.178606990456,-3.63091411613088,10.9439054680865));
#36610=CARTESIAN_POINT('Ctrl Pts',(221.297080142114,-8.40378593687573,7.89498012503259));
#36611=CARTESIAN_POINT('Ctrl Pts',(221.415553293773,-11.1490504371411,2.94110909442268));
#36612=CARTESIAN_POINT('Ctrl Pts',(221.53402644543,-11.2047153301085,-2.72190910822649));
#36613=CARTESIAN_POINT('Ctrl Pts',(221.652499597089,-8.55664415334701,-7.72908455304227));
#36614=CARTESIAN_POINT('Ctrl Pts',(221.731481698195,-5.41558793727451,-9.82229523321173));
#36615=CARTESIAN_POINT('Ctrl Pts',(221.770972748747,-3.68981949298323,-10.4326641617422));
#36616=CARTESIAN_POINT('Ctrl Pts',(221.275,-3.97626028075622,-11.2425521648637));
#36617=CARTESIAN_POINT('Ctrl Pts',(221.235508949447,-5.83600017639738,-10.5848002797813));
#36618=CARTESIAN_POINT('Ctrl Pts',(221.196017898894,-7.52844842425034,-9.45694693863041));
#36619=CARTESIAN_POINT('Ctrl Pts',(221.156526848342,-8.85027938390384,-7.99370649955156));
#36620=CARTESIAN_POINT('Ctrl Pts',(221.117035797789,-10.1721103435575,-6.53046606047255));
#36621=CARTESIAN_POINT('Ctrl Pts',(221.077544747236,-11.1233240150115,-4.73183852346552));
#36622=CARTESIAN_POINT('Ctrl Pts',(221.038053696683,-11.5889331573844,-2.81541834495975));
#36623=CARTESIAN_POINT('Ctrl Pts',(221.019088080173,-11.8125424135174,-1.8950556382265));
#36624=CARTESIAN_POINT('Ctrl Pts',(221.000122463662,-11.9241513443901,-0.947525116180473));
#36625=CARTESIAN_POINT('Ctrl Pts',(220.981156847152,-11.9240411815327,1.80394148113772E-5));
#36626=CARTESIAN_POINT('Origin',(212.6,0.,0.));
#36627=CARTESIAN_POINT('Origin',(221.275,0.,0.));
#36628=CARTESIAN_POINT('Origin',(158.,0.,0.));
#36629=CARTESIAN_POINT('',(166.,-16.55,-2.02679045258887E-15));
#36630=CARTESIAN_POINT('Origin',(166.,0.,0.));
#36631=CARTESIAN_POINT('',(150.,-16.55,-2.02679045258887E-15));
#36632=CARTESIAN_POINT('',(158.,-16.55,-2.02679045258887E-15));
#36633=CARTESIAN_POINT('Origin',(150.,0.,0.));
#36634=CARTESIAN_POINT('Origin',(150.,22.2,0.));
#36635=CARTESIAN_POINT('',(150.,-22.2,-2.71871589410712E-15));
#36636=CARTESIAN_POINT('Origin',(150.,0.,0.));
#36637=CARTESIAN_POINT('Origin',(150.4,0.,0.));
#36638=CARTESIAN_POINT('',(150.4,-22.6,-2.76770176607302E-15));
#36639=CARTESIAN_POINT('Origin',(221.6,0.,0.));
#36640=CARTESIAN_POINT('',(222.,-11.2,-1.37160441504503E-15));
#36641=CARTESIAN_POINT('Origin',(222.,0.,0.));
#36642=CARTESIAN_POINT('',(221.6,-11.6,-1.42059028701093E-15));
#36643=CARTESIAN_POINT('Origin',(222.,5.05,0.));
#36644=CARTESIAN_POINT('',(222.,-5.05,-6.18446633569413E-16));
#36645=CARTESIAN_POINT('Origin',(222.,0.,0.));
#36646=CARTESIAN_POINT('Origin',(209.,0.,0.));
#36647=CARTESIAN_POINT('',(196.,-5.05,-6.18446633569413E-16));
#36648=CARTESIAN_POINT('',(209.,-5.05,-6.18446633569413E-16));
#36649=CARTESIAN_POINT('Origin',(196.,0.,0.));
#36650=CARTESIAN_POINT('Origin',(196.,17.5,0.));
#36651=CARTESIAN_POINT('',(196.,-17.5,-2.14313189850787E-15));
#36652=CARTESIAN_POINT('Origin',(196.,0.,0.));
#36653=CARTESIAN_POINT('Origin',(181.,0.,0.));
#36654=CARTESIAN_POINT('',(166.,-17.5,-2.14313189850787E-15));
#36655=CARTESIAN_POINT('',(181.,-17.5,-2.14313189850787E-15));
#36656=CARTESIAN_POINT('Origin',(166.,0.,0.));
#36657=CARTESIAN_POINT('Origin',(166.,16.55,0.));
#36658=CARTESIAN_POINT('',(0.,0.,0.));
#36659=CARTESIAN_POINT('Origin',(215.7,0.,0.));
#36660=CARTESIAN_POINT('',(209.664320454657,-4.9420180477033,0.000126580456323855));
#36661=CARTESIAN_POINT('',(209.519679545343,-4.94198289688221,9.21666299965981E-5));
#36662=CARTESIAN_POINT('',(215.7,-4.942,-6.05220448138622E-16));
#36663=CARTESIAN_POINT('',(209.342,2.16926434203831,4.44056974845354));
#36664=CARTESIAN_POINT('Ctrl Pts',(209.664320454657,-4.9420180477033,0.000126580456323855));
#36665=CARTESIAN_POINT('Ctrl Pts',(209.658355941445,-4.9422072805368,0.185328915025629));
#36666=CARTESIAN_POINT('Ctrl Pts',(209.652391428234,-4.93199568223875,0.370510473892667));
#36667=CARTESIAN_POINT('Ctrl Pts',(209.646426915022,-4.91122249414261,0.554499541264965));
#36668=CARTESIAN_POINT('Ctrl Pts',(209.620030391337,-4.81928876339832,1.36876075631831));
#36669=CARTESIAN_POINT('Ctrl Pts',(209.593633867651,-4.52049682480743,2.15966595601887));
#36670=CARTESIAN_POINT('Ctrl Pts',(209.567237343965,-4.05107496711084,2.83131889085814));
#36671=CARTESIAN_POINT('Ctrl Pts',(209.540840820279,-3.58165310941424,3.50297182569741));
#36672=CARTESIAN_POINT('Ctrl Pts',(209.514444296593,-2.94160133261193,4.05537249567538));
#36673=CARTESIAN_POINT('Ctrl Pts',(209.488047772907,-2.20852840820168,4.42153669317007));
#36674=CARTESIAN_POINT('Ctrl Pts',(209.461651249221,-1.47545548379142,4.78770089066475));
#36675=CARTESIAN_POINT('Ctrl Pts',(209.435254725536,-0.649361411773217,
4.96762861567614));
#36676=CARTESIAN_POINT('Ctrl Pts',(209.40885820185,0.16959176212969,4.93951348019594));
#36677=CARTESIAN_POINT('Ctrl Pts',(209.386572134567,0.861017866287247,4.9157764226786));
#36678=CARTESIAN_POINT('Ctrl Pts',(209.364286067283,1.54735387132166,4.74374446378248));
#36679=CARTESIAN_POINT('Ctrl Pts',(209.342,2.1693573297895,4.44063731407458));
#36680=CARTESIAN_POINT('',(209.342,-2.16917135428513,4.44050218283347));
#36681=CARTESIAN_POINT('Origin',(209.342,0.,0.));
#36682=CARTESIAN_POINT('Ctrl Pts',(209.342,-2.16917135428514,4.44050218283347));
#36683=CARTESIAN_POINT('Ctrl Pts',(209.368396523686,-2.90564751248118,4.08073589521655));
#36684=CARTESIAN_POINT('Ctrl Pts',(209.394793047372,-3.55049743892233,3.53432461158655));
#36685=CARTESIAN_POINT('Ctrl Pts',(209.421189571058,-4.02583336624512,2.86696358887512));
#36686=CARTESIAN_POINT('Ctrl Pts',(209.447586094743,-4.50116929356792,2.19960256616367));
#36687=CARTESIAN_POINT('Ctrl Pts',(209.473982618429,-4.80699122177235,1.41129180437078));
#36688=CARTESIAN_POINT('Ctrl Pts',(209.500379142115,-4.90613404925993,0.597858302054359));
#36689=CARTESIAN_POINT('Ctrl Pts',(209.506812609858,-4.93029754101932,0.399604991874226));
#36690=CARTESIAN_POINT('Ctrl Pts',(209.5132460776,-4.94218400193112,0.199859355380918));
#36691=CARTESIAN_POINT('Ctrl Pts',(209.519679545343,-4.94198289688221,9.21666299965981E-5));
#36692=CARTESIAN_POINT('Origin',(215.7,0.,0.));
#36693=CARTESIAN_POINT('',(210.664320454657,-4.94221937800576,-0.000104761278833521));
#36694=CARTESIAN_POINT('',(210.519679545343,-4.94226008201731,-9.58615277245487E-5));
#36695=CARTESIAN_POINT('',(215.7,-4.942,-6.05220448138622E-16));
#36696=CARTESIAN_POINT('Ctrl Pts',(210.664320454657,-4.94221937800576,-0.000104761278833521));
#36697=CARTESIAN_POINT('Ctrl Pts',(210.641780892342,-4.941563040604,0.699682317088681));
#36698=CARTESIAN_POINT('Ctrl Pts',(210.619241330028,-4.79143840278129,1.39974202050533));
#36699=CARTESIAN_POINT('Ctrl Pts',(210.596701767713,-4.50302543707184,2.03723795764061));
#36700=CARTESIAN_POINT('Ctrl Pts',(210.570305244027,-4.16525935384578,2.78382195822132));
#36701=CARTESIAN_POINT('Ctrl Pts',(210.543908720341,-3.63782790166743,3.44459842901169));
#36702=CARTESIAN_POINT('Ctrl Pts',(210.517512196655,-2.98468296975735,3.93944718870812));
#36703=CARTESIAN_POINT('Ctrl Pts',(210.491115672969,-2.33153803784727,4.43429594840454));
#36704=CARTESIAN_POINT('Ctrl Pts',(210.464719149284,-1.55267962620546,4.76321699700701));
#36705=CARTESIAN_POINT('Ctrl Pts',(210.438322625598,-0.742545536773605,
4.88632814185778));
#36706=CARTESIAN_POINT('Ctrl Pts',(210.411926101912,0.0675885526582515,
5.00943928670855));
#36707=CARTESIAN_POINT('Ctrl Pts',(210.385529578226,0.908998319880143,4.92674052780762));
#36708=CARTESIAN_POINT('Ctrl Pts',(210.35913305454,1.67966151371283,4.64825922034747));
#36709=CARTESIAN_POINT('Ctrl Pts',(210.332736530854,2.45032470754551,4.36977791288732));
#36710=CARTESIAN_POINT('Ctrl Pts',(210.306340007169,3.15024132798898,3.89551405686796));
#36711=CARTESIAN_POINT('Ctrl Pts',(210.279943483483,3.69454538824977,3.28297288476245));
#36712=CARTESIAN_POINT('Ctrl Pts',(210.253546959797,4.23884944851057,2.67043171265694));
#36713=CARTESIAN_POINT('Ctrl Pts',(210.227150436111,4.62754094858869,1.91961322446529));
#36714=CARTESIAN_POINT('Ctrl Pts',(210.200753912425,4.81349043727808,1.12155534276936));
#36715=CARTESIAN_POINT('Ctrl Pts',(210.174357388739,4.99943992596747,0.323497461073427));
#36716=CARTESIAN_POINT('Ctrl Pts',(210.147960865053,4.98264740326812,-0.521799814126788));
#36717=CARTESIAN_POINT('Ctrl Pts',(210.121564341368,4.76514898523828,-1.31184287638444));
#36718=CARTESIAN_POINT('Ctrl Pts',(210.095167817682,4.54765056720844,-2.10188593864209));
#36719=CARTESIAN_POINT('Ctrl Pts',(210.068771293996,4.12944625384811,-2.83667478795718));
#36720=CARTESIAN_POINT('Ctrl Pts',(210.04237477031,3.5612439805398,-3.42711510149462));
#36721=CARTESIAN_POINT('Ctrl Pts',(210.015978246624,2.99304170723149,-4.01755541503206));
#36722=CARTESIAN_POINT('Ctrl Pts',(209.989581722938,2.27484147397519,-4.46364719279186));
#36723=CARTESIAN_POINT('Ctrl Pts',(209.963185199253,1.49372616717388,-4.71130116034573));
#36724=CARTESIAN_POINT('Ctrl Pts',(209.936788675567,0.712610860372571,-4.95895512789961));
#36725=CARTESIAN_POINT('Ctrl Pts',(209.910392151881,-0.13141951997376,-5.00817128524755));
#36726=CARTESIAN_POINT('Ctrl Pts',(209.883995628195,-0.936024934326331,
-4.85298198583465));
#36727=CARTESIAN_POINT('Ctrl Pts',(209.857599104509,-1.7406303486789,-4.69779268642175));
#36728=CARTESIAN_POINT('Ctrl Pts',(209.831202580823,-2.50581079703771,-4.33819793024801));
#36729=CARTESIAN_POINT('Ctrl Pts',(209.804806057137,-3.1387870254314,-3.81779937891553));
#36730=CARTESIAN_POINT('Ctrl Pts',(209.778409533452,-3.7717632538251,-3.29740082758306));
#36731=CARTESIAN_POINT('Ctrl Pts',(209.752013009766,-4.27253526225367,-2.61619848109185));
#36732=CARTESIAN_POINT('Ctrl Pts',(209.72561648608,-4.58038350501912,-1.85678869264318));
#36733=CARTESIAN_POINT('Ctrl Pts',(209.705184475606,-4.81867088693121,-1.26897383730318));
#36734=CARTESIAN_POINT('Ctrl Pts',(209.684752465131,-4.9413698125332,-0.634301730049446));
#36735=CARTESIAN_POINT('Ctrl Pts',(209.664320454657,-4.9420180477033,0.000126580456323855));
#36736=CARTESIAN_POINT('Ctrl Pts',(209.519679545343,-4.94198289688221,9.21666299965981E-5));
#36737=CARTESIAN_POINT('Ctrl Pts',(209.539642601286,-4.94135886774234,-0.619785592014529));
#36738=CARTESIAN_POINT('Ctrl Pts',(209.559605657229,-4.82434832763514,-1.23987086903581));
#36739=CARTESIAN_POINT('Ctrl Pts',(209.579568713173,-4.59661203239717,-1.81622046758434));
#36740=CARTESIAN_POINT('Ctrl Pts',(209.605965236859,-4.2954834612761,-2.57830949206667));
#36741=CARTESIAN_POINT('Ctrl Pts',(209.632361760544,-3.80076259226322,-3.26393129819136));
#36742=CARTESIAN_POINT('Ctrl Pts',(209.65875828423,-3.17241385187217,-3.78990976178524));
#36743=CARTESIAN_POINT('Ctrl Pts',(209.685154807916,-2.54406511148113,-4.31588822537912));
#36744=CARTESIAN_POINT('Ctrl Pts',(209.711551331602,-1.7820884997119,-4.68222334644218));
#36745=CARTESIAN_POINT('Ctrl Pts',(209.737947855288,-0.978885076945217,
-4.8445163738841));
#36746=CARTESIAN_POINT('Ctrl Pts',(209.764344378974,-0.175681654178535,
-5.00680940132602));
#36747=CARTESIAN_POINT('Ctrl Pts',(209.790740902659,0.668748579585601,-4.96506033514679));
#36748=CARTESIAN_POINT('Ctrl Pts',(209.817137426345,1.45202191277295,-4.72432184612485));
#36749=CARTESIAN_POINT('Ctrl Pts',(209.843533950031,2.2352952459603,-4.48358335710292));
#36750=CARTESIAN_POINT('Ctrl Pts',(209.869930473717,2.95741167857085,-4.04385544523827));
#36751=CARTESIAN_POINT('Ctrl Pts',(209.896326997403,3.53081120871917,-3.45846025712288));
#36752=CARTESIAN_POINT('Ctrl Pts',(209.922723521089,4.10421073886749,-2.87306506900749));
#36753=CARTESIAN_POINT('Ctrl Pts',(209.949120044775,4.52889336655357,-2.14200260464136));
#36754=CARTESIAN_POINT('Ctrl Pts',(209.97551656846,4.75336671917514,-1.35391323544134));
#36755=CARTESIAN_POINT('Ctrl Pts',(210.001913092146,4.97784007179672,-0.565823866241315));
#36756=CARTESIAN_POINT('Ctrl Pts',(210.028309615832,5.00210414935379,0.279292407792593));
#36757=CARTESIAN_POINT('Ctrl Pts',(210.054706139518,4.82321639471094,1.07896292800015));
#36758=CARTESIAN_POINT('Ctrl Pts',(210.081102663204,4.64432864006809,1.8786334482077));
#36759=CARTESIAN_POINT('Ctrl Pts',(210.10749918689,4.26228905322531,2.63285821458891));
#36760=CARTESIAN_POINT('Ctrl Pts',(210.133895710575,3.72342076754685,3.25018675848713));
#36761=CARTESIAN_POINT('Ctrl Pts',(210.160292234261,3.18455248186838,3.86751530238536));
#36762=CARTESIAN_POINT('Ctrl Pts',(210.186688757947,2.48885549735423,4.34794762380061));
#36763=CARTESIAN_POINT('Ctrl Pts',(210.213085281633,1.72068405168742,4.63323033259046));
#36764=CARTESIAN_POINT('Ctrl Pts',(210.239481805319,0.952512606020613,4.91851304138032));
#36765=CARTESIAN_POINT('Ctrl Pts',(210.265878329005,0.11186669920115,5.00864613754478));
#36766=CARTESIAN_POINT('Ctrl Pts',(210.292274852691,-0.699323984278334,
4.8927009452202));
#36767=CARTESIAN_POINT('Ctrl Pts',(210.318671376376,-1.51051466775782,4.77675575289561));
#36768=CARTESIAN_POINT('Ctrl Pts',(210.345067900062,-2.29225012789733,4.45473227208197));
#36769=CARTESIAN_POINT('Ctrl Pts',(210.371464423748,-2.94974374088599,3.96567630539273));
#36770=CARTESIAN_POINT('Ctrl Pts',(210.397860947434,-3.60723735387464,3.4766203387035));
#36771=CARTESIAN_POINT('Ctrl Pts',(210.42425747112,-4.14048911971245,2.82053188613866));
#36772=CARTESIAN_POINT('Ctrl Pts',(210.450653994806,-4.48484141537169,2.07696272260168));
#36773=CARTESIAN_POINT('Ctrl Pts',(210.473662511651,-4.78499592396769,1.42883102810752));
#36774=CARTESIAN_POINT('Ctrl Pts',(210.496671028497,-4.94162974142002,0.714233863442395));
#36775=CARTESIAN_POINT('Ctrl Pts',(210.519679545343,-4.94226008201731,-9.58615277245487E-5));
#36776=CARTESIAN_POINT('Origin',(215.7,0.,0.));
#36777=CARTESIAN_POINT('',(211.664320454657,-4.9415897287205,1.37434265569392E-5));
#36778=CARTESIAN_POINT('',(211.519679545343,-4.94158749800685,3.21734411369081E-7));
#36779=CARTESIAN_POINT('',(215.7,-4.942,-6.05220448138622E-16));
#36780=CARTESIAN_POINT('Ctrl Pts',(211.664320454657,-4.9415897287205,1.37434265569392E-5));
#36781=CARTESIAN_POINT('Ctrl Pts',(211.651602366925,-4.94162817182109,0.395017559605729));
#36782=CARTESIAN_POINT('Ctrl Pts',(211.638884279193,-4.89482715788202,0.790012419678822));
#36783=CARTESIAN_POINT('Ctrl Pts',(211.626166191461,-4.80108290976675,1.17353290387558));
#36784=CARTESIAN_POINT('Ctrl Pts',(211.599769667775,-4.60651574543051,1.96953366739189));
#36785=CARTESIAN_POINT('Ctrl Pts',(211.573373144089,-4.20972916787737,2.7161057624864));
#36786=CARTESIAN_POINT('Ctrl Pts',(211.546976620403,-3.65883417083036,3.32272615382265));
#36787=CARTESIAN_POINT('Ctrl Pts',(211.520580096718,-3.10793917378334,3.92934654515892));
#36788=CARTESIAN_POINT('Ctrl Pts',(211.494183573032,-2.40293575724243,4.39601523273692));
#36789=CARTESIAN_POINT('Ctrl Pts',(211.467787049346,-1.62930668919103,4.66614790758825));
#36790=CARTESIAN_POINT('Ctrl Pts',(211.44139052566,-0.855677621139631,4.9362805824396));
#36791=CARTESIAN_POINT('Ctrl Pts',(211.414994001974,-0.0134229015777539,
5.00987724456428));
#36792=CARTESIAN_POINT('Ctrl Pts',(211.388597478288,0.795332766144239,4.87801418345934));
#36793=CARTESIAN_POINT('Ctrl Pts',(211.362200954603,1.60408843386621,4.7461511223544));
#36794=CARTESIAN_POINT('Ctrl Pts',(211.335804430917,2.37934504974831,4.40882833801985));
#36795=CARTESIAN_POINT('Ctrl Pts',(211.309407907231,3.02710153540114,3.90694674615674));
#36796=CARTESIAN_POINT('Ctrl Pts',(211.283011383545,3.67485802105398,3.40506515429362));
#36797=CARTESIAN_POINT('Ctrl Pts',(211.256614859859,4.19511437647758,2.73862475490193));
#36798=CARTESIAN_POINT('Ctrl Pts',(211.230218336173,4.52478870408222,1.98843248976257));
#36799=CARTESIAN_POINT('Ctrl Pts',(211.203821812487,4.85446303168686,1.23824022462321));
#36800=CARTESIAN_POINT('Ctrl Pts',(211.177425288802,4.99355533147254,0.404296093736161));
#36801=CARTESIAN_POINT('Ctrl Pts',(211.151028765116,4.92520044433258,-0.412282871435125));
#36802=CARTESIAN_POINT('Ctrl Pts',(211.12463224143,4.85684555719262,-1.22886183660641));
#36803=CARTESIAN_POINT('Ctrl Pts',(211.098235717744,4.58104348312702,-2.02807563606193));
#36804=CARTESIAN_POINT('Ctrl Pts',(211.071839194058,4.13123565540155,-2.7130183453989));
#36805=CARTESIAN_POINT('Ctrl Pts',(211.045442670372,3.68142782767608,-3.39796105473587));
#36806=CARTESIAN_POINT('Ctrl Pts',(211.019046146687,3.05761424629074,-3.9686326739543));
#36807=CARTESIAN_POINT('Ctrl Pts',(210.992649623001,2.33543328460936,-4.35583837579821));
#36808=CARTESIAN_POINT('Ctrl Pts',(210.966253099315,1.61325232292797,-4.74304407764211));
#36809=CARTESIAN_POINT('Ctrl Pts',(210.939856575629,0.792703980950555,-4.94678386211149));
#36810=CARTESIAN_POINT('Ctrl Pts',(210.913460051943,-0.0267189702393086,
-4.942353961378));
#36811=CARTESIAN_POINT('Ctrl Pts',(210.887063528257,-0.846141921429158,
-4.93792406064451));
#36812=CARTESIAN_POINT('Ctrl Pts',(210.860667004571,-1.66443948183145,-4.72532447470816));
#36813=CARTESIAN_POINT('Ctrl Pts',(210.834270480886,-2.38239179114626,-4.33033323618878));
#36814=CARTESIAN_POINT('Ctrl Pts',(210.8078739572,-3.10034410046108,-3.9353419976694));
#36815=CARTESIAN_POINT('Ctrl Pts',(210.781477433514,-3.71795115868842,-3.35795910656698));
#36816=CARTESIAN_POINT('Ctrl Pts',(210.755080909828,-4.16032714312371,-2.66819314238538));
#36817=CARTESIAN_POINT('Ctrl Pts',(210.728684386142,-4.60270312755899,-1.97842717820379));
#36818=CARTESIAN_POINT('Ctrl Pts',(210.702287862456,-4.86984803820222,-1.17627814094302));
#36819=CARTESIAN_POINT('Ctrl Pts',(210.67589133877,-4.92937013638695,-0.359007857127102));
#36820=CARTESIAN_POINT('Ctrl Pts',(210.672034377399,-4.93806728288102,-0.239591378199565));
#36821=CARTESIAN_POINT('Ctrl Pts',(210.668177416028,-4.9423316902135,-0.1198520612323));
#36822=CARTESIAN_POINT('Ctrl Pts',(210.664320454657,-4.94221937800576,-0.000104761278833521));
#36823=CARTESIAN_POINT('Ctrl Pts',(210.519679545343,-4.94226008201731,-9.58615277245487E-5));
#36824=CARTESIAN_POINT('Ctrl Pts',(210.523067552183,-4.94235289974518,-0.10528099842556));
#36825=CARTESIAN_POINT('Ctrl Pts',(210.526455559023,-4.93906315687572,-0.210460336536133));
#36826=CARTESIAN_POINT('Ctrl Pts',(210.529843565863,-4.93235099880689,-0.315420813356548));
#36827=CARTESIAN_POINT('Ctrl Pts',(210.556240089549,-4.88005546110216,-1.13318531126868));
#36828=CARTESIAN_POINT('Ctrl Pts',(210.582636613235,-4.62001156021202,-1.93766443258382));
#36829=CARTESIAN_POINT('Ctrl Pts',(210.609033136921,-4.18375002366602,-2.63131381930358));
#36830=CARTESIAN_POINT('Ctrl Pts',(210.635429660607,-3.74748848712002,-3.32496320602334));
#36831=CARTESIAN_POINT('Ctrl Pts',(210.661826184293,-3.13500931491815,-3.90778285814772));
#36832=CARTESIAN_POINT('Ctrl Pts',(210.688222707978,-2.4205765667749,-4.30910498280575));
#36833=CARTESIAN_POINT('Ctrl Pts',(210.714619231664,-1.70614381863165,-4.71042710746378));
#36834=CARTESIAN_POINT('Ctrl Pts',(210.74101575535,-0.889757494547013,-4.93025170465545));
#36835=CARTESIAN_POINT('Ctrl Pts',(210.767412279036,-0.0704057138513457,
-4.94192469669601));
#36836=CARTESIAN_POINT('Ctrl Pts',(210.793808802722,0.748946066844314,-4.95359768873657));
#36837=CARTESIAN_POINT('Ctrl Pts',(210.820205326408,1.57126330415101,-4.75711907562602));
#36838=CARTESIAN_POINT('Ctrl Pts',(210.846601850093,2.29683874538686,-4.37631219733406));
#36839=CARTESIAN_POINT('Ctrl Pts',(210.872998373779,3.02241418662272,-3.99550531904209));
#36840=CARTESIAN_POINT('Ctrl Pts',(210.899394897465,3.65124783178774,-3.43037017556871));
#36841=CARTESIAN_POINT('Ctrl Pts',(210.925791421151,4.10709261705286,-2.74943028756545));
#36842=CARTESIAN_POINT('Ctrl Pts',(210.952187944837,4.56293740231798,-2.06849039956218));
#36843=CARTESIAN_POINT('Ctrl Pts',(210.978584468523,4.8457933276832,-1.27174576702903));
#36844=CARTESIAN_POINT('Ctrl Pts',(211.004980992209,4.92136366930947,-0.455802924132807));
#36845=CARTESIAN_POINT('Ctrl Pts',(211.031377515894,4.99693401093573,0.360139918763401));
#36846=CARTESIAN_POINT('Ctrl Pts',(211.05777403958,4.86521876882306,1.19528097202268));
#36847=CARTESIAN_POINT('Ctrl Pts',(211.084170563266,4.54218862231425,1.94835807552615));
#36848=CARTESIAN_POINT('Ctrl Pts',(211.110567086952,4.21915847580543,2.70143517902964));
#36849=CARTESIAN_POINT('Ctrl Pts',(211.136963610638,3.70481342490047,3.37244833277733));
#36850=CARTESIAN_POINT('Ctrl Pts',(211.163360134324,3.06151861224838,3.88003614133731));
#36851=CARTESIAN_POINT('Ctrl Pts',(211.189756658009,2.4182237995963,4.38762394989728));
#36852=CARTESIAN_POINT('Ctrl Pts',(211.216153181695,1.64597922519708,4.73178641326956));
#36853=CARTESIAN_POINT('Ctrl Pts',(211.242549705381,0.838420752701002,4.87079329397425));
#36854=CARTESIAN_POINT('Ctrl Pts',(211.268946229067,0.0308622802049217,
5.00980017467893));
#36855=CARTESIAN_POINT('Ctrl Pts',(211.295342752753,-0.812010090388028,
4.94365147271603));
#36856=CARTESIAN_POINT('Ctrl Pts',(211.321739276439,-1.58799676457591,4.68036782175277));
#36857=CARTESIAN_POINT('Ctrl Pts',(211.348135800125,-2.3639834387638,4.4170841707895));
#36858=CARTESIAN_POINT('Ctrl Pts',(211.37453232381,-3.07308441654662,3.95666557082588));
#36859=CARTESIAN_POINT('Ctrl Pts',(211.400928847496,-3.62932009422403,3.35493849792489));
#36860=CARTESIAN_POINT('Ctrl Pts',(211.427325371182,-4.18555577190144,2.7532114250239));
#36861=CARTESIAN_POINT('Ctrl Pts',(211.453721894868,-4.58892614947342,2.01017587918554));
#36862=CARTESIAN_POINT('Ctrl Pts',(211.480118418554,-4.79052193715797,1.21592608361099));
#36863=CARTESIAN_POINT('Ctrl Pts',(211.493305460817,-4.891234144716,0.81913877379881));
#36864=CARTESIAN_POINT('Ctrl Pts',(211.50649250308,-4.94158843063211,0.409569660407683));
#36865=CARTESIAN_POINT('Ctrl Pts',(211.519679545343,-4.94158749800685,3.21734411369081E-7));
#36866=CARTESIAN_POINT('Origin',(215.7,0.,0.));
#36867=CARTESIAN_POINT('',(212.664320454657,-4.94229966671163,8.50863313224884E-5));
#36868=CARTESIAN_POINT('',(212.519679545343,-4.94226196377334,9.54014550954459E-5));
#36869=CARTESIAN_POINT('',(215.7,-4.942,-6.05220448138622E-16));
#36870=CARTESIAN_POINT('Ctrl Pts',(212.664320454657,-4.94229966671163,8.50863313224884E-5));
#36871=CARTESIAN_POINT('Ctrl Pts',(212.661423841508,-4.94237235712893,0.0900121728263076));
#36872=CARTESIAN_POINT('Ctrl Pts',(212.658527228358,-4.93996817019507,0.179935373971945));
#36873=CARTESIAN_POINT('Ctrl Pts',(212.655630615209,-4.93506096691248,0.269721774778861));
#36874=CARTESIAN_POINT('Ctrl Pts',(212.629234091523,-4.89034215186677,1.08793557601746));
#36875=CARTESIAN_POINT('Ctrl Pts',(212.602837567838,-4.63776082920043,1.89478881963755));
#36876=CARTESIAN_POINT('Ctrl Pts',(212.576441044152,-4.20794287971893,2.59244928666999));
#36877=CARTESIAN_POINT('Ctrl Pts',(212.550044520466,-3.77812493023742,3.29010975370243));
#36878=CARTESIAN_POINT('Ctrl Pts',(212.52364799678,-3.17107035394075,3.87857744414721));
#36879=CARTESIAN_POINT('Ctrl Pts',(212.497251473094,-2.46038546858754,4.28649972925419));
#36880=CARTESIAN_POINT('Ctrl Pts',(212.470854949408,-1.74970058323433,4.69442201436117));
#36881=CARTESIAN_POINT('Ctrl Pts',(212.444458425722,-0.935385388824589,
4.92179889413036));
#36882=CARTESIAN_POINT('Ctrl Pts',(212.418061902037,-0.116176877542877,
4.94106056591673));
#36883=CARTESIAN_POINT('Ctrl Pts',(212.391665378351,0.703031633738836,4.9603222377031));
#36884=CARTESIAN_POINT('Ctrl Pts',(212.365268854665,1.52713346189252,4.77146870150665));
#36885=CARTESIAN_POINT('Ctrl Pts',(212.338872330979,2.25620497007056,4.39739874425346));
#36886=CARTESIAN_POINT('Ctrl Pts',(212.312475807293,2.9852764782486,4.02332878700027));
#36887=CARTESIAN_POINT('Ctrl Pts',(212.286079283607,3.61931766645099,3.46404240869033));
#36888=CARTESIAN_POINT('Ctrl Pts',(212.259682759921,4.08145004797628,2.78735395829224));
#36889=CARTESIAN_POINT('Ctrl Pts',(212.233286236236,4.54358242950156,2.11066550789415));
#36890=CARTESIAN_POINT('Ctrl Pts',(212.20688971255,4.83380600434973,1.31657498540791));
#36891=CARTESIAN_POINT('Ctrl Pts',(212.180493188864,4.91693070970694,0.501367109884335));
#36892=CARTESIAN_POINT('Ctrl Pts',(212.154096665178,5.00005541506415,-0.313840765639247));
#36893=CARTESIAN_POINT('Ctrl Pts',(212.127700141492,4.87608125093039,-1.15016599420016));
#36894=CARTESIAN_POINT('Ctrl Pts',(212.101303617806,4.56004027879635,-1.90620283251492));
#36895=CARTESIAN_POINT('Ctrl Pts',(212.07490709412,4.2439993066623,-2.66223967082967));
#36896=CARTESIAN_POINT('Ctrl Pts',(212.048510570435,3.73589152652797,-3.33798811889825));
#36897=CARTESIAN_POINT('Ctrl Pts',(212.022114046749,3.09732580220978,-3.85151261946505));
#36898=CARTESIAN_POINT('Ctrl Pts',(211.995717523063,2.45876007789159,-4.36503712003185));
#36899=CARTESIAN_POINT('Ctrl Pts',(211.969320999377,1.68973640938953,-4.71633767309686));
#36900=CARTESIAN_POINT('Ctrl Pts',(211.942924475691,0.883500120465094,-4.86281853661754));
#36901=CARTESIAN_POINT('Ctrl Pts',(211.916527952005,0.0772638315406597,
-5.00929940013821));
#36902=CARTESIAN_POINT('Ctrl Pts',(211.89013142832,-0.766185077806151,-4.95096057411454));
#36903=CARTESIAN_POINT('Ctrl Pts',(211.863734904634,-1.54457710684397,-4.69487573253505));
#36904=CARTESIAN_POINT('Ctrl Pts',(211.837338380948,-2.32296913588178,-4.43879089095556));
#36905=CARTESIAN_POINT('Ctrl Pts',(211.810941857262,-3.03630428461059,-3.98496003382025));
#36906=CARTESIAN_POINT('Ctrl Pts',(211.784545333576,-3.59808954947537,-3.38841086305795));
#36907=CARTESIAN_POINT('Ctrl Pts',(211.75814880989,-4.15987481434016,-2.79186169229563));
#36908=CARTESIAN_POINT('Ctrl Pts',(211.731752286205,-4.5701101953409,-2.0525942079063));
#36909=CARTESIAN_POINT('Ctrl Pts',(211.705355762519,-4.77905401028161,-1.26024574974258));
#36910=CARTESIAN_POINT('Ctrl Pts',(211.691677326565,-4.88732677470474,-0.849658061487058));
#36911=CARTESIAN_POINT('Ctrl Pts',(211.677998890611,-4.941548382765,-0.424816979164754));
#36912=CARTESIAN_POINT('Ctrl Pts',(211.664320454657,-4.9415897287205,1.37434265569392E-5));
#36913=CARTESIAN_POINT('Ctrl Pts',(211.519679545343,-4.94158749800685,3.21734411369081E-7));
#36914=CARTESIAN_POINT('Ctrl Pts',(211.532889026766,-4.94158656379464,-0.410265942875176));
#36915=CARTESIAN_POINT('Ctrl Pts',(211.546098508189,-4.89105889568341,-0.820532433534242));
#36916=CARTESIAN_POINT('Ctrl Pts',(211.559307989611,-4.79000721059605,-1.21795221319883));
#36917=CARTESIAN_POINT('Ctrl Pts',(211.585704513297,-4.58807549855246,-2.01211666912335));
#36918=CARTESIAN_POINT('Ctrl Pts',(211.612101036983,-4.18439087666816,-2.75498153566165));
#36919=CARTESIAN_POINT('Ctrl Pts',(211.638497560669,-3.62790073734079,-3.3564732847439));
#36920=CARTESIAN_POINT('Ctrl Pts',(211.664894084355,-3.07141059801342,-3.95796503382616));
#36921=CARTESIAN_POINT('Ctrl Pts',(211.691290608041,-2.36211494124297,-4.41808366545237));
#36922=CARTESIAN_POINT('Ctrl Pts',(211.717687131727,-1.58601697586039,-4.68103907519265));
#36923=CARTESIAN_POINT('Ctrl Pts',(211.744083655412,-0.809919010477825,
-4.94399448493293));
#36924=CARTESIAN_POINT('Ctrl Pts',(211.770480179098,0.0329812635168701,
-5.00978667278729));
#36925=CARTESIAN_POINT('Ctrl Pts',(211.796876702784,0.840480868287655,-4.87043823297658));
#36926=CARTESIAN_POINT('Ctrl Pts',(211.82327322647,1.64798047305844,-4.73108979316587));
#36927=CARTESIAN_POINT('Ctrl Pts',(211.849669750156,2.42007940860532,-4.38660072569009));
#36928=CARTESIAN_POINT('Ctrl Pts',(211.876066273842,3.06315947022311,-3.87874086930026));
#36929=CARTESIAN_POINT('Ctrl Pts',(211.902462797527,3.7062395318409,-3.37088101291043));
#36930=CARTESIAN_POINT('Ctrl Pts',(211.928859321213,4.22030071952961,-2.69965036760654));
#36931=CARTESIAN_POINT('Ctrl Pts',(211.955255844899,4.54301230948639,-1.94643669998611));
#36932=CARTESIAN_POINT('Ctrl Pts',(211.981652368585,4.86572389944316,-1.19322303236568));
#36933=CARTESIAN_POINT('Ctrl Pts',(212.008048892271,4.99708589166801,-0.358026342428714));
#36934=CARTESIAN_POINT('Ctrl Pts',(212.034445415957,4.92117043894809,0.457884463616269));
#36935=CARTESIAN_POINT('Ctrl Pts',(212.060841939643,4.84525498622817,1.27379526966126));
#36936=CARTESIAN_POINT('Ctrl Pts',(212.087238463328,4.56206208856348,2.07042019181425));
#36937=CARTESIAN_POINT('Ctrl Pts',(212.113634987014,4.10592932815241,2.75116721109706));
#36938=CARTESIAN_POINT('Ctrl Pts',(212.1400315107,3.64979656774134,3.43191423037987));
#36939=CARTESIAN_POINT('Ctrl Pts',(212.166428034386,3.02072394458389,3.9967833467925));
#36940=CARTESIAN_POINT('Ctrl Pts',(212.192824558072,2.29498749909123,4.37728329563128));
#36941=CARTESIAN_POINT('Ctrl Pts',(212.219221081758,1.56925105359856,4.75778324447007));
#36942=CARTESIAN_POINT('Ctrl Pts',(212.245617605443,0.746850785770678,4.95391402573501));
#36943=CARTESIAN_POINT('Ctrl Pts',(212.272014129129,-0.072495984398216,
4.94189447514248));
#36944=CARTESIAN_POINT('Ctrl Pts',(212.298410652815,-0.89184275456711,4.92987492454996));
#36945=CARTESIAN_POINT('Ctrl Pts',(212.324807176501,-1.70813602707702,4.70970504209997));
#36946=CARTESIAN_POINT('Ctrl Pts',(212.351203700187,-2.42239896467692,4.30808077072957));
#36947=CARTESIAN_POINT('Ctrl Pts',(212.377600223873,-3.13666190227682,3.90645649935917));
#36948=CARTESIAN_POINT('Ctrl Pts',(212.403996747559,-3.74889450496672,3.32337783906836));
#36949=CARTESIAN_POINT('Ctrl Pts',(212.430393271244,-4.18486261118127,2.62954399026423));
#36950=CARTESIAN_POINT('Ctrl Pts',(212.45678979493,-4.62083071739583,1.93571014146011));
#36951=CARTESIAN_POINT('Ctrl Pts',(212.483186318616,-4.88053432713503,1.13112110414268));
#36952=CARTESIAN_POINT('Ctrl Pts',(212.509582842302,-4.93248397113545,0.313334558722124));
#36953=CARTESIAN_POINT('Ctrl Pts',(212.512948409982,-4.93910757221779,0.209066436166142));
#36954=CARTESIAN_POINT('Ctrl Pts',(212.516313977663,-4.94235385099752,0.104583770228035));
#36955=CARTESIAN_POINT('Ctrl Pts',(212.519679545343,-4.94226196377334,9.54014550954459E-5));
#36956=CARTESIAN_POINT('Origin',(215.7,0.,0.));
#36957=CARTESIAN_POINT('',(213.664320454657,-4.94192591391644,-0.000125637169695325));
#36958=CARTESIAN_POINT('',(213.519679545343,-4.94197050942031,-0.000126753746856371));
#36959=CARTESIAN_POINT('',(215.7,-4.942,-6.05220448138622E-16));
#36960=CARTESIAN_POINT('Ctrl Pts',(213.664320454657,-4.94192591391644,-0.000125637169695325));
#36961=CARTESIAN_POINT('Ctrl Pts',(213.644848792405,-4.94133232753319,0.604515633599268));
#36962=CARTESIAN_POINT('Ctrl Pts',(213.625377130152,-4.8301532058668,1.20936919881882));
#36963=CARTESIAN_POINT('Ctrl Pts',(213.6059054679,-4.61324303097403,1.77357416537976));
#36964=CARTESIAN_POINT('Ctrl Pts',(213.579508944214,-4.31919137297763,2.53843181186435));
#36965=CARTESIAN_POINT('Ctrl Pts',(213.553112420528,-3.8308320314266,3.2285873268173));
#36966=CARTESIAN_POINT('Ctrl Pts',(213.526715896842,-3.2073793410417,3.76035827356807));
#36967=CARTESIAN_POINT('Ctrl Pts',(213.500319373156,-2.58392665065679,4.29212922031885));
#36968=CARTESIAN_POINT('Ctrl Pts',(213.473922849471,-1.82538061143801,4.66551559886746));
#36969=CARTESIAN_POINT('Ctrl Pts',(213.447526325785,-1.02371611819283,4.83524372625467));
#36970=CARTESIAN_POINT('Ctrl Pts',(213.421129802099,-0.222051624947664,
5.00497185364188));
#36971=CARTESIAN_POINT('Ctrl Pts',(213.394733278413,0.62273132232389,4.97104172986771));
#36972=CARTESIAN_POINT('Ctrl Pts',(213.368336754727,1.40820146870356,4.73756743555953));
#36973=CARTESIAN_POINT('Ctrl Pts',(213.341940231041,2.19367161508324,4.50409314125135));
#36974=CARTESIAN_POINT('Ctrl Pts',(213.315543707355,2.91982896057103,4.07107467640918));
#36975=CARTESIAN_POINT('Ctrl Pts',(213.28914718367,3.49862579018089,3.49101620781315));
#36976=CARTESIAN_POINT('Ctrl Pts',(213.262750659984,4.07742261979076,2.91095773921712));
#36977=CARTESIAN_POINT('Ctrl Pts',(213.236354136298,4.5088589335227,2.18385926686723));
#36978=CARTESIAN_POINT('Ctrl Pts',(213.209957612612,4.74062240289565,1.39788261885495));
#36979=CARTESIAN_POINT('Ctrl Pts',(213.183561088926,4.9723858722686,0.611905970842695));
#36980=CARTESIAN_POINT('Ctrl Pts',(213.15716456524,5.00447649728257,-0.232948852831949));
#36981=CARTESIAN_POINT('Ctrl Pts',(213.130768041555,4.83300323941469,-1.03424188212432));
#36982=CARTESIAN_POINT('Ctrl Pts',(213.104371517869,4.66152998154681,-1.83553491141671));
#36983=CARTESIAN_POINT('Ctrl Pts',(213.077974994183,4.28649284079707,-2.59326614632683));
#36984=CARTESIAN_POINT('Ctrl Pts',(213.051578470497,3.75336565762595,-3.21555948834523));
#36985=CARTESIAN_POINT('Ctrl Pts',(213.025181946811,3.22023847445484,-3.83785283036363));
#36986=CARTESIAN_POINT('Ctrl Pts',(212.998785423125,2.52902124886233,-4.32470827949033));
#36987=CARTESIAN_POINT('Ctrl Pts',(212.972388899439,1.7635251515962,-4.61709385031543));
#36988=CARTESIAN_POINT('Ctrl Pts',(212.945992375754,0.998029054330063,-4.90947942114053));
#36989=CARTESIAN_POINT('Ctrl Pts',(212.919595852068,0.158254085390298,-5.00739511366405));
#36990=CARTESIAN_POINT('Ctrl Pts',(212.893199328382,-0.653975725517873,
-4.89896849687425));
#36991=CARTESIAN_POINT('Ctrl Pts',(212.866802804696,-1.46620553642604,-4.79054188008444));
#36992=CARTESIAN_POINT('Ctrl Pts',(212.84040628101,-2.25089018930262,-4.47577295398131));
#36993=CARTESIAN_POINT('Ctrl Pts',(212.814009757324,-2.91288544151243,-3.99282794364569));
#36994=CARTESIAN_POINT('Ctrl Pts',(212.787613233638,-3.57488069372224,-3.50988293331007));
#36995=CARTESIAN_POINT('Ctrl Pts',(212.761216709953,-4.1141865452653,-2.85876183874197));
#36996=CARTESIAN_POINT('Ctrl Pts',(212.734820186267,-4.46541131732428,-2.11841411202937));
#36997=CARTESIAN_POINT('Ctrl Pts',(212.71132027573,-4.77809456379463,-1.45930818009766));
#36998=CARTESIAN_POINT('Ctrl Pts',(212.687820365194,-4.94170993718427,-0.729483681936857));
#36999=CARTESIAN_POINT('Ctrl Pts',(212.664320454657,-4.94229966671163,8.50863313224884E-5));
#37000=CARTESIAN_POINT('Ctrl Pts',(212.519679545343,-4.94226196377334,9.54014550954459E-5));
#37001=CARTESIAN_POINT('Ctrl Pts',(212.542710501349,-4.94163316922262,-0.714930190902053));
#37002=CARTESIAN_POINT('Ctrl Pts',(212.565741457354,-4.78468413781976,-1.4302228366333));
#37003=CARTESIAN_POINT('Ctrl Pts',(212.588772413359,-4.48396252385269,-2.07885948440059));
#37004=CARTESIAN_POINT('Ctrl Pts',(212.615168937045,-4.1392957543079,-2.82228292857908));
#37005=CARTESIAN_POINT('Ctrl Pts',(212.641565460731,-3.6057665369567,-3.4781457634124));
#37006=CARTESIAN_POINT('Ctrl Pts',(212.667961984417,-2.94806612467695,-3.96692359338189));
#37007=CARTESIAN_POINT('Ctrl Pts',(212.694358508103,-2.29036571239719,-4.45570142335139));
#37008=CARTESIAN_POINT('Ctrl Pts',(212.720755031789,-1.50849410518888,-4.77739424845707));
#37009=CARTESIAN_POINT('Ctrl Pts',(212.747151555475,-0.697254459495896,
-4.89299631002423));
#37010=CARTESIAN_POINT('Ctrl Pts',(212.77354807916,0.113985186197088,-5.00859837159139));
#37011=CARTESIAN_POINT('Ctrl Pts',(212.799944602846,0.954592870374744,-4.91810966962003));
#37012=CARTESIAN_POINT('Ctrl Pts',(212.826341126532,1.72264359530558,-4.63250210089001));
#37013=CARTESIAN_POINT('Ctrl Pts',(212.852737650218,2.4906943202364,-4.34689453215999));
#37014=CARTESIAN_POINT('Ctrl Pts',(212.879134173904,3.18618808592041,-3.86616809667132));
#37015=CARTESIAN_POINT('Ctrl Pts',(212.90553069759,3.72479518442856,-3.2486116273349));
#37016=CARTESIAN_POINT('Ctrl Pts',(212.931927221275,4.26340228293672,-2.63105515799846));
#37017=CARTESIAN_POINT('Ctrl Pts',(212.958323744961,4.645122714269,-1.87666865481429));
#37018=CARTESIAN_POINT('Ctrl Pts',(212.984720268647,4.82367227851871,-1.07692266233362));
#37019=CARTESIAN_POINT('Ctrl Pts',(213.011116792333,5.00222184276842,-0.277176669852958));
#37020=CARTESIAN_POINT('Ctrl Pts',(213.037513316019,4.97760053993555,0.567928811924184));
#37021=CARTESIAN_POINT('Ctrl Pts',(213.063909839705,4.7527937415348,1.35592342026579));
#37022=CARTESIAN_POINT('Ctrl Pts',(213.090306363391,4.52798694313405,2.1439180286074));
#37023=CARTESIAN_POINT('Ctrl Pts',(213.116702887077,4.10299464916542,2.87480176351348));
#37024=CARTESIAN_POINT('Ctrl Pts',(213.143099410762,3.52934784062516,3.45995382788155));
#37025=CARTESIAN_POINT('Ctrl Pts',(213.169495934448,2.95570103208489,4.04510589224962));
#37026=CARTESIAN_POINT('Ctrl Pts',(213.195892458134,2.23339970897298,4.48452628607969));
#37027=CARTESIAN_POINT('Ctrl Pts',(213.22228898182,1.45002403752555,4.7249345986792));
#37028=CARTESIAN_POINT('Ctrl Pts',(213.248685505506,0.666648366078123,4.96534291127871));
#37029=CARTESIAN_POINT('Ctrl Pts',(213.275082029192,-0.177801653704833,
5.00673914264765));
#37030=CARTESIAN_POINT('Ctrl Pts',(213.301478552878,-0.980935134884255,
4.84410393492411));
#37031=CARTESIAN_POINT('Ctrl Pts',(213.327875076563,-1.78406861606368,4.68146872720057));
#37032=CARTESIAN_POINT('Ctrl Pts',(213.354271600249,-2.54588555863957,4.31480208038455));
#37033=CARTESIAN_POINT('Ctrl Pts',(213.380668123935,-3.17401446565158,3.78856289944251));
#37034=CARTESIAN_POINT('Ctrl Pts',(213.407064647621,-3.80214337266358,3.26232371850047));
#37035=CARTESIAN_POINT('Ctrl Pts',(213.433461171307,-4.2965842441117,2.57651200343242));
#37036=CARTESIAN_POINT('Ctrl Pts',(213.459857694993,-4.59738535025415,1.81428349837234));
#37037=CARTESIAN_POINT('Ctrl Pts',(213.479798311776,-4.82461828656924,1.238476369306));
#37038=CARTESIAN_POINT('Ctrl Pts',(213.49973892856,-4.94134715880491,0.619060605181198));
#37039=CARTESIAN_POINT('Ctrl Pts',(213.519679545343,-4.94197050942031,-0.000126753746856371));
#37040=CARTESIAN_POINT('Origin',(215.7,0.,0.));
#37041=CARTESIAN_POINT('',(214.664320454657,-4.94170537201422,9.14365381503302E-5));
#37042=CARTESIAN_POINT('',(214.519679545343,-4.9416771233585,8.15223711883949E-5));
#37043=CARTESIAN_POINT('',(215.7,-4.942,-6.05220448138622E-16));
#37044=CARTESIAN_POINT('Ctrl Pts',(214.664320454657,-4.94170537201422,9.14365381503302E-5));
#37045=CARTESIAN_POINT('Ctrl Pts',(214.654670266987,-4.94190534123349,0.299791017841205));
#37046=CARTESIAN_POINT('Ctrl Pts',(214.645020079318,-4.91507622987908,0.59945521995453));
#37047=CARTESIAN_POINT('Ctrl Pts',(214.635369891648,-4.86088328872289,0.894086257778003));
#37048=CARTESIAN_POINT('Ctrl Pts',(214.608973367962,-4.71264728505111,1.70000169017262));
#37049=CARTESIAN_POINT('Ctrl Pts',(214.582576844276,-4.35967310358994,2.4682586188898));
#37050=CARTESIAN_POINT('Ctrl Pts',(214.55618032059,-3.84475941644516,3.10570468856735));
#37051=CARTESIAN_POINT('Ctrl Pts',(214.529783796904,-3.32984572930037,3.74315075824491));
#37052=CARTESIAN_POINT('Ctrl Pts',(214.503387273219,-2.65299253647195,4.24978596888284));
#37053=CARTESIAN_POINT('Ctrl Pts',(214.476990749533,-1.8962693472472,4.56418000802155));
#37054=CARTESIAN_POINT('Ctrl Pts',(214.450594225847,-1.13954615802247,4.87857404716025));
#37055=CARTESIAN_POINT('Ctrl Pts',(214.424197702161,-0.302952972401405,
5.00072691479974));
#37056=CARTESIAN_POINT('Ctrl Pts',(214.397801178475,0.512071976119432,4.91582738450061));
#37057=CARTESIAN_POINT('Ctrl Pts',(214.371404654789,1.32709692464027,4.83092785420148));
#37058=CARTESIAN_POINT('Ctrl Pts',(214.345008131104,2.12055363606088,4.53897592596373));
#37059=CARTESIAN_POINT('Ctrl Pts',(214.318611607418,2.79623424191442,4.07537122815557));
#37060=CARTESIAN_POINT('Ctrl Pts',(214.292215083732,3.47191484776796,3.61176653034741));
#37061=CARTESIAN_POINT('Ctrl Pts',(214.265818560046,4.02981934805443,2.97650906296882));
#37062=CARTESIAN_POINT('Ctrl Pts',(214.23942203636,4.40230094867901,2.24662478847556));
#37063=CARTESIAN_POINT('Ctrl Pts',(214.213025512674,4.77478254930359,1.5167405139823));
#37064=CARTESIAN_POINT('Ctrl Pts',(214.186628988988,4.96184125026628,0.692229432374359));
#37065=CARTESIAN_POINT('Ctrl Pts',(214.160232465303,4.94079589122303,-0.126935196878605));
#37066=CARTESIAN_POINT('Ctrl Pts',(214.133835941617,4.91975053217978,-0.946099826131545));
#37067=CARTESIAN_POINT('Ctrl Pts',(214.107439417931,4.69060111313059,-1.75991800302951));
#37068=CARTESIAN_POINT('Ctrl Pts',(214.081042894245,4.28113235988322,-2.46971299953935));
#37069=CARTESIAN_POINT('Ctrl Pts',(214.054646370559,3.87166360663584,-3.17950799604922));
#37070=CARTESIAN_POINT('Ctrl Pts',(214.028249846873,3.28187551919026,-3.78527981217096));
#37071=CARTESIAN_POINT('Ctrl Pts',(214.001853323188,2.58328082650013,-4.2135776668254));
#37072=CARTESIAN_POINT('Ctrl Pts',(213.975456799502,1.88468613381001,-4.64187552147983));
#37073=CARTESIAN_POINT('Ctrl Pts',(213.949060275816,1.07728483587533,-4.89269941466696));
#37074=CARTESIAN_POINT('Ctrl Pts',(213.92266375213,0.258975604108923,-4.93563655665704));
#37075=CARTESIAN_POINT('Ctrl Pts',(213.896267228444,-0.559333627657485,
-4.97857369864712));
#37076=CARTESIAN_POINT('Ctrl Pts',(213.869870704758,-1.38855079325563,-4.81362408944015));
#37077=CARTESIAN_POINT('Ctrl Pts',(213.843474181072,-2.12813201316436,-4.46078812739161));
#37078=CARTESIAN_POINT('Ctrl Pts',(213.817077657387,-2.86771323307308,-4.10795216534308));
#37079=CARTESIAN_POINT('Ctrl Pts',(213.790681133701,-3.51765850729239,-3.56722985045298));
#37080=CARTESIAN_POINT('Ctrl Pts',(213.764284610015,-3.99916095379242,-2.90418460993702));
#37081=CARTESIAN_POINT('Ctrl Pts',(213.737888086329,-4.48066340029245,-2.24113936942106));
#37082=CARTESIAN_POINT('Ctrl Pts',(213.711491562643,-4.7937230190732,-1.45577120327923));
#37083=CARTESIAN_POINT('Ctrl Pts',(213.685095038957,-4.9003808412427,-0.643307231200192));
#37084=CARTESIAN_POINT('Ctrl Pts',(213.678170177524,-4.92836144384437,-0.430165512491651));
#37085=CARTESIAN_POINT('Ctrl Pts',(213.67124531609,-4.94213701574224,-0.215159000154365));
#37086=CARTESIAN_POINT('Ctrl Pts',(213.664320454657,-4.94192591391644,-0.000125637169695325));
#37087=CARTESIAN_POINT('Ctrl Pts',(213.519679545343,-4.94197050942031,-0.000126753746856371));
#37088=CARTESIAN_POINT('Ctrl Pts',(213.526135452245,-4.94217232331525,-0.200592766796161));
#37089=CARTESIAN_POINT('Ctrl Pts',(213.532591359148,-4.93020414732645,-0.401034838788269));
#37090=CARTESIAN_POINT('Ctrl Pts',(213.53904726605,-4.90587589242006,-0.599965331806195));
#37091=CARTESIAN_POINT('Ctrl Pts',(213.565443789736,-4.80640398760677,-1.41334036187257));
#37092=CARTESIAN_POINT('Ctrl Pts',(213.591840313422,-4.50029883714341,-2.20144512695319));
#37093=CARTESIAN_POINT('Ctrl Pts',(213.618236837108,-4.02467616975082,-2.86872069045377));
#37094=CARTESIAN_POINT('Ctrl Pts',(213.644633360794,-3.54905350235822,-3.53599625395434));
#37095=CARTESIAN_POINT('Ctrl Pts',(213.671029884479,-2.90391331803639,-4.08244261587486));
#37096=CARTESIAN_POINT('Ctrl Pts',(213.697426408165,-2.16747987414245,-4.44180229933583));
#37097=CARTESIAN_POINT('Ctrl Pts',(213.723822931851,-1.43104643024851,-4.8011619827968));
#37098=CARTESIAN_POINT('Ctrl Pts',(213.750219455537,-0.603319726782466,
-4.97343498779822));
#37099=CARTESIAN_POINT('Ctrl Pts',(213.776615979223,0.215337077601472,-4.93773294277928));
#37100=CARTESIAN_POINT('Ctrl Pts',(213.803012502909,1.03399388198541,-4.90203089776034));
#37101=CARTESIAN_POINT('Ctrl Pts',(213.829409026594,1.84358078728724,-4.65835380272105));
#37102=CARTESIAN_POINT('Ctrl Pts',(213.85580555028,2.54593411377918,-4.23624788692696));
#37103=CARTESIAN_POINT('Ctrl Pts',(213.882202073966,3.24828744027111,-3.81414197113286));
#37104=CARTESIAN_POINT('Ctrl Pts',(213.908598597652,3.84340718795315,-3.21360723458397));
#37105=CARTESIAN_POINT('Ctrl Pts',(213.934995121338,4.25913415572091,-2.50745945426226));
#37106=CARTESIAN_POINT('Ctrl Pts',(213.961391645024,4.67486112348867,-1.80131167394057));
#37107=CARTESIAN_POINT('Ctrl Pts',(213.98778816871,4.91119531134216,-0.989550849846085));
#37108=CARTESIAN_POINT('Ctrl Pts',(214.014184692395,4.93948082900791,-0.170604252763584));
#37109=CARTESIAN_POINT('Ctrl Pts',(214.040581216081,4.96776634667366,0.648342344318934));
#37110=CARTESIAN_POINT('Ctrl Pts',(214.066977739767,4.78800319415165,1.47447471438945));
#37111=CARTESIAN_POINT('Ctrl Pts',(214.093374263453,4.42198793511587,2.207623014214));
#37112=CARTESIAN_POINT('Ctrl Pts',(214.119770787139,4.05597267608009,2.94077131403855));
#37113=CARTESIAN_POINT('Ctrl Pts',(214.146167310825,3.50370531053053,3.58093554361713));
#37114=CARTESIAN_POINT('Ctrl Pts',(214.172563834511,2.83214912114986,4.05049478789539));
#37115=CARTESIAN_POINT('Ctrl Pts',(214.198960358196,2.1605929317692,4.52005403217365));
#37116=CARTESIAN_POINT('Ctrl Pts',(214.225356881882,1.36974791855743,4.8190082911516));
#37117=CARTESIAN_POINT('Ctrl Pts',(214.251753405568,0.555505277484793,4.91110889289621));
#37118=CARTESIAN_POINT('Ctrl Pts',(214.278149929254,-0.258737363587817,
5.0032094946408));
#37119=CARTESIAN_POINT('Ctrl Pts',(214.30454645294,-1.09637763252129,4.88845643915207));
#37120=CARTESIAN_POINT('Ctrl Pts',(214.330942976626,-1.85585033532817,4.58076371406123));
#37121=CARTESIAN_POINT('Ctrl Pts',(214.357339500311,-2.61532303813507,4.27307098897037));
#37122=CARTESIAN_POINT('Ctrl Pts',(214.383736023997,-3.29662817481538,3.77243859427741));
#37123=CARTESIAN_POINT('Ctrl Pts',(214.410132547683,-3.81715643091995,3.13956899161081));
#37124=CARTESIAN_POINT('Ctrl Pts',(214.436529071369,-4.33768468702453,2.5066993889442));
#37125=CARTESIAN_POINT('Ctrl Pts',(214.462925595055,-4.69743606255337,1.74159257830395));
#37126=CARTESIAN_POINT('Ctrl Pts',(214.489322118741,-4.85279014000988,0.937018958303713));
#37127=CARTESIAN_POINT('Ctrl Pts',(214.499441260941,-4.91234533068453,0.628584598965291));
#37128=CARTESIAN_POINT('Ctrl Pts',(214.509560403142,-4.94186265527411,0.314350266997381));
#37129=CARTESIAN_POINT('Ctrl Pts',(214.519679545343,-4.9416771233585,8.15223711883949E-5));
#37130=CARTESIAN_POINT('Origin',(215.7,0.,0.));
#37131=CARTESIAN_POINT('',(215.664320454657,-4.9424258920011,-5.59704580684751E-6));
#37132=CARTESIAN_POINT('',(215.519679545343,-4.94242455630813,9.71285613910342E-6));
#37133=CARTESIAN_POINT('',(215.7,-4.942,-6.05220448138622E-16));
#37134=CARTESIAN_POINT('Ctrl Pts',(215.664320454657,-4.94242563693782,-5.5936937812251E-6));
#37135=CARTESIAN_POINT('Ctrl Pts',(215.638095217884,-4.94237108343367,0.814112285436369));
#37136=CARTESIAN_POINT('Ctrl Pts',(215.611869981111,-4.7369973879704,1.62825668193243));
#37137=CARTESIAN_POINT('Ctrl Pts',(215.585644744339,-4.3507429111603,2.3449120887405));
#37138=CARTESIAN_POINT('Ctrl Pts',(215.559248220653,-3.96196566067396,3.06624824231987));
#37139=CARTESIAN_POINT('Ctrl Pts',(215.532851696967,-3.38993711145197,3.68881777271392));
#37140=CARTESIAN_POINT('Ctrl Pts',(215.506455173281,-2.70401662063462,4.1371331496901));
#37141=CARTESIAN_POINT('Ctrl Pts',(215.480058649595,-2.01809612981727,4.58544852666628));
#37142=CARTESIAN_POINT('Ctrl Pts',(215.453662125909,-1.21828369740459,4.85950975022456));
#37143=CARTESIAN_POINT('Ctrl Pts',(215.427265602223,-0.401557832984007,
4.92608646794818));
#37144=CARTESIAN_POINT('Ctrl Pts',(215.400869078538,0.41516803143658,4.9926631856718));
#37145=CARTESIAN_POINT('Ctrl Pts',(215.374472554852,1.24880732786508,4.85175539756075));
#37146=CARTESIAN_POINT('Ctrl Pts',(215.348076031166,1.99827998649403,4.52044839352363));
#37147=CARTESIAN_POINT('Ctrl Pts',(215.32167950748,2.74775264512299,4.18914138948651));
#37148=CARTESIAN_POINT('Ctrl Pts',(215.295282983794,3.4130586659524,3.66743516952332));
#37149=CARTESIAN_POINT('Ctrl Pts',(215.268886460108,3.91352865237769,3.01858742956897));
#37150=CARTESIAN_POINT('Ctrl Pts',(215.242489936422,4.41399863880298,2.36973968961461));
#37151=CARTESIAN_POINT('Ctrl Pts',(215.216093412737,4.74963259082415,1.59375042966909));
#37152=CARTESIAN_POINT('Ctrl Pts',(215.189696889051,4.87973436630227,0.784709562361485));
#37153=CARTESIAN_POINT('Ctrl Pts',(215.163300365365,5.00983614178038,-0.0243313049461004));
#37154=CARTESIAN_POINT('Ctrl Pts',(215.136903841679,4.93440574071546,-0.86642377961577));
#37155=CARTESIAN_POINT('Ctrl Pts',(215.110507317993,4.66258921732772,-1.63946283074435));
#37156=CARTESIAN_POINT('Ctrl Pts',(215.084110794307,4.39077269393997,-2.41250188187294));
#37157=CARTESIAN_POINT('Ctrl Pts',(215.057714270621,3.9225700482294,-3.11648750946044));
#37158=CARTESIAN_POINT('Ctrl Pts',(215.031317746936,3.31475158398952,-3.66606035402746));
#37159=CARTESIAN_POINT('Ctrl Pts',(215.00492122325,2.70693311974964,-4.21563319859447));
#37160=CARTESIAN_POINT('Ctrl Pts',(214.978524699564,1.95949883698045,-4.610793260141));
#37161=CARTESIAN_POINT('Ctrl Pts',(214.952128175878,1.16307631262376,-4.80362676255623));
#37162=CARTESIAN_POINT('Ctrl Pts',(214.925731652192,0.366653788267074,-4.99646026497147));
#37163=CARTESIAN_POINT('Ctrl Pts',(214.899335128506,-0.478756977677111,
-4.98696720825542));
#37164=CARTESIAN_POINT('Ctrl Pts',(214.872938604821,-1.27064860629358,-4.77629864039689));
#37165=CARTESIAN_POINT('Ctrl Pts',(214.846542081135,-2.06254023491004,-4.56563007253835));
#37166=CARTESIAN_POINT('Ctrl Pts',(214.820145557449,-2.80091272619879,-4.15378599353734));
#37167=CARTESIAN_POINT('Ctrl Pts',(214.793749033763,-3.39623725962183,-3.5907031427409));
#37168=CARTESIAN_POINT('Ctrl Pts',(214.767352510077,-3.99156179304486,-3.02762029194445));
#37169=CARTESIAN_POINT('Ctrl Pts',(214.740955986391,-4.44383836860219,-2.31329866935258));
#37170=CARTESIAN_POINT('Ctrl Pts',(214.714559462706,-4.69822774343964,-1.5343508900206));
#37171=CARTESIAN_POINT('Ctrl Pts',(214.697813126689,-4.85961603837852,-1.04017516419425));
#37172=CARTESIAN_POINT('Ctrl Pts',(214.681066790673,-4.94135835785724,-0.519988593426523));
#37173=CARTESIAN_POINT('Ctrl Pts',(214.664320454657,-4.94170537201422,9.14365381503302E-5));
#37174=CARTESIAN_POINT('Ctrl Pts',(214.519679545343,-4.9416771233585,8.15223711883949E-5));
#37175=CARTESIAN_POINT('Ctrl Pts',(214.535956926828,-4.94137868168151,-0.505442774410793));
#37176=CARTESIAN_POINT('Ctrl Pts',(214.552234308313,-4.8642238638634,-1.01105611421827));
#37177=CARTESIAN_POINT('Ctrl Pts',(214.568511689798,-4.71160704544237,-1.49276110631793));
#37178=CARTESIAN_POINT('Ctrl Pts',(214.594908213484,-4.46411309403417,-2.27392712157909));
#37179=CARTESIAN_POINT('Ctrl Pts',(214.62130473717,-4.01816841183361,-2.99221872274118));
#37180=CARTESIAN_POINT('Ctrl Pts',(214.647701260856,-3.42784448971234,-3.56054192863199));
#37181=CARTESIAN_POINT('Ctrl Pts',(214.674097784542,-2.83752056759108,-4.12886513452279));
#37182=CARTESIAN_POINT('Ctrl Pts',(214.700494308228,-2.10281740554911,-4.54721994514231));
#37183=CARTESIAN_POINT('Ctrl Pts',(214.726890831913,-1.31281891220868,-4.76488018474178));
#37184=CARTESIAN_POINT('Ctrl Pts',(214.753287355599,-0.52282041886825,-4.98254042434126));
#37185=CARTESIAN_POINT('Ctrl Pts',(214.779683879285,0.322473405770636,-4.99950609292068));
#37186=CARTESIAN_POINT('Ctrl Pts',(214.806080402971,1.12056936210911,-4.81372007660396));
#37187=CARTESIAN_POINT('Ctrl Pts',(214.832476926657,1.91866531844758,-4.62793406028724));
#37188=CARTESIAN_POINT('Ctrl Pts',(214.858873450343,2.66956340648564,-4.23939635907438));
#37189=CARTESIAN_POINT('Ctrl Pts',(214.885269974028,3.28221605746981,-3.69521777751799));
#37190=CARTESIAN_POINT('Ctrl Pts',(214.911666497714,3.89486870845398,-3.15103919596161));
#37191=CARTESIAN_POINT('Ctrl Pts',(214.9380630214,4.36927592238426,-2.45121973406169));
#37192=CARTESIAN_POINT('Ctrl Pts',(214.964459545086,4.64791508185686,-1.68061359718562));
#37193=CARTESIAN_POINT('Ctrl Pts',(214.990856068772,4.92655424132946,-0.910007460309548));
#37194=CARTESIAN_POINT('Ctrl Pts',(215.017252592458,5.00942534634437,-0.0686146484573258));
#37195=CARTESIAN_POINT('Ctrl Pts',(215.043649116144,4.88648014567853,0.741544642679851));
#37196=CARTESIAN_POINT('Ctrl Pts',(215.070045639829,4.7635349450127,1.55170393381702));
#37197=CARTESIAN_POINT('Ctrl Pts',(215.096442163515,4.43477343866612,2.33062970423914));
#37198=CARTESIAN_POINT('Ctrl Pts',(215.122838687201,3.94005847398043,2.98387598482455));
#37199=CARTESIAN_POINT('Ctrl Pts',(215.149235210887,3.44534350929474,3.63712226540996));
#37200=CARTESIAN_POINT('Ctrl Pts',(215.175631734573,2.78467508626995,4.16468905615867));
#37201=CARTESIAN_POINT('Ctrl Pts',(215.202028258259,2.03816028551635,4.50260805775292));
#37202=CARTESIAN_POINT('Ctrl Pts',(215.228424781945,1.29164548476275,4.84052705934719));
#37203=CARTESIAN_POINT('Ctrl Pts',(215.25482130563,0.459284306280347,4.98879827178699));
#37204=CARTESIAN_POINT('Ctrl Pts',(215.281217829316,-0.357998153925342,
4.92944357843598));
#37205=CARTESIAN_POINT('Ctrl Pts',(215.307614353002,-1.17528061413103,4.87008888508496));
#37206=CARTESIAN_POINT('Ctrl Pts',(215.334010876688,-1.97748435606,4.60310828594313));
#37207=CARTESIAN_POINT('Ctrl Pts',(215.360407400374,-2.66734092010225,4.16087359663157));
#37208=CARTESIAN_POINT('Ctrl Pts',(215.38680392406,-3.35719748414449,3.71863890732002));
#37209=CARTESIAN_POINT('Ctrl Pts',(215.413200447745,-3.9347068703,3.10115012783875));
#37210=CARTESIAN_POINT('Ctrl Pts',(215.439596971431,-4.32984516136964,2.38327873941794));
#37211=CARTESIAN_POINT('Ctrl Pts',(215.465993495117,-4.72498345243928,1.66540735099713));
#37212=CARTESIAN_POINT('Ctrl Pts',(215.492390018803,-4.93775064842305,0.847153353636784));
#37213=CARTESIAN_POINT('Ctrl Pts',(215.518786542489,-4.9423483937073,0.0277313255456686));
#37214=CARTESIAN_POINT('Ctrl Pts',(215.519084210107,-4.94240024143936,0.0184908889552883));
#37215=CARTESIAN_POINT('Ctrl Pts',(215.519381877725,-4.94242561717416,0.0092503038315561));
#37216=CARTESIAN_POINT('Ctrl Pts',(215.519679545343,-4.94242455630813,9.71285613910342E-6));
#37217=CARTESIAN_POINT('Origin',(215.7,0.,0.));
#37218=CARTESIAN_POINT('',(216.664320454657,-4.94168438867978,-8.42883428375796E-5));
#37219=CARTESIAN_POINT('',(216.519679545343,-4.94171357522401,-9.3938055576132E-5));
#37220=CARTESIAN_POINT('',(215.7,-4.942,-6.05220448138622E-16));
#37221=CARTESIAN_POINT('Ctrl Pts',(216.664320454657,-4.94168438867978,-8.42883428375796E-5));
#37222=CARTESIAN_POINT('Ctrl Pts',(216.647916692467,-4.94137282101751,0.509362846945846));
#37223=CARTESIAN_POINT('Ctrl Pts',(216.631512930277,-4.86299534936484,1.018903668412));
#37224=CARTESIAN_POINT('Ctrl Pts',(216.615109168087,-4.70803758557245,1.50398094262197));
#37225=CARTESIAN_POINT('Ctrl Pts',(216.588712644401,-4.45868342919959,2.28455515540122));
#37226=CARTESIAN_POINT('Ctrl Pts',(216.562316120715,-4.01102888604924,3.00178237971507));
#37227=CARTESIAN_POINT('Ctrl Pts',(216.535919597029,-3.41935277031013,3.56869769175051));
#37228=CARTESIAN_POINT('Ctrl Pts',(216.509523073343,-2.82767665457099,4.13561300378596));
#37229=CARTESIAN_POINT('Ctrl Pts',(216.483126549657,-2.09197896624308,4.55221640354299));
#37230=CARTESIAN_POINT('Ctrl Pts',(216.456730025972,-1.30146420181781,4.76799407658186));
#37231=CARTESIAN_POINT('Ctrl Pts',(216.430333502286,-0.510949437392535,
4.98377174962073));
#37232=CARTESIAN_POINT('Ctrl Pts',(216.4039369786,0.33438240313007,4.99872369594143));
#37233=CARTESIAN_POINT('Ctrl Pts',(216.377540454914,1.13203351066578,4.81103696864436));
#37234=CARTESIAN_POINT('Ctrl Pts',(216.351143931228,1.92968461820145,4.62335024134729));
#37235=CARTESIAN_POINT('Ctrl Pts',(216.324747407542,2.67965499275022,4.23302484043244));
#37236=CARTESIAN_POINT('Ctrl Pts',(216.298350883857,3.29100955227154,3.68738833184009));
#37237=CARTESIAN_POINT('Ctrl Pts',(216.271954360171,3.90236411179289,3.14175182324771));
#37238=CARTESIAN_POINT('Ctrl Pts',(216.245557836485,4.37510285628678,2.44080420697781));
#37239=CARTESIAN_POINT('Ctrl Pts',(216.219161312799,4.65190547288072,1.66953647888129));
#37240=CARTESIAN_POINT('Ctrl Pts',(216.192764789113,4.92870808947466,0.898268750784777));
#37241=CARTESIAN_POINT('Ctrl Pts',(216.166368265427,5.00957457816861,0.0566809108616259));
#37242=CARTESIAN_POINT('Ctrl Pts',(216.139971741741,4.8846997506068,-0.753183197737967));
#37243=CARTESIAN_POINT('Ctrl Pts',(216.113575218056,4.75982492304499,-1.56304730633755));
#37244=CARTESIAN_POINT('Ctrl Pts',(216.08717869437,4.42920877922744,-2.34118768361358));
#37245=CARTESIAN_POINT('Ctrl Pts',(216.060782170684,3.93293904419266,-2.993253590593));
#37246=CARTESIAN_POINT('Ctrl Pts',(216.034385646998,3.43666930915788,-3.64531949757242));
#37247=CARTESIAN_POINT('Ctrl Pts',(216.007989123312,2.77474598290587,-4.17131093425521));
#37248=CARTESIAN_POINT('Ctrl Pts',(215.981592599626,2.02742830502788,-4.50745061547042));
#37249=CARTESIAN_POINT('Ctrl Pts',(215.95519607594,1.2801106271499,-4.84359029668564));
#37250=CARTESIAN_POINT('Ctrl Pts',(215.928799552255,0.447398597645939,-4.98987822243327));
#37251=CARTESIAN_POINT('Ctrl Pts',(215.902403028569,-0.369740146242837,
-4.92857675269335));
#37252=CARTESIAN_POINT('Ctrl Pts',(215.876006504883,-1.18687889013161,-4.86727528295342));
#37253=CARTESIAN_POINT('Ctrl Pts',(215.849609981197,-1.98844434840521,-4.59838441772594));
#37254=CARTESIAN_POINT('Ctrl Pts',(215.823213457511,-2.6772454543461,-4.15450759538554));
#37255=CARTESIAN_POINT('Ctrl Pts',(215.796816933825,-3.36604656028698,-3.71063077304514));
#37256=CARTESIAN_POINT('Ctrl Pts',(215.770420410139,-3.94208331389515,-3.09176799359182));
#37257=CARTESIAN_POINT('Ctrl Pts',(215.744023886454,-4.33551035697334,-2.37295733790345));
#37258=CARTESIAN_POINT('Ctrl Pts',(215.717627362768,-4.72893740005153,-1.65414668221509));
#37259=CARTESIAN_POINT('Ctrl Pts',(215.691230839082,-4.93975473259975,-0.835388150291677));
#37260=CARTESIAN_POINT('Ctrl Pts',(215.664834315396,-4.94240042299853,-0.0159574959476391));
#37261=CARTESIAN_POINT('Ctrl Pts',(215.664663028483,-4.94241759087058,-0.0106402144408186));
#37262=CARTESIAN_POINT('Ctrl Pts',(215.66449174157,-4.94242599324733,-0.00532290463290051));
#37263=CARTESIAN_POINT('Ctrl Pts',(215.664320454657,-4.94242563693782,-5.5936937812251E-6));
#37264=CARTESIAN_POINT('Ctrl Pts',(215.519679545343,-4.94242455630813,9.71285613910342E-6));
#37265=CARTESIAN_POINT('Ctrl Pts',(215.545778401411,-4.94233154185726,-0.810185414792319));
#37266=CARTESIAN_POINT('Ctrl Pts',(215.571877257479,-4.73900967080375,-1.62042552671124));
#37267=CARTESIAN_POINT('Ctrl Pts',(215.597976113546,-4.3563166654476,-2.33454102160172));
#37268=CARTESIAN_POINT('Ctrl Pts',(215.624372637232,-3.96925889731891,-3.05680128183612));
#37269=CARTESIAN_POINT('Ctrl Pts',(215.650769160918,-3.3987150664768,-3.68073174348307));
#37270=CARTESIAN_POINT('Ctrl Pts',(215.677165684604,-2.71386450563363,-4.13067986126492));
#37271=CARTESIAN_POINT('Ctrl Pts',(215.70356220829,-2.02901394479045,-4.58062797904678));
#37272=CARTESIAN_POINT('Ctrl Pts',(215.729958731976,-1.22985665394621,-4.85659375296355));
#37273=CARTESIAN_POINT('Ctrl Pts',(215.756355255662,-0.413291705747491,
-4.92511590088579));
#37274=CARTESIAN_POINT('Ctrl Pts',(215.782751779347,0.40327324245123,-4.99363804880802));
#37275=CARTESIAN_POINT('Ctrl Pts',(215.809148303033,1.23724584800443,-4.85471657073573));
#37276=CARTESIAN_POINT('Ctrl Pts',(215.835544826719,1.98750562685147,-4.52519591337562));
#37277=CARTESIAN_POINT('Ctrl Pts',(215.861941350405,2.73776540569852,-4.1956752560155));
#37278=CARTESIAN_POINT('Ctrl Pts',(215.888337874091,3.4043123578394,-3.67555541936756));
#37279=CARTESIAN_POINT('Ctrl Pts',(215.914734397777,3.90632662180527,-3.02790174790614));
#37280=CARTESIAN_POINT('Ctrl Pts',(215.941130921462,4.40834088577113,-2.38024807644474));
#37281=CARTESIAN_POINT('Ctrl Pts',(215.967527445148,4.74582246156199,-1.60506057016986));
#37282=CARTESIAN_POINT('Ctrl Pts',(215.993923968834,4.87785117976427,-0.796331927822826));
#37283=CARTESIAN_POINT('Ctrl Pts',(216.02032049252,5.00987989796655,0.0123967145242333));
#37284=CARTESIAN_POINT('Ctrl Pts',(216.046717016206,4.93645575858024,0.854666492943454));
#37285=CARTESIAN_POINT('Ctrl Pts',(216.073113539892,4.66648155345611,1.62835087817444));
#37286=CARTESIAN_POINT('Ctrl Pts',(216.099510063578,4.39650734833198,2.40203526340543));
#37287=CARTESIAN_POINT('Ctrl Pts',(216.125906587263,3.92998307747003,3.10713425544818));
#37288=CARTESIAN_POINT('Ctrl Pts',(216.152303110949,3.32347553908577,3.65815349764006));
#37289=CARTESIAN_POINT('Ctrl Pts',(216.178699634635,2.71696800070151,4.20917273983195));
#37290=CARTESIAN_POINT('Ctrl Pts',(216.205096158321,1.97047719479494,4.60611223217296));
#37291=CARTESIAN_POINT('Ctrl Pts',(216.231492682007,1.1745163002612,4.80084243978267));
#37292=CARTESIAN_POINT('Ctrl Pts',(216.257889205693,0.378555405727472,4.99557264739237));
#37293=CARTESIAN_POINT('Ctrl Pts',(216.284285729378,-0.46687557743342,4.98809357027076));
#37294=CARTESIAN_POINT('Ctrl Pts',(216.310682253064,-1.25926681893708,4.77931205822781));
#37295=CARTESIAN_POINT('Ctrl Pts',(216.33707877675,-2.05165806044073,4.57053054618486));
#37296=CARTESIAN_POINT('Ctrl Pts',(216.363475300436,-2.79100956028715,4.16044659922057));
#37297=CARTESIAN_POINT('Ctrl Pts',(216.389871824122,-3.38767379161803,3.59878353791694));
#37298=CARTESIAN_POINT('Ctrl Pts',(216.416268347808,-3.98433802294891,3.03712047661331));
#37299=CARTESIAN_POINT('Ctrl Pts',(216.442664871494,-4.43831498576424,2.32387830097037));
#37300=CARTESIAN_POINT('Ctrl Pts',(216.469061395179,-4.69455926259279,1.54553874141088));
#37301=CARTESIAN_POINT('Ctrl Pts',(216.485934111901,-4.85835117496055,1.04802236169082));
#37302=CARTESIAN_POINT('Ctrl Pts',(216.502806828622,-4.9413535679609,0.523908526256979));
#37303=CARTESIAN_POINT('Ctrl Pts',(216.519679545343,-4.94171357522401,-9.3938055576132E-5));
#37304=CARTESIAN_POINT('Origin',(215.7,0.,0.));
#37305=CARTESIAN_POINT('',(217.664320454657,-4.94195837962584,0.000126603499120692));
#37306=CARTESIAN_POINT('',(217.519679545343,-4.94191411506509,0.000125076744195484));
#37307=CARTESIAN_POINT('',(215.7,-4.942,-6.05220448138622E-16));
#37308=CARTESIAN_POINT('Ctrl Pts',(217.664320454657,-4.94195837962584,0.000126603499120692));
#37309=CARTESIAN_POINT('Ctrl Pts',(217.65773816705,-4.94216297129183,0.204518376639697));
#37310=CARTESIAN_POINT('Ctrl Pts',(217.651155879442,-4.92972032171904,0.408885406966804));
#37311=CARTESIAN_POINT('Ctrl Pts',(217.644573591835,-4.90443271504819,0.611650493744549));
#37312=CARTESIAN_POINT('Ctrl Pts',(217.618177068149,-4.80302345610052,1.4247862506487));
#37313=CARTESIAN_POINT('Ctrl Pts',(217.591780544463,-4.4950417374727,2.21215956889818));
#37314=CARTESIAN_POINT('Ctrl Pts',(217.565384020777,-4.01783082471338,2.87830020097209));
#37315=CARTESIAN_POINT('Ctrl Pts',(217.538987497091,-3.54061991195407,3.54444083304598));
#37316=CARTESIAN_POINT('Ctrl Pts',(217.512590973406,-2.89417980506328,4.08934877894429));
#37317=CARTESIAN_POINT('Ctrl Pts',(217.48619444972,-2.15689237904473,4.44695309713873));
#37318=CARTESIAN_POINT('Ctrl Pts',(217.459797926034,-1.41960495302616,4.80455741533317));
#37319=CARTESIAN_POINT('Ctrl Pts',(217.433401402348,-0.59147020787982,4.97485810582372));
#37320=CARTESIAN_POINT('Ctrl Pts',(217.407004878662,0.227099222047519,4.9372059432718));
#37321=CARTESIAN_POINT('Ctrl Pts',(217.380608354976,1.04566865197486,4.89955378071988));
#37322=CARTESIAN_POINT('Ctrl Pts',(217.35421183129,1.8546727666832,4.65394876512549));
#37323=CARTESIAN_POINT('Ctrl Pts',(217.327815307605,2.55601855071661,4.23017088913977));
#37324=CARTESIAN_POINT('Ctrl Pts',(217.301418783919,3.25736433475001,3.80639301315405));
#37325=CARTESIAN_POINT('Ctrl Pts',(217.275022260233,3.85105178810847,3.20444227677701));
#37326=CARTESIAN_POINT('Ctrl Pts',(217.248625736547,4.26509537761672,2.49730614918664));
#37327=CARTESIAN_POINT('Ctrl Pts',(217.222229212861,4.67913896712499,1.79017002159624));
#37328=CARTESIAN_POINT('Ctrl Pts',(217.195832689175,4.91353869278302,0.977848502792508));
#37329=CARTESIAN_POINT('Ctrl Pts',(217.16943616549,4.93987322088706,0.158836848671542));
#37330=CARTESIAN_POINT('Ctrl Pts',(217.143039641804,4.96620774899109,-0.660174805449401));
#37331=CARTESIAN_POINT('Ctrl Pts',(217.116643118118,4.78447707954115,-1.48587659488757));
#37332=CARTESIAN_POINT('Ctrl Pts',(217.090246594432,4.41671634071899,-2.21815088498478));
#37333=CARTESIAN_POINT('Ctrl Pts',(217.063850070746,4.04895560189684,-2.95042517508198));
#37334=CARTESIAN_POINT('Ctrl Pts',(217.03745354706,3.49516479370246,-3.58927196583822));
#37335=CARTESIAN_POINT('Ctrl Pts',(217.011057023374,2.82249191862427,-4.0572300837189));
#37336=CARTESIAN_POINT('Ctrl Pts',(216.984660499689,2.14981904354606,-4.52518820159958));
#37337=CARTESIAN_POINT('Ctrl Pts',(216.958263976003,1.35826410158404,-4.82225764660469));
#37338=CARTESIAN_POINT('Ctrl Pts',(216.931867452317,0.543804368680852,-4.9124182834462));
#37339=CARTESIAN_POINT('Ctrl Pts',(216.905470928631,-0.27065536422234,-5.00257892028772));
#37340=CARTESIAN_POINT('Ctrl Pts',(216.879074404945,-1.1080198880667,-4.88583074896562));
#37341=CARTESIAN_POINT('Ctrl Pts',(216.852677881259,-1.86675744338853,-4.57632966802944));
#37342=CARTESIAN_POINT('Ctrl Pts',(216.826281357573,-2.62549499871034,-4.26682858709326));
#37343=CARTESIAN_POINT('Ctrl Pts',(216.799884833888,-3.30560558550962,-3.764574596543));
#37344=CARTESIAN_POINT('Ctrl Pts',(216.773488310202,-3.82462473038045,-3.13046677904354));
#37345=CARTESIAN_POINT('Ctrl Pts',(216.747091786516,-4.34364387525129,-2.49635896154405));
#37346=CARTESIAN_POINT('Ctrl Pts',(216.72069526283,-4.70157157819368,-1.73039731709535));
#37347=CARTESIAN_POINT('Ctrl Pts',(216.694298739144,-4.85500854486718,-0.925455894248657));
#37348=CARTESIAN_POINT('Ctrl Pts',(216.684305977649,-4.91309418640272,-0.620734418334266));
#37349=CARTESIAN_POINT('Ctrl Pts',(216.674313216153,-4.94187418790405,-0.310426736535013));
#37350=CARTESIAN_POINT('Ctrl Pts',(216.664320454657,-4.94168438867978,-8.42883428375796E-5));
#37351=CARTESIAN_POINT('Ctrl Pts',(216.519679545343,-4.94171357522401,-9.3938055576132E-5));
#37352=CARTESIAN_POINT('Ctrl Pts',(216.529203352308,-4.94191678136659,-0.29586719150049));
#37353=CARTESIAN_POINT('Ctrl Pts',(216.538727159272,-4.91578979804439,-0.591604961667699));
#37354=CARTESIAN_POINT('Ctrl Pts',(216.548250966237,-4.86299941312486,-0.882504039166336));
#37355=CARTESIAN_POINT('Ctrl Pts',(216.574647489923,-4.71668369598663,-1.68877031670807));
#37356=CARTESIAN_POINT('Ctrl Pts',(216.601044013609,-4.3655406708684,-2.45786592831551));
#37357=CARTESIAN_POINT('Ctrl Pts',(216.627440537295,-3.85214697930256,-3.09653682701301));
#37358=CARTESIAN_POINT('Ctrl Pts',(216.65383706098,-3.33875328773674,-3.7352077257105));
#37359=CARTESIAN_POINT('Ctrl Pts',(216.680233584666,-2.66310892972333,-4.24345391149806));
#37360=CARTESIAN_POINT('Ctrl Pts',(216.706630108352,-1.90713684143578,-4.55964973865713));
#37361=CARTESIAN_POINT('Ctrl Pts',(216.733026632038,-1.15116475314824,-4.87584556581619));
#37362=CARTESIAN_POINT('Ctrl Pts',(216.759423155724,-0.314864934586568,
-4.99999103434677));
#37363=CARTESIAN_POINT('Ctrl Pts',(216.78581967941,0.500359951967919,-4.91703331183187));
#37364=CARTESIAN_POINT('Ctrl Pts',(216.812216203095,1.31558483852242,-4.83407558931698));
#37365=CARTESIAN_POINT('Ctrl Pts',(216.838612726781,2.10973479306973,-4.5440146757566));
#37366=CARTESIAN_POINT('Ctrl Pts',(216.865009250467,2.78651789032859,-4.0820209110288));
#37367=CARTESIAN_POINT('Ctrl Pts',(216.891405774153,3.46330098758745,-3.620027146301));
#37368=CARTESIAN_POINT('Ctrl Pts',(216.917802297839,4.02271722755784,-2.98610053040578));
#37369=CARTESIAN_POINT('Ctrl Pts',(216.944198821525,4.39693651534156,-2.25710565797298));
#37370=CARTESIAN_POINT('Ctrl Pts',(216.970595345211,4.77115580312528,-1.52811078554019));
#37371=CARTESIAN_POINT('Ctrl Pts',(216.996991868896,4.96017813872232,-0.704047656569832));
#37372=CARTESIAN_POINT('Ctrl Pts',(217.023388392582,4.94108426801502,0.115164784427049));
#37373=CARTESIAN_POINT('Ctrl Pts',(217.049784916268,4.92199039730772,0.93437722542393));
#37374=CARTESIAN_POINT('Ctrl Pts',(217.076181439954,4.69478032029607,1.74873897844733));
#37375=CARTESIAN_POINT('Ctrl Pts',(217.10257796364,4.28700361452962,2.45950740600789));
#37376=CARTESIAN_POINT('Ctrl Pts',(217.128974487326,3.87922690876317,3.17027583356844));
#37377=CARTESIAN_POINT('Ctrl Pts',(217.155371011012,3.29088357424191,3.77745093566615));
#37378=CARTESIAN_POINT('Ctrl Pts',(217.181767534697,2.59331116136556,4.20741178060033));
#37379=CARTESIAN_POINT('Ctrl Pts',(217.208164058383,1.89573874848922,4.63737262553451));
#37380=CARTESIAN_POINT('Ctrl Pts',(217.234560582069,1.08893725725779,4.89011921330515));
#37381=CARTESIAN_POINT('Ctrl Pts',(217.260957105755,0.27073263158228,4.93500562445416));
#37382=CARTESIAN_POINT('Ctrl Pts',(217.287353629441,-0.54747199409324,4.97989203560317));
#37383=CARTESIAN_POINT('Ctrl Pts',(217.313750153127,-1.37707975421284,4.81691827013054));
#37384=CARTESIAN_POINT('Ctrl Pts',(217.340146676812,-2.11749940905815,4.46584515224566));
#37385=CARTESIAN_POINT('Ctrl Pts',(217.366543200498,-2.85791906390345,4.11477203436078));
#37386=CARTESIAN_POINT('Ctrl Pts',(217.392939724184,-3.50915061347447,3.57559956406364));
#37387=CARTESIAN_POINT('Ctrl Pts',(217.41933624787,-3.99223121284117,2.91370324748667));
#37388=CARTESIAN_POINT('Ctrl Pts',(217.445732771556,-4.47531181220787,2.25180693090971));
#37389=CARTESIAN_POINT('Ctrl Pts',(217.472129295242,-4.79024146137026,1.46718676805292));
#37390=CARTESIAN_POINT('Ctrl Pts',(217.498525818928,-4.89883444732496,0.654979182035602));
#37391=CARTESIAN_POINT('Ctrl Pts',(217.505577061066,-4.92784263975307,0.438016053711726));
#37392=CARTESIAN_POINT('Ctrl Pts',(217.512628303205,-4.94212722614308,0.219084364183518));
#37393=CARTESIAN_POINT('Ctrl Pts',(217.519679545343,-4.94191411506509,0.000125076744195484));
#37394=CARTESIAN_POINT('Origin',(215.7,0.,0.));
#37395=CARTESIAN_POINT('',(218.664320454657,-4.94227242746027,-9.27502432238048E-5));
#37396=CARTESIAN_POINT('',(218.519679545343,-4.94230926220351,-8.20892703918941E-5));
#37397=CARTESIAN_POINT('',(215.7,-4.942,-6.05220448138622E-16));
#37398=CARTESIAN_POINT('Ctrl Pts',(218.664320454657,-4.94227242746027,-9.27502432238048E-5));
#37399=CARTESIAN_POINT('Ctrl Pts',(218.641163117946,-4.94165288350105,0.718852082944881));
#37400=CARTESIAN_POINT('Ctrl Pts',(218.618005781236,-4.78292211280577,1.43806153059028));
#37401=CARTESIAN_POINT('Ctrl Pts',(218.594848444525,-4.47899749627878,2.08953535774377));
#37402=CARTESIAN_POINT('Ctrl Pts',(218.568451920839,-4.13256070870011,2.83213561977484));
#37403=CARTESIAN_POINT('Ctrl Pts',(218.542055397154,-3.5974705980024,3.48672560956518));
#37404=CARTESIAN_POINT('Ctrl Pts',(218.515658873468,-2.93860767782546,3.9739352660503));
#37405=CARTESIAN_POINT('Ctrl Pts',(218.489262349782,-2.27974475764855,4.46114492253539));
#37406=CARTESIAN_POINT('Ctrl Pts',(218.462865826096,-1.49710902799241,4.7809742457153));
#37407=CARTESIAN_POINT('Ctrl Pts',(218.43646930241,-0.685596296344016,4.89464342944124));
#37408=CARTESIAN_POINT('Ctrl Pts',(218.410072778725,0.125916435304404,5.00831261316719));
#37409=CARTESIAN_POINT('Ctrl Pts',(218.383676255039,0.966306168945093,4.91582165743917));
#37410=CARTESIAN_POINT('Ctrl Pts',(218.357279731353,1.73367433369038,4.6283852354397));
#37411=CARTESIAN_POINT('Ctrl Pts',(218.330883207667,2.50104249843566,4.34094881344022));
#37412=CARTESIAN_POINT('Ctrl Pts',(218.304486683981,3.19538909428554,3.85856692516929));
#37413=CARTESIAN_POINT('Ctrl Pts',(218.278090160295,3.73252350944933,3.23972912977937));
#37414=CARTESIAN_POINT('Ctrl Pts',(218.251693636609,4.26965792461312,2.62089133438945));
#37415=CARTESIAN_POINT('Ctrl Pts',(218.225297112923,4.64958015909082,1.86559763188054));
#37416=CARTESIAN_POINT('Ctrl Pts',(218.198900589238,4.82622404715952,1.06542856614232));
#37417=CARTESIAN_POINT('Ctrl Pts',(218.172504065552,5.00286793522823,0.265259500404091));
#37418=CARTESIAN_POINT('Ctrl Pts',(218.146107541866,4.97623347688792,-0.579784928563423));
#37419=CARTESIAN_POINT('Ctrl Pts',(218.11971101818,4.74955014191032,-1.36724176077701));
#37420=CARTESIAN_POINT('Ctrl Pts',(218.093314494494,4.52286680693272,-2.15469859299058));
#37421=CARTESIAN_POINT('Ctrl Pts',(218.066917970808,4.09613459531782,-2.8845678284502));
#37422=CARTESIAN_POINT('Ctrl Pts',(218.040521447123,3.52109545580043,-3.46835167969953));
#37423=CARTESIAN_POINT('Ctrl Pts',(218.014124923437,2.94605631628303,-4.05213553094886));
#37424=CARTESIAN_POINT('Ctrl Pts',(217.987728399751,2.22271024886315,-4.48983399798791));
#37425=CARTESIAN_POINT('Ctrl Pts',(217.961331876065,1.43876409665984,-4.72837545644332));
#37426=CARTESIAN_POINT('Ctrl Pts',(217.934935352379,0.654817944456556,-4.96691691489872));
#37427=CARTESIAN_POINT('Ctrl Pts',(217.908538828693,-0.189728292530149,
-5.00630136477049));
#37428=CARTESIAN_POINT('Ctrl Pts',(217.882142305007,-0.99247206087463,-4.84175337985282));
#37429=CARTESIAN_POINT('Ctrl Pts',(217.855745781322,-1.79521582921913,-4.67720539493514));
#37430=CARTESIAN_POINT('Ctrl Pts',(217.829349257636,-2.55615712892142,-4.308724975228));
#37431=CARTESIAN_POINT('Ctrl Pts',(217.80295273395,-3.18303063609043,-3.7809909485005));
#37432=CARTESIAN_POINT('Ctrl Pts',(217.776556210264,-3.80990414325944,-3.253256921773));
#37433=CARTESIAN_POINT('Ctrl Pts',(217.750159686578,-4.30270985789518,-2.56626928802512));
#37434=CARTESIAN_POINT('Ctrl Pts',(217.723763162892,-4.60169431557929,-1.80332637337177));
#37435=CARTESIAN_POINT('Ctrl Pts',(217.703948926814,-4.82612343733975,-1.23063236240104));
#37436=CARTESIAN_POINT('Ctrl Pts',(217.684134690735,-4.94134251052207,-0.615140775726203));
#37437=CARTESIAN_POINT('Ctrl Pts',(217.664320454657,-4.94195837962584,0.000126603499120692));
#37438=CARTESIAN_POINT('Ctrl Pts',(217.519679545343,-4.94191411506509,0.000125076744195484));
#37439=CARTESIAN_POINT('Ctrl Pts',(217.53902482689,-4.94132943881606,-0.600595899744503));
#37440=CARTESIAN_POINT('Ctrl Pts',(217.558370108438,-4.83162136351427,-1.20152460424478));
#37441=CARTESIAN_POINT('Ctrl Pts',(217.577715389985,-4.61745498945683,-1.76257938588247));
#37442=CARTESIAN_POINT('Ctrl Pts',(217.604111913671,-4.32522622288702,-2.5281353586054));
#37443=CARTESIAN_POINT('Ctrl Pts',(217.630508437357,-3.83851236700038,-3.21945229487338));
#37444=CARTESIAN_POINT('Ctrl Pts',(217.656904961043,-3.21632823880477,-3.75270693386316));
#37445=CARTESIAN_POINT('Ctrl Pts',(217.683301484729,-2.59414411060916,-4.28596157285295));
#37446=CARTESIAN_POINT('Ctrl Pts',(217.709698008414,-1.83648971010458,-4.66115391456454));
#37447=CARTESIAN_POINT('Ctrl Pts',(217.7360945321,-1.0352318195085,-4.83279130017786));
#37448=CARTESIAN_POINT('Ctrl Pts',(217.762491055786,-0.233973928912422,
-5.00442868579118));
#37449=CARTESIAN_POINT('Ctrl Pts',(217.788887579472,0.610887451775157,-4.97251111530622));
#37450=CARTESIAN_POINT('Ctrl Pts',(217.815284103158,1.39691155746148,-4.7409086441133));
#37451=CARTESIAN_POINT('Ctrl Pts',(217.841680626844,2.1829356631478,-4.50930617292037));
#37452=CARTESIAN_POINT('Ctrl Pts',(217.868077150529,2.91012249383287,-4.07801880101947));
#37453=CARTESIAN_POINT('Ctrl Pts',(217.894473674215,3.49029950783875,-3.49934079746146));
#37454=CARTESIAN_POINT('Ctrl Pts',(217.920870197901,4.07047652184462,-2.92066279390347));
#37455=CARTESIAN_POINT('Ctrl Pts',(217.947266721587,4.50364371917131,-2.19459415868837));
#37456=CARTESIAN_POINT('Ctrl Pts',(217.973663245273,4.73727889899207,-1.40917185054278));
#37457=CARTESIAN_POINT('Ctrl Pts',(218.000059768959,4.97091407881283,-0.623749542397181));
#37458=CARTESIAN_POINT('Ctrl Pts',(218.026456292645,5.00501724112767,0.221026438678921));
#37459=CARTESIAN_POINT('Ctrl Pts',(218.05285281633,4.83545332411523,1.02272568242937));
#37460=CARTESIAN_POINT('Ctrl Pts',(218.079249340016,4.66588940710279,1.82442492617982));
#37461=CARTESIAN_POINT('Ctrl Pts',(218.105645863702,4.29265841076308,2.58304743260462));
#37462=CARTESIAN_POINT('Ctrl Pts',(218.132042387388,3.7610151777192,3.20660903512783));
#37463=CARTESIAN_POINT('Ctrl Pts',(218.158438911074,3.22937194467533,3.83017063765104));
#37464=CARTESIAN_POINT('Ctrl Pts',(218.18483543476,2.5393164749273,4.31867133627266));
#37465=CARTESIAN_POINT('Ctrl Pts',(218.211231958445,1.77451907450792,4.61287965650582));
#37466=CARTESIAN_POINT('Ctrl Pts',(218.237628482131,1.00972167408854,4.90708797673897));
#37467=CARTESIAN_POINT('Ctrl Pts',(218.264025005817,0.170182342997809,5.00700391858366));
#37468=CARTESIAN_POINT('Ctrl Pts',(218.290421529503,-0.642303460517146,
4.90051251766643));
#37469=CARTESIAN_POINT('Ctrl Pts',(218.316818053189,-1.45478926403208,4.7940211167492));
#37470=CARTESIAN_POINT('Ctrl Pts',(218.343214576875,-2.24022153997123,4.48112237307008));
#37471=CARTESIAN_POINT('Ctrl Pts',(218.369611100561,-2.90336539523267,3.99975574916308));
#37472=CARTESIAN_POINT('Ctrl Pts',(218.396007624246,-3.56650925049412,3.51838912525607));
#37473=CARTESIAN_POINT('Ctrl Pts',(218.422404147932,-4.10736468507784,2.86855462112118));
#37474=CARTESIAN_POINT('Ctrl Pts',(218.448800671618,-4.46035213079688,2.12904568774214));
#37475=CARTESIAN_POINT('Ctrl Pts',(218.47242696286,-4.77629465021573,1.46714589958227));
#37476=CARTESIAN_POINT('Ctrl Pts',(218.496053254102,-4.94173234535399,0.733406122622747));
#37477=CARTESIAN_POINT('Ctrl Pts',(218.519679545343,-4.94230926220351,-8.20892703918941E-5));
#37478=CARTESIAN_POINT('Origin',(215.7,0.,0.));
#37479=CARTESIAN_POINT('',(219.664320454657,-4.94158767198665,-3.94523114399803E-6));
#37480=CARTESIAN_POINT('',(219.519679545343,-4.94159107100858,-1.73410261375781E-5));
#37481=CARTESIAN_POINT('',(215.7,-4.942,-6.05220448138622E-16));
#37482=CARTESIAN_POINT('Ctrl Pts',(219.664320454657,-4.94158767198665,-3.94523114399803E-6));
#37483=CARTESIAN_POINT('Ctrl Pts',(219.650984592529,-4.94157610618106,0.41418746593572));
#37484=CARTESIAN_POINT('Ctrl Pts',(219.637648730401,-4.8900661808863,0.828381702435691));
#37485=CARTESIAN_POINT('Ctrl Pts',(219.624312868274,-4.78709218279223,1.22935959604286));
#37486=CARTESIAN_POINT('Ctrl Pts',(219.597916344588,-4.58326917130133,2.02304075176169));
#37487=CARTESIAN_POINT('Ctrl Pts',(219.571519820902,-4.17781602960576,2.76494184435379));
#37488=CARTESIAN_POINT('Ctrl Pts',(219.545123297216,-3.61989458589892,3.3651062048489));
#37489=CARTESIAN_POINT('Ctrl Pts',(219.51872677353,-3.06197314219209,3.965270565344));
#37490=CARTESIAN_POINT('Ctrl Pts',(219.492330249844,-2.351583396474,4.4236981937421));
#37491=CARTESIAN_POINT('Ctrl Pts',(219.465933726158,-1.5748612175734,4.68480402240224));
#37492=CARTESIAN_POINT('Ctrl Pts',(219.439537202473,-0.798139038672788,
4.94590985106238));
#37493=CARTESIAN_POINT('Ctrl Pts',(219.413140678787,0.0449155734103233,
5.00969387998454));
#37494=CARTESIAN_POINT('Ctrl Pts',(219.386744155101,0.852080927105088,4.86842219580397));
#37495=CARTESIAN_POINT('Ctrl Pts',(219.360347631415,1.65924628079983,4.72715051162339));
#37496=CARTESIAN_POINT('Ctrl Pts',(219.333951107729,2.43052237610621,4.38082311434008));
#37497=CARTESIAN_POINT('Ctrl Pts',(219.307554584043,3.07239077898644,3.87143274307227));
#37498=CARTESIAN_POINT('Ctrl Pts',(219.281158060357,3.7142591818667,3.36204237180443));
#37499=CARTESIAN_POINT('Ctrl Pts',(219.254761536672,4.22671989232077,2.68958902655207));
#37500=CARTESIAN_POINT('Ctrl Pts',(219.228365012986,4.54763624691617,1.93560872819564));
#37501=CARTESIAN_POINT('Ctrl Pts',(219.2019684893,4.86855260151157,1.18162842983922));
#37502=CARTESIAN_POINT('Ctrl Pts',(219.175571965614,4.9979246002483,0.346121178378721));
#37503=CARTESIAN_POINT('Ctrl Pts',(219.149175441928,4.9200656857394,-0.469606463906328));
#37504=CARTESIAN_POINT('Ctrl Pts',(219.122778918242,4.84220677123051,-1.28533410619134));
#37505=CARTESIAN_POINT('Ctrl Pts',(219.096382394557,4.55711694347603,-2.08128213930093));
#37506=CARTESIAN_POINT('Ctrl Pts',(219.069985870871,4.09936379041748,-2.76094061811314));
#37507=CARTESIAN_POINT('Ctrl Pts',(219.043589347185,3.64161063735894,-3.44059909692535));
#37508=CARTESIAN_POINT('Ctrl Pts',(219.017192823499,3.01119415899634,-4.00396802144018));
#37509=CARTESIAN_POINT('Ctrl Pts',(218.990796299813,2.28455334028836,-4.38273802757024));
#37510=CARTESIAN_POINT('Ctrl Pts',(218.964399776127,1.55791252158036,-4.7615080337003));
#37511=CARTESIAN_POINT('Ctrl Pts',(218.938003252441,0.735047362526965,-4.95567912144557));
#37512=CARTESIAN_POINT('Ctrl Pts',(218.911606728756,-0.0842684480886987,
-4.9417077424297));
#37513=CARTESIAN_POINT('Ctrl Pts',(218.88521020507,-0.903584258704351,-4.92773636341384));
#37514=CARTESIAN_POINT('Ctrl Pts',(218.858813681384,-1.7193507208823,-4.70562251763684));
#37515=CARTESIAN_POINT('Ctrl Pts',(218.832417157698,-2.43265487394899,-4.30229785663257));
#37516=CARTESIAN_POINT('Ctrl Pts',(218.806020634012,-3.1459590270157,-3.89897319562828));
#37517=CARTESIAN_POINT('Ctrl Pts',(218.779624110326,-3.75680087097117,-3.31443771939671));
#37518=CARTESIAN_POINT('Ctrl Pts',(218.753227586641,-4.19111487592392,-2.61956726955851));
#37519=CARTESIAN_POINT('Ctrl Pts',(218.726831062955,-4.62542888087664,-1.92469681972034));
#37520=CARTESIAN_POINT('Ctrl Pts',(218.700434539269,-4.88321504682666,-1.11949139627556));
#37521=CARTESIAN_POINT('Ctrl Pts',(218.674038015583,-4.93321639757186,-0.301583417417288));
#37522=CARTESIAN_POINT('Ctrl Pts',(218.670798828608,-4.93935219507348,-0.201215774174882));
#37523=CARTESIAN_POINT('Ctrl Pts',(218.667559641632,-4.94235908762972,-0.100656850889163));
#37524=CARTESIAN_POINT('Ctrl Pts',(218.664320454657,-4.94227242746027,-9.27502432238048E-5));
#37525=CARTESIAN_POINT('Ctrl Pts',(218.519679545343,-4.94230926220351,-8.20892703918941E-5));
#37526=CARTESIAN_POINT('Ctrl Pts',(218.522449777787,-4.94237690692006,-0.0860851280561018));
#37527=CARTESIAN_POINT('Ctrl Pts',(218.525220010232,-4.94017803630086,-0.172084708311003));
#37528=CARTESIAN_POINT('Ctrl Pts',(218.527990242676,-4.93568950871128,-0.257964619269936));
#37529=CARTESIAN_POINT('Ctrl Pts',(218.554386766362,-4.8929199840523,-1.07628263027977));
#37530=CARTESIAN_POINT('Ctrl Pts',(218.580783290047,-4.64226147788,-1.88373528967626));
#37531=CARTESIAN_POINT('Ctrl Pts',(218.607179813733,-4.21410672648965,-2.58241769838892));
#37532=CARTESIAN_POINT('Ctrl Pts',(218.633576337419,-3.7859519750993,-3.28110010710158));
#37533=CARTESIAN_POINT('Ctrl Pts',(218.659972861105,-3.1803009784909,-3.87101226513042));
#37534=CARTESIAN_POINT('Ctrl Pts',(218.686369384791,-2.4705898681885,-4.28062639976932));
#37535=CARTESIAN_POINT('Ctrl Pts',(218.712765908477,-1.76087875788611,-4.69024053440821));
#37536=CARTESIAN_POINT('Ctrl Pts',(218.739162432163,-0.947107533889707,
-4.91955664565717));
#37537=CARTESIAN_POINT('Ctrl Pts',(218.765558955848,-0.127947231119626,
-4.94076979601827));
#37538=CARTESIAN_POINT('Ctrl Pts',(218.791955479534,0.691213071650503,-4.96198294637938));
#37539=CARTESIAN_POINT('Ctrl Pts',(218.81835200322,1.51576245319432,-4.77509313585261));
#37540=CARTESIAN_POINT('Ctrl Pts',(218.844748526906,2.24572301011498,-4.40276104655224));
#37541=CARTESIAN_POINT('Ctrl Pts',(218.871145050592,2.97568356703559,-4.03042895725189));
#37542=CARTESIAN_POINT('Ctrl Pts',(218.897541574278,3.61105529933306,-3.47265458917798));
#37543=CARTESIAN_POINT('Ctrl Pts',(218.923938097963,4.07479838975134,-2.79706895769081));
#37544=CARTESIAN_POINT('Ctrl Pts',(218.950334621649,4.53854148016963,-2.12148332620362));
#37545=CARTESIAN_POINT('Ctrl Pts',(218.976731145335,4.83065592870871,-1.32808643130321));
#37546=CARTESIAN_POINT('Ctrl Pts',(219.003127669021,4.91572240115944,-0.513078888609636));
#37547=CARTESIAN_POINT('Ctrl Pts',(219.029524192707,5.00078887361018,0.301928654083976));
#37548=CARTESIAN_POINT('Ctrl Pts',(219.055920716393,4.87880736997254,1.13854684457073));
#37549=CARTESIAN_POINT('Ctrl Pts',(219.082317240079,4.56456833853241,1.89533441747495));
#37550=CARTESIAN_POINT('Ctrl Pts',(219.108713763764,4.25032930709229,2.65212199037915));
#37551=CARTESIAN_POINT('Ctrl Pts',(219.13511028745,3.74383274784969,3.32907894570083));
#37552=CARTESIAN_POINT('Ctrl Pts',(219.161506811136,3.10649216156546,3.84412319278793));
#37553=CARTESIAN_POINT('Ctrl Pts',(219.187903334822,2.46915157528122,4.35916743987503));
#37554=CARTESIAN_POINT('Ctrl Pts',(219.214299858508,1.70096696195534,4.71229897872756));
#37555=CARTESIAN_POINT('Ctrl Pts',(219.240696382194,0.895081908595595,4.86070005740969));
#37556=CARTESIAN_POINT('Ctrl Pts',(219.26709290588,0.0891968552358766,5.00910113609182));
#37557=CARTESIAN_POINT('Ctrl Pts',(219.293489429565,-0.754388638157707,
4.95277175460356));
#37558=CARTESIAN_POINT('Ctrl Pts',(219.319885953251,-1.53338850982428,4.69854193863762));
#37559=CARTESIAN_POINT('Ctrl Pts',(219.346282476937,-2.31238838149088,4.44431212267166));
#37560=CARTESIAN_POINT('Ctrl Pts',(219.372679000623,-3.02680263143046,3.99218187222801));
#37561=CARTESIAN_POINT('Ctrl Pts',(219.399075524309,-3.59000741337678,3.39697268801169));
#37562=CARTESIAN_POINT('Ctrl Pts',(219.425472047995,-4.1532121953231,2.80176350379538));
#37563=CARTESIAN_POINT('Ctrl Pts',(219.45186857168,-4.56520750927616,2.0634753858064));
#37564=CARTESIAN_POINT('Ctrl Pts',(219.478265095366,-4.7760382784142,1.27162692418807));
#37565=CARTESIAN_POINT('Ctrl Pts',(219.492069912025,-4.88629825615422,0.857507134612465));
#37566=CARTESIAN_POINT('Ctrl Pts',(219.505874728684,-4.94153840270628,0.428738237424155));
#37567=CARTESIAN_POINT('Ctrl Pts',(219.519679545343,-4.94159107100858,-1.73410261375781E-5));
#37568=CARTESIAN_POINT('Origin',(215.7,0.,0.));
#37569=CARTESIAN_POINT('',(220.664320454657,-4.94224935728931,9.83974689322542E-5));
#37570=CARTESIAN_POINT('',(220.519679545343,-4.94220801981422,0.000106916500303121));
#37571=CARTESIAN_POINT('',(215.7,-4.942,-6.05220448138622E-16));
#37572=CARTESIAN_POINT('Ctrl Pts',(220.664320454657,-4.94224935728931,9.83974689322542E-5));
#37573=CARTESIAN_POINT('Ctrl Pts',(220.660806067112,-4.9423474261517,0.109207874409882));
#37574=CARTESIAN_POINT('Ctrl Pts',(220.657291679567,-4.93880747706411,0.218310997006985));
#37575=CARTESIAN_POINT('Ctrl Pts',(220.653777292022,-4.93158559359821,0.327169853757778));
#37576=CARTESIAN_POINT('Ctrl Pts',(220.627380768336,-4.8773421114786,1.14480745170729));
#37577=CARTESIAN_POINT('Ctrl Pts',(220.60098424465,-4.61538250376007,1.9486648053616));
#37578=CARTESIAN_POINT('Ctrl Pts',(220.574587720964,-4.17746978173744,2.64127295196166));
#37579=CARTESIAN_POINT('Ctrl Pts',(220.548191197278,-3.73955705971481,3.33388109856173));
#37580=CARTESIAN_POINT('Ctrl Pts',(220.521794673592,-3.12569122338807,3.91524003810755));
#37581=CARTESIAN_POINT('Ctrl Pts',(220.495398149907,-2.41030446704932,4.31485908908992));
#37582=CARTESIAN_POINT('Ctrl Pts',(220.469001626221,-1.69491771071057,4.7144781400723));
#37583=CARTESIAN_POINT('Ctrl Pts',(220.442605102535,-0.878010034359826,
4.93235730249122));
#37584=CARTESIAN_POINT('Ctrl Pts',(220.416208578849,-0.0586327723971473,
4.94207838676895));
#37585=CARTESIAN_POINT('Ctrl Pts',(220.389812055163,0.760744489565531,4.95179947104668));
#37586=CARTESIAN_POINT('Ctrl Pts',(220.363415531477,1.58259133714014,4.75336247718321));
#37587=CARTESIAN_POINT('Ctrl Pts',(220.337019007791,2.3072575532734,4.37082820136474));
#37588=CARTESIAN_POINT('Ctrl Pts',(220.310622484106,3.03192376940667,3.98829392554627));
#37589=CARTESIAN_POINT('Ctrl Pts',(220.28422596042,3.65940935409858,3.42166236777279));
#37590=CARTESIAN_POINT('Ctrl Pts',(220.257829436734,4.11363069789834,2.73963849151537));
#37591=CARTESIAN_POINT('Ctrl Pts',(220.231432913048,4.5678520416981,2.05761461525795));
#37592=CARTESIAN_POINT('Ctrl Pts',(220.205036389362,4.8488091446057,1.2601984205166));
#37593=CARTESIAN_POINT('Ctrl Pts',(220.178639865676,4.92243551800822,0.444077869312822));
#37594=CARTESIAN_POINT('Ctrl Pts',(220.152243341991,4.99606189141075,-0.372042681890931));
#37595=CARTESIAN_POINT('Ctrl Pts',(220.125846818305,4.8623575353082,-1.2068675895571));
#37596=CARTESIAN_POINT('Ctrl Pts',(220.099450294619,4.53753431221443,-1.95917302666104));
#37597=CARTESIAN_POINT('Ctrl Pts',(220.073053770933,4.21271108912065,-2.711478463765));
#37598=CARTESIAN_POINT('Ctrl Pts',(220.046657247247,3.69676899903564,-3.38126443030673));
#37599=CARTESIAN_POINT('Ctrl Pts',(220.020260723561,3.05226682811599,-3.88731832924966));
#37600=CARTESIAN_POINT('Ctrl Pts',(219.993864199875,2.40776465719635,-4.39337222819259));
#37601=CARTESIAN_POINT('Ctrl Pts',(219.96746767619,1.63470240544207,-4.73569405953674));
#37602=CARTESIAN_POINT('Ctrl Pts',(219.941071152504,0.826815081159675,-4.87277676530528));
#37603=CARTESIAN_POINT('Ctrl Pts',(219.914674628818,0.0189277568772817,
-5.00985947107383));
#37604=CARTESIAN_POINT('Ctrl Pts',(219.888278105132,-0.823784639933227,
-4.94170305126679));
#37605=CARTESIAN_POINT('Ctrl Pts',(219.861881581446,-1.59914191184,-4.67657157848882));
#37606=CARTESIAN_POINT('Ctrl Pts',(219.83548505776,-2.37449918374677,-4.41144010571084));
#37607=CARTESIAN_POINT('Ctrl Pts',(219.809088534074,-3.0825013307498,-3.94933357996195));
#37608=CARTESIAN_POINT('Ctrl Pts',(219.782692010389,-3.63730198410177,-3.34628314094649));
#37609=CARTESIAN_POINT('Ctrl Pts',(219.756295486703,-4.19210263745373,-2.74323270193106));
#37610=CARTESIAN_POINT('Ctrl Pts',(219.729898963017,-4.59370179715464,-1.99923834964908));
#37611=CARTESIAN_POINT('Ctrl Pts',(219.703502439331,-4.79340493636199,-1.20451056408532));
#37612=CARTESIAN_POINT('Ctrl Pts',(219.690441777773,-4.89221548976318,-0.811289442942511));
#37613=CARTESIAN_POINT('Ctrl Pts',(219.677381116215,-4.94159899911878,-0.405648049051028));
#37614=CARTESIAN_POINT('Ctrl Pts',(219.664320454657,-4.94158767198665,-3.94523114399803E-6));
#37615=CARTESIAN_POINT('Ctrl Pts',(219.519679545343,-4.94159107100858,-1.73410261375781E-5));
#37616=CARTESIAN_POINT('Ctrl Pts',(219.53227125237,-4.94163911104044,-0.391095669943753));
#37617=CARTESIAN_POINT('Ctrl Pts',(219.544862959397,-4.89577279646112,-0.782162918064062));
#37618=CARTESIAN_POINT('Ctrl Pts',(219.557454666424,-4.803864906551,-1.1620923503773));
#37619=CARTESIAN_POINT('Ctrl Pts',(219.58385119011,-4.61119454122674,-1.95855435807664));
#37620=CARTESIAN_POINT('Ctrl Pts',(219.610247713796,-4.21618758625521,-2.70606956822765));
#37621=CARTESIAN_POINT('Ctrl Pts',(219.636644237481,-3.66673925333529,-3.31400059131676));
#37622=CARTESIAN_POINT('Ctrl Pts',(219.663040761167,-3.11729092041538,-3.92193161440586));
#37623=CARTESIAN_POINT('Ctrl Pts',(219.689437284853,-2.4134012095471,-4.39027845043306));
#37624=CARTESIAN_POINT('Ctrl Pts',(219.715833808539,-1.64041785015744,-4.66225331230324));
#37625=CARTESIAN_POINT('Ctrl Pts',(219.742230332225,-0.86743449076778,-4.93422817417342));
#37626=CARTESIAN_POINT('Ctrl Pts',(219.768626855911,-0.0253574828567601,
-5.00983106188657));
#37627=CARTESIAN_POINT('Ctrl Pts',(219.795023379597,0.783710018041144,-4.87989500694632));
#37628=CARTESIAN_POINT('Ctrl Pts',(219.821419903282,1.59277751893909,-4.74995895200607));
#37629=CARTESIAN_POINT('Ctrl Pts',(219.847816426968,2.36883551282391,-4.4144839544124));
#37630=CARTESIAN_POINT('Ctrl Pts',(219.874212950654,3.01778575296881,-3.91414688283106));
#37631=CARTESIAN_POINT('Ctrl Pts',(219.90060947434,3.66673599311367,-3.41380981124975));
#37632=CARTESIAN_POINT('Ctrl Pts',(219.927005998026,4.1885784795186,-2.7486106656808));
#37633=CARTESIAN_POINT('Ctrl Pts',(219.953402521712,4.52003899372927,-1.9992058839361));
#37634=CARTESIAN_POINT('Ctrl Pts',(219.979799045397,4.85149950793995,-1.24980110219136));
#37635=CARTESIAN_POINT('Ctrl Pts',(220.006195569083,4.99257804995633,-0.416190684270871));
#37636=CARTESIAN_POINT('Ctrl Pts',(220.032592092769,4.92616862569162,0.400548801582176));
#37637=CARTESIAN_POINT('Ctrl Pts',(220.058988616455,4.8597592014269,1.21728828743518));
#37638=CARTESIAN_POINT('Ctrl Pts',(220.085385140141,4.58586181088109,2.0171568412208));
#37639=CARTESIAN_POINT('Ctrl Pts',(220.111781663827,4.13768694146142,2.70316914854727));
#37640=CARTESIAN_POINT('Ctrl Pts',(220.138178187512,3.68951207204175,3.38918145587374));
#37641=CARTESIAN_POINT('Ctrl Pts',(220.164574711198,3.06705972374821,3.96133751674111));
#37642=CARTESIAN_POINT('Ctrl Pts',(220.190971234884,2.3458032183009,4.35026251302223));
#37643=CARTESIAN_POINT('Ctrl Pts',(220.21736775857,1.62454671285356,4.73918750930336));
#37644=CARTESIAN_POINT('Ctrl Pts',(220.243764282256,0.804486050252458,4.94488144099823));
#37645=CARTESIAN_POINT('Ctrl Pts',(220.270160805942,-0.0149451303061554,
4.94240359686225));
#37646=CARTESIAN_POINT('Ctrl Pts',(220.296557329628,-0.834376310864792,
4.93992575272628));
#37647=CARTESIAN_POINT('Ctrl Pts',(220.322953853313,-1.65317800938092,4.72927613275944));
#37648=CARTESIAN_POINT('Ctrl Pts',(220.349350376999,-2.37206923802024,4.33599633316731));
#37649=CARTESIAN_POINT('Ctrl Pts',(220.375746900685,-3.09096046665952,3.94271653357521));
#37650=CARTESIAN_POINT('Ctrl Pts',(220.402143424371,-3.70994122542199,3.36680655435784));
#37651=CARTESIAN_POINT('Ctrl Pts',(220.428539948057,-4.15395912826009,2.67809638212087));
#37652=CARTESIAN_POINT('Ctrl Pts',(220.454936471743,-4.59797703109819,1.98938620988389));
#37653=CARTESIAN_POINT('Ctrl Pts',(220.481332995429,-4.86703207801192,1.18787584462733));
#37654=CARTESIAN_POINT('Ctrl Pts',(220.507729519114,-4.9285009233269,0.370749672950385));
#37655=CARTESIAN_POINT('Ctrl Pts',(220.511712861191,-4.93777682044256,0.247442032142238));
#37656=CARTESIAN_POINT('Ctrl Pts',(220.515696203267,-4.94232555847162,0.123778787731126));
#37657=CARTESIAN_POINT('Ctrl Pts',(220.519679545343,-4.94220801981422,0.000106916500303121));
#37658=CARTESIAN_POINT('Origin',(215.7,0.,0.));
#37659=CARTESIAN_POINT('',(221.664320454657,-4.94199158848527,-0.000125892924181525));
#37660=CARTESIAN_POINT('',(221.519679545343,-4.94203042585278,-0.000125883567849882));
#37661=CARTESIAN_POINT('',(215.7,-4.942,-6.05220448138622E-16));
#37662=CARTESIAN_POINT('Ctrl Pts',(221.664320454657,-4.94199158848527,-0.000125892924181525));
#37663=CARTESIAN_POINT('Ctrl Pts',(221.644231018009,-4.9413595014958,0.623677216857374));
#37664=CARTESIAN_POINT('Ctrl Pts',(221.62414158136,-4.8228328568654,1.2477129064962));
#37665=CARTESIAN_POINT('Ctrl Pts',(221.604052144712,-4.59227556616025,1.82717265502392));
#37666=CARTESIAN_POINT('Ctrl Pts',(221.577655621026,-4.2893347176133,2.58855403394672));
#37667=CARTESIAN_POINT('Ctrl Pts',(221.551259097341,-3.79297680109525,3.27297657942667));
#37668=CARTESIAN_POINT('Ctrl Pts',(221.524862573655,-3.16337544666258,3.79745180908665));
#37669=CARTESIAN_POINT('Ctrl Pts',(221.498466049969,-2.53377409222991,4.32192703874663));
#37670=CARTESIAN_POINT('Ctrl Pts',(221.472069526283,-1.77092929988263,4.68645495258663));
#37671=CARTESIAN_POINT('Ctrl Pts',(221.445673002597,-0.967342154830876,
4.84683651533342));
#37672=CARTESIAN_POINT('Ctrl Pts',(221.419276478911,-0.16375500977912,5.00721807808021));
#37673=CARTESIAN_POINT('Ctrl Pts',(221.392879955225,0.680574487977104,4.96345328973378));
#37674=CARTESIAN_POINT('Ctrl Pts',(221.36648343154,1.46327240205375,4.72084844128926));
#37675=CARTESIAN_POINT('Ctrl Pts',(221.340086907854,2.24597031613039,4.47824359284474));
#37676=CARTESIAN_POINT('Ctrl Pts',(221.313690384168,2.96703664652745,4.03679868430212));
#37677=CARTESIAN_POINT('Ctrl Pts',(221.287293860482,3.53903987119754,3.45003972328623));
#37678=CARTESIAN_POINT('Ctrl Pts',(221.260897336796,4.11104309586764,2.86328076227034));
#37679=CARTESIAN_POINT('Ctrl Pts',(221.23450081311,4.53398321481077,2.13120774878118));
#37680=CARTESIAN_POINT('Ctrl Pts',(221.208104289424,4.75657859487517,1.3425856246213));
#37681=CARTESIAN_POINT('Ctrl Pts',(221.181707765739,4.97917397493956,0.553963500461416));
#37682=CARTESIAN_POINT('Ctrl Pts',(221.155311242053,5.00142461612522,-0.291207734369187));
#37683=CARTESIAN_POINT('Ctrl Pts',(221.128914718367,4.82063234918612,-1.09044971754622));
#37684=CARTESIAN_POINT('Ctrl Pts',(221.102518194681,4.63984008224701,-1.88969170072324));
#37685=CARTESIAN_POINT('Ctrl Pts',(221.076121670995,4.25600490718315,-2.64300443224668));
#37686=CARTESIAN_POINT('Ctrl Pts',(221.049725147309,3.71566755489277,-3.25904757674573));
#37687=CARTESIAN_POINT('Ctrl Pts',(221.023328623623,3.17533020260239,-3.87509072124477));
#37688=CARTESIAN_POINT('Ctrl Pts',(220.996932099938,2.47849067308549,-4.3538642787194));
#37689=CARTESIAN_POINT('Ctrl Pts',(220.970535576252,1.70964179607628,-4.63731619980054));
#37690=CARTESIAN_POINT('Ctrl Pts',(220.944139052566,0.940792919067059,-4.92076812088168));
#37691=CARTESIAN_POINT('Ctrl Pts',(220.91774252888,0.0999346945655297,-5.0088984055693));
#37692=CARTESIAN_POINT('Ctrl Pts',(220.891346005194,-0.710977475777925,
-4.89102112168558));
#37693=CARTESIAN_POINT('Ctrl Pts',(220.864949481508,-1.5218896461214,-4.77314383780185));
#37694=CARTESIAN_POINT('Ctrl Pts',(220.838552957823,-2.3028557623068,-4.44925898534677));
#37695=CARTESIAN_POINT('Ctrl Pts',(220.812156434137,-2.95918247211069,-3.95863810841745));
#37696=CARTESIAN_POINT('Ctrl Pts',(220.785759910451,-3.61550918191456,-3.46801723148815));
#37697=CARTESIAN_POINT('Ctrl Pts',(220.759363386765,-4.14719648533692,-2.81066033008462));
#37698=CARTESIAN_POINT('Ctrl Pts',(220.732966863079,-4.48977645878774,-2.0662729582605));
#37699=CARTESIAN_POINT('Ctrl Pts',(220.710084726939,-4.78674592661956,-1.4209920346718));
#37700=CARTESIAN_POINT('Ctrl Pts',(220.687202590798,-4.941610832075,-0.710312128852271));
#37701=CARTESIAN_POINT('Ctrl Pts',(220.664320454657,-4.94224935728931,9.83974689322542E-5));
#37702=CARTESIAN_POINT('Ctrl Pts',(220.519679545343,-4.94220801981422,0.000106916500303121));
#37703=CARTESIAN_POINT('Ctrl Pts',(220.542092726953,-4.94154666178272,-0.69576103981452));
#37704=CARTESIAN_POINT('Ctrl Pts',(220.564505908562,-4.79315067695678,-1.39190212180872));
#37705=CARTESIAN_POINT('Ctrl Pts',(220.586919090172,-4.50786581270915,-2.02650499277872));
#37706=CARTESIAN_POINT('Ctrl Pts',(220.613315613858,-4.1718792130602,-2.77389150873351));
#37707=CARTESIAN_POINT('Ctrl Pts',(220.639712137544,-3.64602337004608,-3.43592256254577));
#37708=CARTESIAN_POINT('Ctrl Pts',(220.66610866123,-2.99405912783336,-3.93232585250573));
#37709=CARTESIAN_POINT('Ctrl Pts',(220.692505184915,-2.34209488562064,-4.4287291424657));
#37710=CARTESIAN_POINT('Ctrl Pts',(220.718901708601,-1.56402224420932,-4.75950466857337));
#37711=CARTESIAN_POINT('Ctrl Pts',(220.745298232287,-0.754183729619758,
-4.88454538040227));
#37712=CARTESIAN_POINT('Ctrl Pts',(220.771694755973,0.0556547849698012,
-5.00958609223117));
#37713=CARTESIAN_POINT('Ctrl Pts',(220.798091279659,0.897259172737602,-4.92889198978129));
#37714=CARTESIAN_POINT('Ctrl Pts',(220.824487803345,1.66858358435085,-4.65224735938235));
#37715=CARTESIAN_POINT('Ctrl Pts',(220.850884327031,2.43990799596407,-4.37560272898341));
#37716=CARTESIAN_POINT('Ctrl Pts',(220.877280850716,3.14095243142275,-3.90300757063542));
#37717=CARTESIAN_POINT('Ctrl Pts',(220.903677374402,3.68671415482571,-3.29176478700478));
#37718=CARTESIAN_POINT('Ctrl Pts',(220.930073898088,4.23247587822868,-2.68052200337414));
#37719=CARTESIAN_POINT('Ctrl Pts',(220.956470421774,4.62295488957593,-1.93063159446086));
#37720=CARTESIAN_POINT('Ctrl Pts',(220.98286694546,4.81080499863636,-1.13301894668909));
#37721=CARTESIAN_POINT('Ctrl Pts',(221.009263469146,4.99865510769681,-0.33540629891727));
#37722=CARTESIAN_POINT('Ctrl Pts',(221.035659992831,4.98387631447041,0.509928587713042));
#37723=CARTESIAN_POINT('Ctrl Pts',(221.062056516517,4.76826056819422,1.30048753549871));
#37724=CARTESIAN_POINT('Ctrl Pts',(221.088453040203,4.55264482191805,2.09104648328436));
#37725=CARTESIAN_POINT('Ctrl Pts',(221.114849563889,4.1361921225921,2.82682949222537));
#37726=CARTESIAN_POINT('Ctrl Pts',(221.141246087575,3.56939801746833,3.4186217190299));
#37727=CARTESIAN_POINT('Ctrl Pts',(221.167642611261,3.00260391234456,4.01041394583443));
#37728=CARTESIAN_POINT('Ctrl Pts',(221.194039134947,2.28546840142296,4.45821539050247));
#37729=CARTESIAN_POINT('Ctrl Pts',(221.220435658632,1.50494527649849,4.70772943008145));
#37730=CARTESIAN_POINT('Ctrl Pts',(221.246832182318,0.724422151574042,4.95724346966042));
#37731=CARTESIAN_POINT('Ctrl Pts',(221.273228706004,-0.119488587353277,
5.00847010415033));
#37732=CARTESIAN_POINT('Ctrl Pts',(221.29962522969,-0.924461417308162,4.85519801696677));
#37733=CARTESIAN_POINT('Ctrl Pts',(221.326021753376,-1.72943424726307,4.70192592978319));
#37734=CARTESIAN_POINT('Ctrl Pts',(221.352418277062,-2.49546916824554,4.34415512092613));
#37735=CARTESIAN_POINT('Ctrl Pts',(221.378814800748,-3.1296832992209,3.82526587584749));
#37736=CARTESIAN_POINT('Ctrl Pts',(221.405211324433,-3.76389743019626,3.30637663076886));
#37737=CARTESIAN_POINT('Ctrl Pts',(221.431607848119,-4.26629077116451,2.62636894946865));
#37738=CARTESIAN_POINT('Ctrl Pts',(221.458004371805,-4.57594723172245,1.86769479654986));
#37739=CARTESIAN_POINT('Ctrl Pts',(221.478562762984,-4.81711681613945,1.27681699010054));
#37740=CARTESIAN_POINT('Ctrl Pts',(221.499121154164,-4.94137695401291,0.638222038707901));
#37741=CARTESIAN_POINT('Ctrl Pts',(221.519679545343,-4.94203042585278,-0.000125883567849882));
#37742=CARTESIAN_POINT('Origin',(207.493410108095,0.,0.));
#37743=CARTESIAN_POINT('',(221.993410108095,-4.37199255865188,-0.000111372696215136));
#37744=CARTESIAN_POINT('',(222.,-4.372,-3.09002298987926E-13));
#37745=CARTESIAN_POINT('',(207.493410108095,-4.372,-3.09002298987926E-13));
#37746=CARTESIAN_POINT('',(222.,-4.36825282109637,-0.180973177525291));
#37747=CARTESIAN_POINT('Ctrl Pts',(221.993410108095,-4.37199255865188,-0.000111372696215244));
#37748=CARTESIAN_POINT('Ctrl Pts',(221.99560673873,-4.372053701201,-0.06045261198359));
#37749=CARTESIAN_POINT('Ctrl Pts',(221.997803369365,-4.370867891782,-0.12079139131084));
#37750=CARTESIAN_POINT('Ctrl Pts',(222.,-4.36842834878727,-0.181075889670185));
#37751=CARTESIAN_POINT('Origin',(222.,0.,0.));
#37752=CARTESIAN_POINT('Origin',(207.493410108095,0.,0.));
#37753=CARTESIAN_POINT('',(220.993410108095,-4.37222059693825,8.70485094473427E-5));
#37754=CARTESIAN_POINT('',(221.190589891905,-4.37202691659821,-0.00011136441995574));
#37755=CARTESIAN_POINT('',(207.493410108095,-4.372,-3.09002298987926E-13));
#37756=CARTESIAN_POINT('Ctrl Pts',(220.993410108095,-4.37222059693825,8.70485094474523E-5));
#37757=CARTESIAN_POINT('Ctrl Pts',(221.016292244236,-4.37165571789394,-0.628386205451742));
#37758=CARTESIAN_POINT('Ctrl Pts',(221.065570904062,-4.07660766898167,-1.98237095103711));
#37759=CARTESIAN_POINT('Ctrl Pts',(221.141246087575,-2.72814027777575,-3.64956206171641));
#37760=CARTESIAN_POINT('Ctrl Pts',(221.220435658632,-0.655466951210102,
-4.50914800360244));
#37761=CARTESIAN_POINT('Ctrl Pts',(221.29962522969,1.57615920673447,-4.27525144067998));
#37762=CARTESIAN_POINT('Ctrl Pts',(221.378814800747,3.42556172983117,-3.00459300688041));
#37763=CARTESIAN_POINT('Ctrl Pts',(221.458004371805,4.44425500302777,-1.00531138270765));
#37764=CARTESIAN_POINT('Ctrl Pts',(221.537193942863,4.38520210748118,1.23776144530491));
#37765=CARTESIAN_POINT('Ctrl Pts',(221.61638351392,3.26272485129782,3.18067315006488));
#37766=CARTESIAN_POINT('Ctrl Pts',(221.695573084978,1.34902473201658,4.35226186322655));
#37767=CARTESIAN_POINT('Ctrl Pts',(221.774762656035,-0.891814137382579,
4.46841300931145));
#37768=CARTESIAN_POINT('Ctrl Pts',(221.853952227093,-2.91639371982429,3.50096094174254));
#37769=CARTESIAN_POINT('Ctrl Pts',(221.926834711113,-4.12880172544123,1.82918469772558));
#37770=CARTESIAN_POINT('Ctrl Pts',(221.973320671447,-4.37143337526095,0.551743583994388));
#37771=CARTESIAN_POINT('Ctrl Pts',(221.993410108095,-4.37199255865188,-0.000111372696215244));
#37772=CARTESIAN_POINT('',(222.,-1.59436307123045,4.07092009220233));
#37773=CARTESIAN_POINT('Origin',(222.,0.,0.));
#37774=CARTESIAN_POINT('Ctrl Pts',(221.190589891905,-4.37202691659821,-0.000111364419955705));
#37775=CARTESIAN_POINT('Ctrl Pts',(221.196428024412,-4.37219108482666,-0.160480092140677));
#37776=CARTESIAN_POINT('Ctrl Pts',(221.228662680604,-4.32440771702623,-1.04584244130126));
#37777=CARTESIAN_POINT('Ctrl Pts',(221.287293860482,-3.7409896782648,-2.60135569353455));
#37778=CARTESIAN_POINT('Ctrl Pts',(221.36648343154,-2.04579887264011,-4.07145650839735));
#37779=CARTESIAN_POINT('Ctrl Pts',(221.445673002597,0.14550072168771,-4.5542152892435));
#37780=CARTESIAN_POINT('Ctrl Pts',(221.524862573655,2.30152409777985,-3.93256490416486));
#37781=CARTESIAN_POINT('Ctrl Pts',(221.604052144712,3.89940335283094,-2.35725035066262));
#37782=CARTESIAN_POINT('Ctrl Pts',(221.68324171577,4.55170192744695,-0.210305677009054));
#37783=CARTESIAN_POINT('Ctrl Pts',(221.762431286827,4.10012073214107,1.98766009715916));
#37784=CARTESIAN_POINT('Ctrl Pts',(221.841620857885,2.65441560822601,3.70356057542857));
#37785=CARTESIAN_POINT('Ctrl Pts',(221.920810428942,0.56466538392668,4.52140736785216));
#37786=CARTESIAN_POINT('Ctrl Pts',(221.973603476314,-0.919183673409389,
4.33535198326386));
#37787=CARTESIAN_POINT('Ctrl Pts',(222.,-1.59436307123039,4.07092009220235));
#37788=CARTESIAN_POINT('Origin',(207.493410108095,0.,0.));
#37789=CARTESIAN_POINT('',(219.993410108095,-4.37163522904201,-3.49019642618775E-6));
#37790=CARTESIAN_POINT('',(220.190589891905,-4.37218402724156,9.45849734608484E-5));
#37791=CARTESIAN_POINT('',(207.493410108095,-4.372,-3.09002298987926E-13));
#37792=CARTESIAN_POINT('Ctrl Pts',(219.993410108095,-4.37163522904201,-3.49019642562065E-6));
#37793=CARTESIAN_POINT('Ctrl Pts',(220.006470769653,-4.37164524972628,-0.358861446873992));
#37794=CARTESIAN_POINT('Ctrl Pts',(220.045927954897,-4.2396615535932,-1.44298955297618));
#37795=CARTESIAN_POINT('Ctrl Pts',(220.111781663827,-3.35331469136689,-3.08501753966403));
#37796=CARTESIAN_POINT('Ctrl Pts',(220.190971234884,-1.47428673505533,-4.31144190059531));
#37797=CARTESIAN_POINT('Ctrl Pts',(220.270160805942,0.762260370684581,-4.49232810095734));
#37798=CARTESIAN_POINT('Ctrl Pts',(220.349350376999,2.81395694980418,-3.58381067078537));
#37799=CARTESIAN_POINT('Ctrl Pts',(220.428539948057,4.18326015772707,-1.80620793157832));
#37800=CARTESIAN_POINT('Ctrl Pts',(220.507729519115,4.53810967910322,0.409405886501342));
#37801=CARTESIAN_POINT('Ctrl Pts',(220.586919090172,3.79245339384702,2.52573749520784));
#37802=CARTESIAN_POINT('Ctrl Pts',(220.66610866123,2.12711528603252,4.02956985290854));
#37803=CARTESIAN_POINT('Ctrl Pts',(220.745298232287,-0.0540549391371643,
4.55621890420622));
#37804=CARTESIAN_POINT('Ctrl Pts',(220.824487803345,-2.22211667183979,3.97797060507901));
#37805=CARTESIAN_POINT('Ctrl Pts',(220.903677374402,-3.85130815489554,2.43505197879753));
#37806=CARTESIAN_POINT('Ctrl Pts',(220.959984809319,-4.34565384402969,0.918087508898033));
#37807=CARTESIAN_POINT('Ctrl Pts',(220.98989572055,-4.37230735474205,0.0966120653418909));
#37808=CARTESIAN_POINT('Ctrl Pts',(220.993410108095,-4.37222059693825,8.70485094474523E-5));
#37809=CARTESIAN_POINT('Ctrl Pts',(220.190589891905,-4.37218402724156,9.45849734610045E-5));
#37810=CARTESIAN_POINT('Ctrl Pts',(220.213003073515,-4.37159894886969,-0.615513408755456));
#37811=CARTESIAN_POINT('Ctrl Pts',(220.26181277881,-4.08570679415814,-1.95666340110848));
#37812=CARTESIAN_POINT('Ctrl Pts',(220.337019007791,-2.76029389481659,-3.62530417052153));
#37813=CARTESIAN_POINT('Ctrl Pts',(220.416208578849,-0.695299810488197,
-4.50317786546855));
#37814=CARTESIAN_POINT('Ctrl Pts',(220.495398149907,1.53830665449812,-4.28901682788606));
#37815=CARTESIAN_POINT('Ctrl Pts',(220.574587720964,3.39886894010639,-3.03475578035621));
#37816=CARTESIAN_POINT('Ctrl Pts',(220.653777292022,4.43519486338251,-1.044556953301));
#37817=CARTESIAN_POINT('Ctrl Pts',(220.732966863079,4.39597214951006,1.19895020433616));
#37818=CARTESIAN_POINT('Ctrl Pts',(220.812156434137,3.29071241572633,3.15170818597724));
#37819=CARTESIAN_POINT('Ctrl Pts',(220.891346005194,1.38744463724644,4.34016705855231));
#37820=CARTESIAN_POINT('Ctrl Pts',(220.970535576252,-0.852282851982811,
4.47612184162993));
#37821=CARTESIAN_POINT('Ctrl Pts',(221.049725147309,-2.88532899192737,3.52660303771061));
#37822=CARTESIAN_POINT('Ctrl Pts',(221.12307658586,-4.12037514219452,1.85492309998823));
#37823=CARTESIAN_POINT('Ctrl Pts',(221.170031500726,-4.37144881484117,0.564610836347166));
#37824=CARTESIAN_POINT('Ctrl Pts',(221.190589891905,-4.37202691659821,-0.000111364419955705));
#37825=CARTESIAN_POINT('Origin',(207.493410108095,0.,0.));
#37826=CARTESIAN_POINT('',(218.993410108095,-4.37224100624368,-8.20526232630265E-5));
#37827=CARTESIAN_POINT('',(219.190589891905,-4.37163823602782,-1.53409482898936E-5));
#37828=CARTESIAN_POINT('',(207.493410108095,-4.372,-3.09002298987926E-13));
#37829=CARTESIAN_POINT('Ctrl Pts',(218.993410108095,-4.37224100624368,-8.20526232626559E-5));
#37830=CARTESIAN_POINT('Ctrl Pts',(218.99664929507,-4.37231767120945,-0.0890472990870102));
#37831=CARTESIAN_POINT('Ctrl Pts',(219.026285005732,-4.34798024483397,-0.902959118710753));
#37832=CARTESIAN_POINT('Ctrl Pts',(219.082317240079,-3.8638878894494,-2.41504099698875));
#37833=CARTESIAN_POINT('Ctrl Pts',(219.161506811136,-2.24272204053807,-3.96639010792621));
#37834=CARTESIAN_POINT('Ctrl Pts',(219.240696382194,-0.077689074547423,
-4.55587719841812));
#37835=CARTESIAN_POINT('Ctrl Pts',(219.319885953251,2.10618373527536,-4.04054980326089));
#37836=CARTESIAN_POINT('Ctrl Pts',(219.399075524309,3.77930039456389,-2.54537642933601));
#37837=CARTESIAN_POINT('Ctrl Pts',(219.478265095366,4.53592487469901,-0.43294130139881));
#37838=CARTESIAN_POINT('Ctrl Pts',(219.557454666424,4.19257337016016,1.78448344772206));
#37839=CARTESIAN_POINT('Ctrl Pts',(219.636644237481,2.83250969587536,3.569165373325));
#37840=CARTESIAN_POINT('Ctrl Pts',(219.715833808539,0.785553551391572,4.48831352038449));
#37841=CARTESIAN_POINT('Ctrl Pts',(219.795023379596,-1.45190178897309,4.3190315852685));
#37842=CARTESIAN_POINT('Ctrl Pts',(219.874212950654,-3.33726639942199,3.10237096728598));
#37843=CARTESIAN_POINT('Ctrl Pts',(219.940341860154,-4.2358587294695,1.45812021942101));
#37844=CARTESIAN_POINT('Ctrl Pts',(219.980074245967,-4.37162499721238,0.366415945178225));
#37845=CARTESIAN_POINT('Ctrl Pts',(219.993410108095,-4.37163522904201,-3.49019642562065E-6));
#37846=CARTESIAN_POINT('Ctrl Pts',(219.190589891905,-4.37163823602782,-1.53409482897549E-5));
#37847=CARTESIAN_POINT('Ctrl Pts',(219.203181598932,-4.37168073522234,-0.345987508902117));
#37848=CARTESIAN_POINT('Ctrl Pts',(219.242169829645,-4.24604297815936,-1.41720529400801));
#37849=CARTESIAN_POINT('Ctrl Pts',(219.307554584043,-3.38045360582197,-3.05525549394406));
#37850=CARTESIAN_POINT('Ctrl Pts',(219.386744155101,-1.51233999842644,-4.29824155248976));
#37851=CARTESIAN_POINT('Ctrl Pts',(219.465933726158,0.722520793916989,-4.49889057621407));
#37852=CARTESIAN_POINT('Ctrl Pts',(219.545123297216,2.78216803143074,-3.60854454860609));
#37853=CARTESIAN_POINT('Ctrl Pts',(219.624312868274,4.16713080999959,-1.84311516914782));
#37854=CARTESIAN_POINT('Ctrl Pts',(219.703502439331,4.5415513193251,0.369275409857588));
#37855=CARTESIAN_POINT('Ctrl Pts',(219.782692010389,3.81463141353823,2.49211554572396));
#37856=CARTESIAN_POINT('Ctrl Pts',(219.861881581446,2.16265144586963,4.01060985862089));
#37857=CARTESIAN_POINT('Ctrl Pts',(219.941071152504,-0.0137782689576099,
4.55651872307046));
#37858=CARTESIAN_POINT('Ctrl Pts',(220.020260723561,-2.1868667104261,3.99745753013543));
#37859=CARTESIAN_POINT('Ctrl Pts',(220.099450294619,-3.82963312724697,2.46900036959006));
#37860=CARTESIAN_POINT('Ctrl Pts',(220.156226684067,-4.34159732403268,0.943867817456289));
#37861=CARTESIAN_POINT('Ctrl Pts',(220.186606549829,-4.37228800923471,0.109502399830049));
#37862=CARTESIAN_POINT('Ctrl Pts',(220.190589891905,-4.37218402724156,9.45849734610045E-5));
#37863=CARTESIAN_POINT('Origin',(207.493410108095,0.,0.));
#37864=CARTESIAN_POINT('',(217.993410108095,-4.37196318003322,0.000112001314848215));
#37865=CARTESIAN_POINT('',(218.190589891905,-4.37227359254426,-7.26212656684822E-5));
#37866=CARTESIAN_POINT('',(207.493410108095,-4.372,-3.09002298987926E-13));
#37867=CARTESIAN_POINT('Ctrl Pts',(217.993410108095,-4.37196318003322,0.000112001314848311));
#37868=CARTESIAN_POINT('Ctrl Pts',(218.013224344173,-4.37141834399079,-0.544191718226455));
#37869=CARTESIAN_POINT('Ctrl Pts',(218.059435103938,-4.13369733469641,-1.81407939528679));
#37870=CARTESIAN_POINT('Ctrl Pts',(218.132042387388,-2.93451119586052,-3.48578494470606));
#37871=CARTESIAN_POINT('Ctrl Pts',(218.211231958445,-0.914983456707324,
-4.46372690846136));
#37872=CARTESIAN_POINT('Ctrl Pts',(218.290421529503,1.32643063562732,-4.35920112041638));
#37873=CARTESIAN_POINT('Ctrl Pts',(218.369611100561,3.24618114559881,-3.1975554114556));
#37874=CARTESIAN_POINT('Ctrl Pts',(218.448800671618,4.37872256355528,-1.26049250326289));
#37875=CARTESIAN_POINT('Ctrl Pts',(218.527990242676,4.44941004951064,0.982243783733906));
#37876=CARTESIAN_POINT('Ctrl Pts',(218.607179813733,3.44110166678914,2.98678287764463));
#37877=CARTESIAN_POINT('Ctrl Pts',(218.686369384791,1.59831535534295,4.26701777172829));
#37878=CARTESIAN_POINT('Ctrl Pts',(218.765558955848,-0.632067434303197,
4.51248749559082));
#37879=CARTESIAN_POINT('Ctrl Pts',(218.844748526906,-2.70917189204705,3.66366487259853));
#37880=CARTESIAN_POINT('Ctrl Pts',(218.920698910988,-4.07120472088646,1.99745382197457));
#37881=CARTESIAN_POINT('Ctrl Pts',(218.970252771385,-4.37169291919601,0.635941179003326));
#37882=CARTESIAN_POINT('Ctrl Pts',(218.993410108095,-4.37224100624368,-8.20526232626559E-5));
#37883=CARTESIAN_POINT('Ctrl Pts',(218.190589891905,-4.37227359254426,-7.26212656684041E-5));
#37884=CARTESIAN_POINT('Ctrl Pts',(218.193360124349,-4.3723334352599,-0.0761562484549823));
#37885=CARTESIAN_POINT('Ctrl Pts',(218.222526880479,-4.35185253664576,-0.877180496390307));
#37886=CARTESIAN_POINT('Ctrl Pts',(218.278090160295,-3.88508462005382,-2.38079192904617));
#37887=CARTESIAN_POINT('Ctrl Pts',(218.357279731353,-2.27769520857755,-3.94641067949257));
#37888=CARTESIAN_POINT('Ctrl Pts',(218.43646930241,-0.117957577266953,-4.55501248344671));
#37889=CARTESIAN_POINT('Ctrl Pts',(218.515658873468,2.07038513587111,-4.05900949783985));
#37890=CARTESIAN_POINT('Ctrl Pts',(218.594848444525,3.75665297092044,-2.57868399973024));
#37891=CARTESIAN_POINT('Ctrl Pts',(218.674038015583,4.53192069796186,-0.473019557497457));
#37892=CARTESIAN_POINT('Ctrl Pts',(218.75322758664,4.20818346572563,1.74735360851304));
#37893=CARTESIAN_POINT('Ctrl Pts',(218.832417157698,2.86394856669164,3.54398805327205));
#37894=CARTESIAN_POINT('Ctrl Pts',(218.911606728756,0.825197172846602,4.48119429843385));
#37895=CARTESIAN_POINT('Ctrl Pts',(218.990796299813,-1.41366711921135,4.33169689503441));
#37896=CARTESIAN_POINT('Ctrl Pts',(219.069985870871,-3.30971270848846,3.13174943149354));
#37897=CARTESIAN_POINT('Ctrl Pts',(219.136583734901,-4.22927944508702,1.48390254504573));
#37898=CARTESIAN_POINT('Ctrl Pts',(219.176785075246,-4.37159164237796,0.379288460950675));
#37899=CARTESIAN_POINT('Ctrl Pts',(219.190589891905,-4.37163823602782,-1.53409482897549E-5));
#37900=CARTESIAN_POINT('Origin',(207.493410108095,0.,0.));
#37901=CARTESIAN_POINT('',(216.993410108095,-4.37172079063294,-7.45667008033409E-5));
#37902=CARTESIAN_POINT('',(217.190589891905,-4.37192402085483,0.000110650652629316));
#37903=CARTESIAN_POINT('',(207.493410108095,-4.372,-3.09002298987926E-13));
#37904=CARTESIAN_POINT('Ctrl Pts',(216.993410108095,-4.37172079063294,-7.45667008031012E-5));
#37905=CARTESIAN_POINT('Ctrl Pts',(217.003402869591,-4.37188869880949,-0.274622762470965));
#37906=CARTESIAN_POINT('Ctrl Pts',(217.039792154772,-4.27917236998106,-1.27429571461977));
#37907=CARTESIAN_POINT('Ctrl Pts',(217.10257796364,-3.52601195980057,-2.8860513333469));
#37908=CARTESIAN_POINT('Ctrl Pts',(217.181767534697,-1.72100782049271,-4.21902651344751));
#37909=CARTESIAN_POINT('Ctrl Pts',(217.260957105755,0.501346103979698,-4.52887455372684));
#37910=CARTESIAN_POINT('Ctrl Pts',(217.340146676813,2.60212202845841,-3.74045633424341));
#37911=CARTESIAN_POINT('Ctrl Pts',(217.41933624787,4.07187521345992,-2.04496574185997));
#37912=CARTESIAN_POINT('Ctrl Pts',(217.498525818928,4.55418590963663,0.146435445973139));
#37913=CARTESIAN_POINT('Ctrl Pts',(217.577715389985,3.93209226298936,2.3023255796497));
#37914=CARTESIAN_POINT('Ctrl Pts',(217.656904961043,2.35645393068466,3.89989455138609));
#37915=CARTESIAN_POINT('Ctrl Pts',(217.7360945321,0.209368141831046,4.55172688334399));
#37916=CARTESIAN_POINT('Ctrl Pts',(217.815284103158,-1.98849007697495,4.0997511940534));
#37917=CARTESIAN_POINT('Ctrl Pts',(217.894473674215,-3.70413322589841,2.65357300336085));
#37918=CARTESIAN_POINT('Ctrl Pts',(217.953849009194,-4.31699380515626,1.0867590052297));
#37919=CARTESIAN_POINT('Ctrl Pts',(217.986827820488,-4.37214417452203,0.180929652502748));
#37920=CARTESIAN_POINT('Ctrl Pts',(217.993410108095,-4.37196318003322,0.000112001314848311));
#37921=CARTESIAN_POINT('Ctrl Pts',(217.190589891905,-4.37192402085483,0.000110650652629211));
#37922=CARTESIAN_POINT('Ctrl Pts',(217.209935173452,-4.37140677994815,-0.531324417985278));
#37923=CARTESIAN_POINT('Ctrl Pts',(217.255676978685,-4.14192180632446,-1.78833405490227));
#37924=CARTESIAN_POINT('Ctrl Pts',(217.327815307605,-2.96520904301682,-3.45970924292799));
#37925=CARTESIAN_POINT('Ctrl Pts',(217.407004878662,-0.954404689107857,
-4.45546455532968));
#37926=CARTESIAN_POINT('Ctrl Pts',(217.48619444972,1.28784579027261,-4.37075576243597));
#37927=CARTESIAN_POINT('Ctrl Pts',(217.565384020777,3.21778963310249,-3.22612501175764));
#37928=CARTESIAN_POINT('Ctrl Pts',(217.644573591835,4.36740941459516,-1.2991488443191));
#37929=CARTESIAN_POINT('Ctrl Pts',(217.723763162892,4.45791873813246,0.942874985667582));
#37930=CARTESIAN_POINT('Ctrl Pts',(217.80295273395,3.46736880936034,2.95624867936802));
#37931=CARTESIAN_POINT('Ctrl Pts',(217.882142305007,1.63597108754423,4.25272281192996));
#37932=CARTESIAN_POINT('Ctrl Pts',(217.961331876065,-0.592154745435518,
4.5178983467812));
#37933=CARTESIAN_POINT('Ctrl Pts',(218.040521447122,-2.6766811985351,3.68746938642191));
#37934=CARTESIAN_POINT('Ctrl Pts',(218.116940785736,-4.06188970218061,2.02314982239138));
#37935=CARTESIAN_POINT('Ctrl Pts',(218.166963600663,-4.37176321608425,0.648816586018496));
#37936=CARTESIAN_POINT('Ctrl Pts',(218.190589891905,-4.37227359254426,-7.26212656684041E-5));
#37937=CARTESIAN_POINT('Origin',(207.493410108095,0.,0.));
#37938=CARTESIAN_POINT('',(215.993410108095,-4.37237677050361,-4.95149419051281E-6));
#37939=CARTESIAN_POINT('',(216.190589891905,-4.37174661086188,-8.31034356851834E-5));
#37940=CARTESIAN_POINT('',(207.493410108095,-4.372,-3.09002298987926E-13));
#37941=CARTESIAN_POINT('Ctrl Pts',(215.993410108095,-4.37237654485879,-4.94852878089684E-6));
#37942=CARTESIAN_POINT('Ctrl Pts',(215.993581395008,-4.3723768600723,-0.00470897188487751));
#37943=CARTESIAN_POINT('Ctrl Pts',(216.020149205607,-4.37122390828525,-0.734336079798519));
#37944=CARTESIAN_POINT('Ctrl Pts',(216.073113539892,-3.99700949719232,-2.18768547070287));
#37945=CARTESIAN_POINT('Ctrl Pts',(216.152303110949,-2.46821587915816,-3.83013877206057));
#37946=CARTESIAN_POINT('Ctrl Pts',(216.231492682007,-0.340872182129313,
-4.54377142854046));
#37947=CARTESIAN_POINT('Ctrl Pts',(216.310682253064,1.86913408638018,-4.15552528647124));
#37948=CARTESIAN_POINT('Ctrl Pts',(216.389871824122,3.62586948644518,-2.75955125095293));
#37949=CARTESIAN_POINT('Ctrl Pts',(216.469061395179,4.50332018298729,-0.694377396571518));
#37950=CARTESIAN_POINT('Ctrl Pts',(216.548250966237,4.28870163468497,1.5391851506627));
#37951=CARTESIAN_POINT('Ctrl Pts',(216.627440537294,3.03405951149959,3.39949047947615));
#37952=CARTESIAN_POINT('Ctrl Pts',(216.706630108352,1.04364845674816,4.43540872277824));
#37953=CARTESIAN_POINT('Ctrl Pts',(216.78581967941,-1.19985061656117,4.39572646297605));
#37954=CARTESIAN_POINT('Ctrl Pts',(216.865009250467,-3.15238215846906,3.29006677232181));
#37955=CARTESIAN_POINT('Ctrl Pts',(216.934206060029,-4.19053128720911,1.62675556634124));
#37956=CARTESIAN_POINT('Ctrl Pts',(216.977006345905,-4.37144515853675,0.450613995719711));
#37957=CARTESIAN_POINT('Ctrl Pts',(216.993410108095,-4.37172079063294,-7.45667008031012E-5));
#37958=CARTESIAN_POINT('Ctrl Pts',(216.190589891905,-4.37174661086188,-8.31034356850099E-5));
#37959=CARTESIAN_POINT('Ctrl Pts',(216.20011369887,-4.37192637963066,-0.261742485074944));
#37960=CARTESIAN_POINT('Ctrl Pts',(216.23603402952,-4.28475048323144,-1.24850796410071));
#37961=CARTESIAN_POINT('Ctrl Pts',(216.298350883856,-3.55138537175629,-2.85477050840615));
#37962=CARTESIAN_POINT('Ctrl Pts',(216.377540454914,-1.75823454219255,-4.20364889221627));
#37963=CARTESIAN_POINT('Ctrl Pts',(216.456730025972,0.46129366910955,-4.53312925750298));
#37964=CARTESIAN_POINT('Ctrl Pts',(216.535919597029,2.56895672128326,-3.76331158403921));
#37965=CARTESIAN_POINT('Ctrl Pts',(216.615109168087,4.05363972481456,-2.08087906803723));
#37966=CARTESIAN_POINT('Ctrl Pts',(216.694298739144,4.55530240261518,0.106173137461614));
#37967=CARTESIAN_POINT('Ctrl Pts',(216.773488310202,3.95228998454865,2.26747802468437));
#37968=CARTESIAN_POINT('Ctrl Pts',(216.852677881259,2.39083487010492,3.87891239115818));
#37969=CARTESIAN_POINT('Ctrl Pts',(216.931867452317,0.249594813651761,4.5496983574066));
#37970=CARTESIAN_POINT('Ctrl Pts',(217.011057023374,-1.95217276662517,4.11716822629792));
#37971=CARTESIAN_POINT('Ctrl Pts',(217.090246594432,-3.68053233849351,2.68621190893303));
#37972=CARTESIAN_POINT('Ctrl Pts',(217.150090883942,-4.31216843510475,1.11254484294713));
#37973=CARTESIAN_POINT('Ctrl Pts',(217.183538649767,-4.37211255214439,0.193815629342384));
#37974=CARTESIAN_POINT('Ctrl Pts',(217.190589891905,-4.37192402085483,0.000110650652629211));
#37975=CARTESIAN_POINT('Origin',(207.493410108095,0.,0.));
#37976=CARTESIAN_POINT('',(214.993410108095,-4.37173935379323,8.08904380046663E-5));
#37977=CARTESIAN_POINT('',(215.190589891905,-4.37237558886668,8.59259548038633E-6));
#37978=CARTESIAN_POINT('',(207.493410108095,-4.372,-3.09002298987926E-13));
#37979=CARTESIAN_POINT('Ctrl Pts',(214.993410108095,-4.37173935379323,8.08904380046604E-5));
#37980=CARTESIAN_POINT('Ctrl Pts',(215.010156444111,-4.37143236352728,-0.460014190704367));
#37981=CARTESIAN_POINT('Ctrl Pts',(215.053299303813,-4.18513208821824,-1.6455800269089));
#37982=CARTESIAN_POINT('Ctrl Pts',(215.122838687201,-3.13107142267409,-3.31035411783751));
#37983=CARTESIAN_POINT('Ctrl Pts',(215.202028258259,-1.17144099051237,-4.40338263669165));
#37984=CARTESIAN_POINT('Ctrl Pts',(215.281217829316,1.07226754977981,-4.42857707859527));
#37985=CARTESIAN_POINT('Ctrl Pts',(215.360407400374,3.05594785184388,-3.37982771249969));
#37986=CARTESIAN_POINT('Ctrl Pts',(215.439596971431,4.29855123127321,-1.5114595434512));
#37987=CARTESIAN_POINT('Ctrl Pts',(215.518786542489,4.49874247780649,0.723442297456857));
#37988=CARTESIAN_POINT('Ctrl Pts',(215.597976113546,3.60797458733507,2.7829071160415));
#37989=CARTESIAN_POINT('Ctrl Pts',(215.677165684604,1.84226156240618,4.16750824534888));
#37990=CARTESIAN_POINT('Ctrl Pts',(215.756355255662,-0.370205659762209,
4.54147557615916));
#37991=CARTESIAN_POINT('Ctrl Pts',(215.835544826719,-2.49289685027711,3.81412085981142));
#37992=CARTESIAN_POINT('Ctrl Pts',(215.914563110864,-4.0077689802887,2.16540379512807));
#37993=CARTESIAN_POINT('Ctrl Pts',(215.967184871322,-4.37232828344233,0.720214267893106));
#37994=CARTESIAN_POINT('Ctrl Pts',(215.993410108095,-4.37237654485879,-4.94852878089684E-6));
#37995=CARTESIAN_POINT('Ctrl Pts',(215.190589891905,-4.37237558886668,8.59259548050451E-6));
#37996=CARTESIAN_POINT('Ctrl Pts',(215.216688747973,-4.37229330250909,-0.716740314340791));
#37997=CARTESIAN_POINT('Ctrl Pts',(215.269184127726,-4.01049950323238,-2.15849297429132));
#37998=CARTESIAN_POINT('Ctrl Pts',(215.348076031166,-2.50197584827897,-3.8081714206452));
#37999=CARTESIAN_POINT('Ctrl Pts',(215.427265602223,-0.381023394472204,
-4.54058078743843));
#38000=CARTESIAN_POINT('Ctrl Pts',(215.506455173281,1.83232842552693,-4.17188509614013));
#38001=CARTESIAN_POINT('Ctrl Pts',(215.585644744338,3.60133486508171,-2.79149420632338));
#38002=CARTESIAN_POINT('Ctrl Pts',(215.664834315396,4.49700632361528,-0.734157230948736));
#38003=CARTESIAN_POINT('Ctrl Pts',(215.744023886454,4.30213966797164,1.50121517167094));
#38004=CARTESIAN_POINT('Ctrl Pts',(215.823213457511,3.06399067229672,3.3725381946642));
#38005=CARTESIAN_POINT('Ctrl Pts',(215.902403028569,1.08281434484414,4.42601014560404));
#38006=CARTESIAN_POINT('Ctrl Pts',(215.981592599626,-1.16094785166298,4.40616077783247));
#38007=CARTESIAN_POINT('Ctrl Pts',(216.060782170684,-3.12317655906599,3.31780362518501));
#38008=CARTESIAN_POINT('Ctrl Pts',(216.130447934777,-4.18312293967722,1.65252427293828));
#38009=CARTESIAN_POINT('Ctrl Pts',(216.173717175184,-4.37142812608763,0.463482006636045));
#38010=CARTESIAN_POINT('Ctrl Pts',(216.190589891905,-4.37174661086188,-8.31034356850099E-5));
#38011=CARTESIAN_POINT('Origin',(207.493410108095,0.,0.));
#38012=CARTESIAN_POINT('',(213.993410108095,-4.37193445885121,-0.000111146439951045));
#38013=CARTESIAN_POINT('',(214.190589891905,-4.3717143632787,7.2119750405969E-5));
#38014=CARTESIAN_POINT('',(207.493410108095,-4.372,-3.09002298987926E-13));
#38015=CARTESIAN_POINT('Ctrl Pts',(213.993410108095,-4.37193445885121,-0.00011114643995053));
#38016=CARTESIAN_POINT('Ctrl Pts',(214.000334969528,-4.37212121263154,-0.19034300863519));
#38017=CARTESIAN_POINT('Ctrl Pts',(214.033656354648,-4.31348053118326,-1.10559563790858));
#38018=CARTESIAN_POINT('Ctrl Pts',(214.093374263453,-3.68692103050771,-2.6774364519387));
#38019=CARTESIAN_POINT('Ctrl Pts',(214.172563834511,-1.96197521572409,-4.11250603552804));
#38020=CARTESIAN_POINT('Ctrl Pts',(214.251753405568,0.238755732067328,-4.55028002872078));
#38021=CARTESIAN_POINT('Ctrl Pts',(214.330942976626,2.38158766725776,-3.88459686744144));
#38022=CARTESIAN_POINT('Ctrl Pts',(214.410132547683,3.94687713608336,-2.27688680263919));
#38023=CARTESIAN_POINT('Ctrl Pts',(214.489322118741,4.55503654123292,-0.117024558973872));
#38024=CARTESIAN_POINT('Ctrl Pts',(214.568511689798,4.05858532273295,2.07121650666143));
#38025=CARTESIAN_POINT('Ctrl Pts',(214.647701260856,2.57791445552183,3.75718108418821));
#38026=CARTESIAN_POINT('Ctrl Pts',(214.726890831913,0.472091261067617,4.53201748458606));
#38027=CARTESIAN_POINT('Ctrl Pts',(214.806080402971,-1.74821554237347,4.20782545464685));
#38028=CARTESIAN_POINT('Ctrl Pts',(214.885269974028,-3.54457460290309,2.86322257671746));
#38029=CARTESIAN_POINT('Ctrl Pts',(214.94771320907,-4.2832591449728,1.25545762566034));
#38030=CARTESIAN_POINT('Ctrl Pts',(214.983759920425,-4.37191625897872,0.265213745447506));
#38031=CARTESIAN_POINT('Ctrl Pts',(214.993410108095,-4.37173935379323,8.08904380046604E-5));
#38032=CARTESIAN_POINT('Ctrl Pts',(214.190589891905,-4.3717143632787,7.21197504059343E-5));
#38033=CARTESIAN_POINT('Ctrl Pts',(214.20686727339,-4.37145034324393,-0.447146056196735));
#38034=CARTESIAN_POINT('Ctrl Pts',(214.249541178561,-4.19250586234899,-1.61981056612665));
#38035=CARTESIAN_POINT('Ctrl Pts',(214.318611607418,-3.16021087534511,-3.28254778148629));
#38036=CARTESIAN_POINT('Ctrl Pts',(214.397801178475,-1.21031879251578,-4.39285569247082));
#38037=CARTESIAN_POINT('Ctrl Pts',(214.476990749533,1.03307938716119,-4.43788234343958));
#38038=CARTESIAN_POINT('Ctrl Pts',(214.55618032059,3.02595258074822,-3.40670863054845));
#38039=CARTESIAN_POINT('Ctrl Pts',(214.635369891648,4.28502279886023,-1.54939740790998));
#38040=CARTESIAN_POINT('Ctrl Pts',(214.714559462705,4.50496157129557,0.683647537507614));
#38041=CARTESIAN_POINT('Ctrl Pts',(214.793749033763,3.63243305708234,2.75090581449194));
#38042=CARTESIAN_POINT('Ctrl Pts',(214.872938604821,1.87902815291533,4.15106081802492));
#38043=CARTESIAN_POINT('Ctrl Pts',(214.952128175878,-0.330046961810515,
4.54457057568587));
#38044=CARTESIAN_POINT('Ctrl Pts',(215.031317746936,-2.45908465487818,3.83600773911274));
#38045=CARTESIAN_POINT('Ctrl Pts',(215.110507317993,-3.99178661943011,2.19720101477514));
#38046=CARTESIAN_POINT('Ctrl Pts',(215.163598032983,-4.37036335382686,0.74128143659256));
#38047=CARTESIAN_POINT('Ctrl Pts',(215.190292224287,-4.37237652737464,0.00818339302941881));
#38048=CARTESIAN_POINT('Ctrl Pts',(215.190589891905,-4.37237558886668,8.59259548050451E-6));
#38049=CARTESIAN_POINT('Origin',(207.493410108095,0.,0.));
#38050=CARTESIAN_POINT('',(212.993410108095,-4.37226510377645,7.5272650791474E-5));
#38051=CARTESIAN_POINT('',(213.190589891905,-4.37197391080243,-0.000112134234356298));
#38052=CARTESIAN_POINT('',(207.493410108095,-4.372,-3.09002298987926E-13));
#38053=CARTESIAN_POINT('Ctrl Pts',(212.993410108095,-4.37226510377645,7.52726507913769E-5));
#38054=CARTESIAN_POINT('Ctrl Pts',(213.016910018632,-4.37174339242606,-0.645346551482844));
#38055=CARTESIAN_POINT('Ctrl Pts',(213.066806452854,-4.06441348752009,-2.01622563803203));
#38056=CARTESIAN_POINT('Ctrl Pts',(213.143099410762,-2.685457954271,-3.68108247872997));
#38057=CARTESIAN_POINT('Ctrl Pts',(213.22228898182,-0.602915682492534,-4.51647487750953));
#38058=CARTESIAN_POINT('Ctrl Pts',(213.301478552877,1.62583553009629,-4.25660797683398));
#38059=CARTESIAN_POINT('Ctrl Pts',(213.380668123935,3.46031653593829,-2.96450031379357));
#38060=CARTESIAN_POINT('Ctrl Pts',(213.459857694992,4.45565994712272,-0.953492042429545));
#38061=CARTESIAN_POINT('Ctrl Pts',(213.53904726605,4.37049186989017,1.28874103472886));
#38062=CARTESIAN_POINT('Ctrl Pts',(213.618236837108,3.22546582964164,3.21845037575295));
#38063=CARTESIAN_POINT('Ctrl Pts',(213.697426408165,1.29825422636,4.36767542327822));
#38064=CARTESIAN_POINT('Ctrl Pts',(213.776615979223,-0.943788091813559,
4.45772550490954));
#38065=CARTESIAN_POINT('Ctrl Pts',(213.85580555028,-2.9569588426014,3.46676319389305));
#38066=CARTESIAN_POINT('Ctrl Pts',(213.928070259904,-4.13971832299312,1.79527273839626));
#38067=CARTESIAN_POINT('Ctrl Pts',(213.973938445843,-4.37140933548667,0.534792057890676));
#38068=CARTESIAN_POINT('Ctrl Pts',(213.993410108095,-4.37193445885121,-0.00011114643995053));
#38069=CARTESIAN_POINT('Ctrl Pts',(213.190589891905,-4.37197391080243,-0.000112134234356263));
#38070=CARTESIAN_POINT('Ctrl Pts',(213.197045798807,-4.37215244790249,-0.177456814333501));
#38071=CARTESIAN_POINT('Ctrl Pts',(213.229898229396,-4.31827393176692,-1.079809973257));
#38072=CARTESIAN_POINT('Ctrl Pts',(213.28914718367,-3.71044411132438,-2.6447414261376));
#38073=CARTESIAN_POINT('Ctrl Pts',(213.368336754727,-1.99825093901252,-4.09500255178501));
#38074=CARTESIAN_POINT('Ctrl Pts',(213.447526325785,0.198524342788504,-4.55221273664913));
#38075=CARTESIAN_POINT('Ctrl Pts',(213.526715896842,2.34715684985826,-3.90549707931699));
#38076=CARTESIAN_POINT('Ctrl Pts',(213.6059054679,3.92659647158984,-2.31168615164089));
#38077=CARTESIAN_POINT('Ctrl Pts',(213.685095038957,4.55382415428641,-0.157284094007629));
#38078=CARTESIAN_POINT('Ctrl Pts',(213.764284610015,4.07673522096414,2.03525984889906));
#38079=CARTESIAN_POINT('Ctrl Pts',(213.843474181072,2.61102523177998,3.7342469057895));
#38080=CARTESIAN_POINT('Ctrl Pts',(213.92266375213,0.512133448436073,4.5276673956225));
#38081=CARTESIAN_POINT('Ctrl Pts',(214.001853323188,-1.71095229970873,4.22311436531282));
#38082=CARTESIAN_POINT('Ctrl Pts',(214.081042894245,-3.51912675796424,2.89444287830494));
#38083=CARTESIAN_POINT('Ctrl Pts',(214.143955083818,-4.27764833622274,1.28124536185332));
#38084=CARTESIAN_POINT('Ctrl Pts',(214.180470749704,-4.3718784963291,0.278093761091111));
#38085=CARTESIAN_POINT('Ctrl Pts',(214.190589891905,-4.3717143632787,7.21197504059343E-5));
#38086=CARTESIAN_POINT('Origin',(207.493410108095,0.,0.));
#38087=CARTESIAN_POINT('',(211.993410108095,-4.37163704855645,1.21582882285062E-5));
#38088=CARTESIAN_POINT('',(212.190589891905,-4.37223174941664,8.43980496761931E-5));
#38089=CARTESIAN_POINT('',(207.493410108095,-4.372,-3.09002298987926E-13));
#38090=CARTESIAN_POINT('Ctrl Pts',(211.993410108095,-4.37163704855645,1.21582882286683E-5));
#38091=CARTESIAN_POINT('Ctrl Pts',(212.007088544049,-4.37160047135746,-0.375819472462299));
#38092=CARTESIAN_POINT('Ctrl Pts',(212.047163503689,-4.23106483712903,-1.47695448277203));
#38093=CARTESIAN_POINT('Ctrl Pts',(212.113634987014,-3.31716382083363,-3.1238560826521));
#38094=CARTESIAN_POINT('Ctrl Pts',(212.192824558072,-1.42398215132184,-4.32831693295292));
#38095=CARTESIAN_POINT('Ctrl Pts',(212.272014129129,0.814519648555283,-4.48314737450014));
#38096=CARTESIAN_POINT('Ctrl Pts',(212.351203700187,2.85549788329282,-3.5508005404247));
#38097=CARTESIAN_POINT('Ctrl Pts',(212.430393271244,4.20400894040367,-1.75737345728678));
#38098=CARTESIAN_POINT('Ctrl Pts',(212.509582842302,4.53303466617831,0.462222191803663));
#38099=CARTESIAN_POINT('Ctrl Pts',(212.588772413359,3.76278529189487,2.56972751210507));
#38100=CARTESIAN_POINT('Ctrl Pts',(212.667961984417,2.08004870256613,4.05406586457634));
#38101=CARTESIAN_POINT('Ctrl Pts',(212.747151555475,-0.107106210032759,
4.55528055109042));
#38102=CARTESIAN_POINT('Ctrl Pts',(212.826341126532,-2.2682875313355,3.95182544080049));
#38103=CARTESIAN_POINT('Ctrl Pts',(212.90553069759,-3.87940202399173,2.39004028744685));
#38104=CARTESIAN_POINT('Ctrl Pts',(212.961220358111,-4.35082037023268,0.884127586732209));
#38105=CARTESIAN_POINT('Ctrl Pts',(212.990513494946,-4.37232941023223,0.0796303560494513));
#38106=CARTESIAN_POINT('Ctrl Pts',(212.993410108095,-4.37226510377645,7.52726507913769E-5));
#38107=CARTESIAN_POINT('Ctrl Pts',(212.190589891905,-4.37223174941664,8.43980496762972E-5));
#38108=CARTESIAN_POINT('Ctrl Pts',(212.21362084791,-4.37167547872142,-0.632471629830828));
#38109=CARTESIAN_POINT('Ctrl Pts',(212.263048327602,-4.07369174834855,-1.99052761130526));
#38110=CARTESIAN_POINT('Ctrl Pts',(212.338872330979,-2.71789185781366,-3.65720064579733));
#38111=CARTESIAN_POINT('Ctrl Pts',(212.418061902036,-0.642815370532352,
-4.51096897725948));
#38112=CARTESIAN_POINT('Ctrl Pts',(212.497251473094,1.58814585683998,-4.27081320731686));
#38113=CARTESIAN_POINT('Ctrl Pts',(212.576441044152,3.43397674124133,-2.99497186213889));
#38114=CARTESIAN_POINT('Ctrl Pts',(212.655630615209,4.44705751367238,-0.992840462753262));
#38115=CARTESIAN_POINT('Ctrl Pts',(212.734820186267,4.38171291473348,1.25005785756018));
#38116=CARTESIAN_POINT('Ctrl Pts',(212.814009757324,3.25378921426957,3.18981323332466));
#38117=CARTESIAN_POINT('Ctrl Pts',(212.893199328382,1.33681144131616,4.35602891229573));
#38118=CARTESIAN_POINT('Ctrl Pts',(212.972388899439,-0.904347291883607,
4.46589394075284));
#38119=CARTESIAN_POINT('Ctrl Pts',(213.051578470497,-2.92619897517484,3.4927657052937));
#38120=CARTESIAN_POINT('Ctrl Pts',(213.124312134652,-4.13145831734779,1.82101681823968));
#38121=CARTESIAN_POINT('Ctrl Pts',(213.170649275122,-4.37142245615048,0.547659442705151));
#38122=CARTESIAN_POINT('Ctrl Pts',(213.190589891905,-4.37197391080243,-0.000112134234356263));
#38123=CARTESIAN_POINT('Origin',(207.493410108095,0.,0.));
#38124=CARTESIAN_POINT('',(210.993410108095,-4.37219407540291,-9.26783309010704E-5));
#38125=CARTESIAN_POINT('',(211.190589891905,-4.37163507512868,2.84626229390961E-7));
#38126=CARTESIAN_POINT('',(207.493410108095,-4.372,-3.09002298987926E-13));
#38127=CARTESIAN_POINT('Ctrl Pts',(210.993410108095,-4.37219407540291,-9.26783309011282E-5));
#38128=CARTESIAN_POINT('Ctrl Pts',(210.997267069466,-4.37229343375423,-0.106028573797621));
#38129=CARTESIAN_POINT('Ctrl Pts',(211.027520554523,-4.3427019859007,-0.936920061828269));
#38130=CARTESIAN_POINT('Ctrl Pts',(211.084170563266,-3.83550395069923,-2.45987033873152));
#38131=CARTESIAN_POINT('Ctrl Pts',(211.163360134324,-2.19638331619705,-3.99223658715306));
#38132=CARTESIAN_POINT('Ctrl Pts',(211.242549705381,-0.0246328503458637,
-4.55647296294042));
#38133=CARTESIAN_POINT('Ctrl Pts',(211.321739276439,2.1530911588358,-4.01575037833895));
#38134=CARTESIAN_POINT('Ctrl Pts',(211.400928847496,3.80868382039997,-2.501195753153));
#38135=CARTESIAN_POINT('Ctrl Pts',(211.480118418554,4.54065873004066,-0.380093326269416));
#38136=CARTESIAN_POINT('Ctrl Pts',(211.559307989612,4.17150968026545,1.83318292235754));
#38137=CARTESIAN_POINT('Ctrl Pts',(211.638497560669,2.79075647149654,3.60190657238208));
#38138=CARTESIAN_POINT('Ctrl Pts',(211.717687131727,0.733236080175323,4.4971566005755));
#38139=CARTESIAN_POINT('Ctrl Pts',(211.796876702784,-1.50209635644419,4.30183207195806));
#38140=CARTESIAN_POINT('Ctrl Pts',(211.876066273842,-3.37316572337063,3.06329979630588));
#38141=CARTESIAN_POINT('Ctrl Pts',(211.941577408945,-4.24433544629584,1.42415411441826));
#38142=CARTESIAN_POINT('Ctrl Pts',(211.980692020363,-4.3716710577098,0.349457055968407));
#38143=CARTESIAN_POINT('Ctrl Pts',(211.993410108095,-4.37163704855645,1.21582882286683E-5));
#38144=CARTESIAN_POINT('Ctrl Pts',(211.190589891905,-4.37163507512868,2.84626229390961E-7));
#38145=CARTESIAN_POINT('Ctrl Pts',(211.203799373328,-4.37163424866656,-0.36294672243026));
#38146=CARTESIAN_POINT('Ctrl Pts',(211.243405378436,-4.23761044520356,-1.45117179924369));
#38147=CARTESIAN_POINT('Ctrl Pts',(211.309407907231,-3.34464745971568,-3.09441207414373));
#38148=CARTESIAN_POINT('Ctrl Pts',(211.388597478288,-1.46218654627958,-4.31556059142606));
#38149=CARTESIAN_POINT('Ctrl Pts',(211.467787049346,0.774859182922043,-4.49017215271657));
#38150=CARTESIAN_POINT('Ctrl Pts',(211.546976620403,2.82399913408206,-3.57590290767156));
#38151=CARTESIAN_POINT('Ctrl Pts',(211.626166191461,4.18831045292564,-1.79446601090796));
#38152=CARTESIAN_POINT('Ctrl Pts',(211.705355762519,4.53694337280039,0.42213451220282));
#38153=CARTESIAN_POINT('Ctrl Pts',(211.784545333576,3.78535331902254,2.53636609434741));
#38154=CARTESIAN_POINT('Ctrl Pts',(211.863734904634,2.11580323295756,4.03552095692693));
#38155=CARTESIAN_POINT('Ctrl Pts',(211.942924475691,-0.0668357619494714,
4.55604935172072));
#38156=CARTESIAN_POINT('Ctrl Pts',(212.022114046749,-2.23326687531246,3.97172151315046));
#38157=CARTESIAN_POINT('Ctrl Pts',(212.101303617806,-3.85812377876869,2.42423877167448));
#38158=CARTESIAN_POINT('Ctrl Pts',(212.157462232858,-4.34691686173918,0.909906504712177));
#38159=CARTESIAN_POINT('Ctrl Pts',(212.187224324225,-4.37231303855952,0.0925212957176837));
#38160=CARTESIAN_POINT('Ctrl Pts',(212.190589891905,-4.37223174941664,8.43980496762972E-5));
#38161=CARTESIAN_POINT('Origin',(207.493410108095,0.,0.));
#38162=CARTESIAN_POINT('',(209.993410108095,-4.37201596611874,0.000111980929712991));
#38163=CARTESIAN_POINT('',(210.190589891905,-4.37223008469844,-8.48050595506078E-5));
#38164=CARTESIAN_POINT('',(207.493410108095,-4.372,-3.09002298987926E-13));
#38165=CARTESIAN_POINT('Ctrl Pts',(209.993410108095,-4.37201596611874,0.000111980929712943));
#38166=CARTESIAN_POINT('Ctrl Pts',(210.013842118569,-4.37144249704474,-0.561142687935352));
#38167=CARTESIAN_POINT('Ctrl Pts',(210.06067065273,-4.12266125418189,-1.84798782433965));
#38168=CARTESIAN_POINT('Ctrl Pts',(210.133895710575,-2.89372191923785,-3.5197193599864));
#38169=CARTESIAN_POINT('Ctrl Pts',(210.213085281633,-0.862943537879242,
-4.47407889498736));
#38170=CARTESIAN_POINT('Ctrl Pts',(210.29227485269,1.37710147802978,-4.3434598905811));
#38171=CARTESIAN_POINT('Ctrl Pts',(210.371464423748,3.2831950149358,-3.15953845045613));
#38172=CARTESIAN_POINT('Ctrl Pts',(210.450653994806,4.39310350826522,-1.20941895478298));
#38173=CARTESIAN_POINT('Ctrl Pts',(210.529843565863,4.43767063245068,1.03398838263629));
#38174=CARTESIAN_POINT('Ctrl Pts',(210.609033136921,3.40608873948736,3.02665031932622));
#38175=CARTESIAN_POINT('Ctrl Pts',(210.688222707978,1.54851965941115,4.28534006751519));
#38176=CARTESIAN_POINT('Ctrl Pts',(210.767412279036,-0.68457028532424,4.50482143573546));
#38177=CARTESIAN_POINT('Ctrl Pts',(210.846601850094,-2.75164979303246,3.63186949857032));
#38178=CARTESIAN_POINT('Ctrl Pts',(210.92193445978,-4.08326796574857,1.9635921272198));
#38179=CARTESIAN_POINT('Ctrl Pts',(210.97087054578,-4.37161343859181,0.618982414065456));
#38180=CARTESIAN_POINT('Ctrl Pts',(210.993410108095,-4.37219407540291,-9.26783309011282E-5));
#38181=CARTESIAN_POINT('Ctrl Pts',(210.190589891905,-4.37223008469844,-8.48050595506078E-5));
#38182=CARTESIAN_POINT('Ctrl Pts',(210.193977898745,-4.37231219702262,-0.0931381070659649));
#38183=CARTESIAN_POINT('Ctrl Pts',(210.223762429271,-4.34672717194406,-0.9111400330763));
#38184=CARTESIAN_POINT('Ctrl Pts',(210.279943483483,-3.85709805879303,-2.425870420406));
#38185=CARTESIAN_POINT('Ctrl Pts',(210.35913305454,-2.23158676324473,-3.97266575777209));
#38186=CARTESIAN_POINT('Ctrl Pts',(210.438322625598,-0.0649086922827653,
-4.55607721401773));
#38187=CARTESIAN_POINT('Ctrl Pts',(210.517512196655,2.11750994076351,-4.0346256782917));
#38188=CARTESIAN_POINT('Ctrl Pts',(210.596701767713,3.7864257825248,-2.53476478355335));
#38189=CARTESIAN_POINT('Ctrl Pts',(210.67589133877,4.53712151645643,-0.420215491706979));
#38190=CARTESIAN_POINT('Ctrl Pts',(210.755080909828,4.18755107623993,1.79623737242675));
#38191=CARTESIAN_POINT('Ctrl Pts',(210.834270480885,2.82248638832623,3.57709704959276));
#38192=CARTESIAN_POINT('Ctrl Pts',(210.913460051943,0.77295991365603,4.49049949184098));
#38193=CARTESIAN_POINT('Ctrl Pts',(210.992649623001,-1.46401176030129,4.31494174701186));
#38194=CARTESIAN_POINT('Ctrl Pts',(211.071839194058,-3.34595599838294,3.09299711788944));
#38195=CARTESIAN_POINT('Ctrl Pts',(211.137819283693,-4.23792051755099,1.44993808277174));
#38196=CARTESIAN_POINT('Ctrl Pts',(211.177402849642,-4.37163590018688,0.362330747734179));
#38197=CARTESIAN_POINT('Ctrl Pts',(211.190589891905,-4.37163507512868,2.84626229390961E-7));
#38198=CARTESIAN_POINT('Origin',(227.75,0.85,3.75));
#38199=CARTESIAN_POINT('',(227.6,0.699999999999996,-6.96491205974634));
#38200=CARTESIAN_POINT('',(228.,1.1,-6.50768776140958));
#38201=CARTESIAN_POINT('Ctrl Pts',(227.6,0.69999999999998,-6.96491205974636));
#38202=CARTESIAN_POINT('Ctrl Pts',(227.806787469448,0.906787469447637,-6.73629991057805));
#38203=CARTESIAN_POINT('Ctrl Pts',(228.,1.09999999999999,-6.5076877614096));
#38204=CARTESIAN_POINT('',(228.,1.1,6.50768776140958));
#38205=CARTESIAN_POINT('',(228.,1.1,3.75));
#38206=CARTESIAN_POINT('',(227.6,0.699999999999996,6.96491205974634));
#38207=CARTESIAN_POINT('Ctrl Pts',(228.,1.09999999999999,6.5076877614096));
#38208=CARTESIAN_POINT('Ctrl Pts',(227.806787469448,0.906787469447637,6.73629991057805));
#38209=CARTESIAN_POINT('Ctrl Pts',(227.6,0.69999999999998,6.96491205974636));
#38210=CARTESIAN_POINT('',(227.5,0.6,6.97423830966508));
#38211=CARTESIAN_POINT('Origin',(226.9,0.,0.));
#38212=CARTESIAN_POINT('',(227.5,0.6,-6.97423830966508));
#38213=CARTESIAN_POINT('',(227.5,0.6,3.75));
#38214=CARTESIAN_POINT('Origin',(226.9,0.,0.));
#38215=CARTESIAN_POINT('Origin',(228.,0.,0.));
#38216=CARTESIAN_POINT('Origin',(228.,0.,0.));
#38217=CARTESIAN_POINT('Origin',(227.75,-0.85,-3.75));
#38218=CARTESIAN_POINT('',(227.6,-0.699999999999996,6.96491205974634));
#38219=CARTESIAN_POINT('',(228.,-1.1,6.50768776140958));
#38220=CARTESIAN_POINT('Ctrl Pts',(227.6,-0.69999999999998,6.96491205974636));
#38221=CARTESIAN_POINT('Ctrl Pts',(227.806787469448,-0.906787469447637,
6.73629991057805));
#38222=CARTESIAN_POINT('Ctrl Pts',(228.,-1.09999999999999,6.5076877614096));
#38223=CARTESIAN_POINT('',(228.,-1.1,-6.50768776140958));
#38224=CARTESIAN_POINT('',(228.,-1.1,-3.75));
#38225=CARTESIAN_POINT('',(227.6,-0.699999999999996,-6.96491205974634));
#38226=CARTESIAN_POINT('Ctrl Pts',(228.,-1.09999999999999,-6.5076877614096));
#38227=CARTESIAN_POINT('Ctrl Pts',(227.806787469448,-0.906787469447637,
-6.73629991057805));
#38228=CARTESIAN_POINT('Ctrl Pts',(227.6,-0.69999999999998,-6.96491205974636));
#38229=CARTESIAN_POINT('',(227.5,-0.6,-6.97423830966508));
#38230=CARTESIAN_POINT('Origin',(226.9,0.,0.));
#38231=CARTESIAN_POINT('',(227.5,-0.6,6.97423830966508));
#38232=CARTESIAN_POINT('',(227.5,-0.6,-3.75));
#38233=CARTESIAN_POINT('Origin',(226.9,0.,0.));
#38234=CARTESIAN_POINT('Origin',(225.,0.,0.));
#38235=CARTESIAN_POINT('Origin',(227.6,0.,0.));
#38236=CARTESIAN_POINT('',(226.2,0.6,-6.97423830966508));
#38237=CARTESIAN_POINT('',(225.,0.6,-6.97423830966508));
#38238=CARTESIAN_POINT('',(226.2,0.197221149720988,-6.99722114972099));
#38239=CARTESIAN_POINT('Origin',(226.2,0.,0.));
#38240=CARTESIAN_POINT('',(222.5,0.197221149720988,-6.99722114972099));
#38241=CARTESIAN_POINT('',(225.,0.197221149720988,-6.99722114972099));
#38242=CARTESIAN_POINT('',(222.5,-0.19722114972099,-6.99722114972099));
#38243=CARTESIAN_POINT('Origin',(222.5,0.,0.));
#38244=CARTESIAN_POINT('',(226.2,-0.19722114972099,-6.99722114972099));
#38245=CARTESIAN_POINT('',(225.,-0.19722114972099,-6.99722114972099));
#38246=CARTESIAN_POINT('',(226.2,-0.6,-6.97423830966508));
#38247=CARTESIAN_POINT('Origin',(226.2,0.,0.));
#38248=CARTESIAN_POINT('',(225.,-0.6,-6.97423830966508));
#38249=CARTESIAN_POINT('',(227.6,-7.,-8.57252759403147E-16));
#38250=CARTESIAN_POINT('Origin',(227.6,0.,0.));
#38251=CARTESIAN_POINT('',(227.5,-7.,-8.57252759403147E-16));
#38252=CARTESIAN_POINT('',(225.,-7.,-8.57252759403147E-16));
#38253=CARTESIAN_POINT('',(227.5,-6.99722114972099,-0.197221149720988));
#38254=CARTESIAN_POINT('Origin',(227.5,0.,0.));
#38255=CARTESIAN_POINT('',(222.5,-6.99722114972099,-0.197221149720988));
#38256=CARTESIAN_POINT('',(225.,-6.99722114972099,-0.197221149720988));
#38257=CARTESIAN_POINT('',(222.5,-7.,-8.57252759403147E-16));
#38258=CARTESIAN_POINT('Origin',(222.5,0.,0.));
#38259=CARTESIAN_POINT('',(222.4,-7.,-8.57252759403147E-16));
#38260=CARTESIAN_POINT('',(225.,-7.,-8.57252759403147E-16));
#38261=CARTESIAN_POINT('Origin',(222.4,0.,0.));
#38262=CARTESIAN_POINT('',(222.5,-6.99722114972099,0.19722114972099));
#38263=CARTESIAN_POINT('Origin',(222.5,0.,0.));
#38264=CARTESIAN_POINT('',(227.5,-6.99722114972099,0.19722114972099));
#38265=CARTESIAN_POINT('',(225.,-6.99722114972099,0.19722114972099));
#38266=CARTESIAN_POINT('Origin',(227.5,0.,0.));
#38267=CARTESIAN_POINT('Origin',(227.6,0.,0.));
#38268=CARTESIAN_POINT('',(226.2,-0.6,6.97423830966508));
#38269=CARTESIAN_POINT('',(225.,-0.6,6.97423830966508));
#38270=CARTESIAN_POINT('',(226.2,-0.197221149720991,6.99722114972099));
#38271=CARTESIAN_POINT('Origin',(226.2,0.,0.));
#38272=CARTESIAN_POINT('',(222.5,-0.197221149720991,6.99722114972099));
#38273=CARTESIAN_POINT('',(225.,-0.197221149720991,6.99722114972099));
#38274=CARTESIAN_POINT('',(222.5,0.197221149720991,6.99722114972099));
#38275=CARTESIAN_POINT('Origin',(222.5,0.,0.));
#38276=CARTESIAN_POINT('',(226.2,0.197221149720991,6.99722114972099));
#38277=CARTESIAN_POINT('',(225.,0.197221149720991,6.99722114972099));
#38278=CARTESIAN_POINT('',(226.2,0.6,6.97423830966508));
#38279=CARTESIAN_POINT('Origin',(226.2,0.,0.));
#38280=CARTESIAN_POINT('',(225.,0.6,6.97423830966508));
#38281=CARTESIAN_POINT('',(222.5,6.99722114972099,-0.19722114972099));
#38282=CARTESIAN_POINT('',(227.5,6.99722114972099,-0.19722114972099));
#38283=CARTESIAN_POINT('',(225.,6.99722114972099,-0.19722114972099));
#38284=CARTESIAN_POINT('',(227.5,6.99722114972099,0.197221149720991));
#38285=CARTESIAN_POINT('Origin',(227.5,0.,0.));
#38286=CARTESIAN_POINT('',(222.5,6.99722114972099,0.197221149720991));
#38287=CARTESIAN_POINT('',(225.,6.99722114972099,0.197221149720991));
#38288=CARTESIAN_POINT('Origin',(222.5,0.,0.));
#38289=CARTESIAN_POINT('',(222.5,6.8098412104164,1.62051309433602));
#38290=CARTESIAN_POINT('',(227.5,6.8098412104164,1.62051309433602));
#38291=CARTESIAN_POINT('',(225.,6.8098412104164,1.62051309433602));
#38292=CARTESIAN_POINT('',(227.5,6.70775203112678,2.00151509834788));
#38293=CARTESIAN_POINT('Origin',(227.5,0.,0.));
#38294=CARTESIAN_POINT('',(222.5,6.70775203112678,2.00151509834788));
#38295=CARTESIAN_POINT('',(225.,6.70775203112678,2.00151509834787));
#38296=CARTESIAN_POINT('Origin',(222.5,0.,0.));
#38297=CARTESIAN_POINT('',(222.5,6.15838184641663,3.32781204903854));
#38298=CARTESIAN_POINT('',(227.5,6.15838184641663,3.32781204903854));
#38299=CARTESIAN_POINT('',(225.,6.15838184641663,3.32781204903854));
#38300=CARTESIAN_POINT('',(227.5,5.96116069669564,3.66940910068244));
#38301=CARTESIAN_POINT('Origin',(227.5,0.,0.));
#38302=CARTESIAN_POINT('',(222.5,5.96116069669564,3.66940910068244));
#38303=CARTESIAN_POINT('',(225.,5.96116069669564,3.66940910068244));
#38304=CARTESIAN_POINT('Origin',(222.5,0.,0.));
#38305=CARTESIAN_POINT('',(222.5,5.08723893679076,4.80832611206852));
#38306=CARTESIAN_POINT('',(227.5,5.08723893679076,4.80832611206852));
#38307=CARTESIAN_POINT('',(225.,5.08723893679076,4.80832611206852));
#38308=CARTESIAN_POINT('',(227.5,4.80832611206852,5.08723893679076));
#38309=CARTESIAN_POINT('Origin',(227.5,0.,0.));
#38310=CARTESIAN_POINT('',(222.5,4.80832611206852,5.08723893679076));
#38311=CARTESIAN_POINT('',(225.,4.80832611206852,5.08723893679076));
#38312=CARTESIAN_POINT('Origin',(222.5,0.,0.));
#38313=CARTESIAN_POINT('',(222.5,3.66940910068245,5.96116069669564));
#38314=CARTESIAN_POINT('',(227.5,3.66940910068245,5.96116069669564));
#38315=CARTESIAN_POINT('',(225.,3.66940910068245,5.96116069669564));
#38316=CARTESIAN_POINT('',(227.5,3.32781204903854,6.15838184641663));
#38317=CARTESIAN_POINT('Origin',(227.5,0.,0.));
#38318=CARTESIAN_POINT('',(222.5,3.32781204903854,6.15838184641663));
#38319=CARTESIAN_POINT('',(225.,3.32781204903854,6.15838184641663));
#38320=CARTESIAN_POINT('Origin',(222.5,0.,0.));
#38321=CARTESIAN_POINT('',(222.5,2.00151509834788,6.70775203112678));
#38322=CARTESIAN_POINT('',(227.5,2.00151509834788,6.70775203112678));
#38323=CARTESIAN_POINT('',(225.,2.00151509834788,6.70775203112678));
#38324=CARTESIAN_POINT('',(227.5,1.62051309433602,6.8098412104164));
#38325=CARTESIAN_POINT('Origin',(227.5,0.,0.));
#38326=CARTESIAN_POINT('',(222.5,1.62051309433602,6.8098412104164));
#38327=CARTESIAN_POINT('',(225.,1.62051309433602,6.8098412104164));
#38328=CARTESIAN_POINT('Origin',(222.5,0.,0.));
#38329=CARTESIAN_POINT('',(222.5,-1.62051309433602,6.8098412104164));
#38330=CARTESIAN_POINT('',(227.5,-1.62051309433602,6.8098412104164));
#38331=CARTESIAN_POINT('',(225.,-1.62051309433602,6.8098412104164));
#38332=CARTESIAN_POINT('',(227.5,-2.00151509834787,6.70775203112678));
#38333=CARTESIAN_POINT('Origin',(227.5,0.,0.));
#38334=CARTESIAN_POINT('',(222.5,-2.00151509834787,6.70775203112678));
#38335=CARTESIAN_POINT('',(225.,-2.00151509834787,6.70775203112678));
#38336=CARTESIAN_POINT('Origin',(222.5,0.,0.));
#38337=CARTESIAN_POINT('',(222.5,-3.32781204903854,6.15838184641663));
#38338=CARTESIAN_POINT('',(227.5,-3.32781204903854,6.15838184641663));
#38339=CARTESIAN_POINT('',(225.,-3.32781204903854,6.15838184641663));
#38340=CARTESIAN_POINT('',(227.5,-3.66940910068244,5.96116069669564));
#38341=CARTESIAN_POINT('Origin',(227.5,0.,0.));
#38342=CARTESIAN_POINT('',(222.5,-3.66940910068244,5.96116069669564));
#38343=CARTESIAN_POINT('',(225.,-3.66940910068244,5.96116069669564));
#38344=CARTESIAN_POINT('Origin',(222.5,0.,0.));
#38345=CARTESIAN_POINT('',(222.5,-4.80832611206852,5.08723893679076));
#38346=CARTESIAN_POINT('',(227.5,-4.80832611206852,5.08723893679076));
#38347=CARTESIAN_POINT('',(225.,-4.80832611206852,5.08723893679076));
#38348=CARTESIAN_POINT('',(227.5,-5.08723893679076,4.80832611206852));
#38349=CARTESIAN_POINT('Origin',(227.5,0.,0.));
#38350=CARTESIAN_POINT('',(222.5,-5.08723893679076,4.80832611206852));
#38351=CARTESIAN_POINT('',(225.,-5.08723893679076,4.80832611206852));
#38352=CARTESIAN_POINT('Origin',(222.5,0.,0.));
#38353=CARTESIAN_POINT('',(222.5,-5.96116069669564,3.66940910068245));
#38354=CARTESIAN_POINT('',(227.5,-5.96116069669564,3.66940910068245));
#38355=CARTESIAN_POINT('',(225.,-5.96116069669564,3.66940910068245));
#38356=CARTESIAN_POINT('',(227.5,-6.15838184641663,3.32781204903855));
#38357=CARTESIAN_POINT('Origin',(227.5,0.,0.));
#38358=CARTESIAN_POINT('',(222.5,-6.15838184641663,3.32781204903855));
#38359=CARTESIAN_POINT('',(225.,-6.15838184641663,3.32781204903855));
#38360=CARTESIAN_POINT('Origin',(222.5,0.,0.));
#38361=CARTESIAN_POINT('',(222.5,-6.70775203112678,2.00151509834788));
#38362=CARTESIAN_POINT('',(227.5,-6.70775203112678,2.00151509834788));
#38363=CARTESIAN_POINT('',(225.,-6.70775203112678,2.00151509834788));
#38364=CARTESIAN_POINT('',(227.5,-6.8098412104164,1.62051309433602));
#38365=CARTESIAN_POINT('Origin',(227.5,0.,0.));
#38366=CARTESIAN_POINT('',(222.5,-6.8098412104164,1.62051309433602));
#38367=CARTESIAN_POINT('',(225.,-6.8098412104164,1.62051309433602));
#38368=CARTESIAN_POINT('Origin',(222.5,0.,0.));
#38369=CARTESIAN_POINT('',(222.5,-6.8098412104164,-1.62051309433602));
#38370=CARTESIAN_POINT('',(227.5,-6.8098412104164,-1.62051309433602));
#38371=CARTESIAN_POINT('',(225.,-6.8098412104164,-1.62051309433602));
#38372=CARTESIAN_POINT('',(227.5,-6.70775203112678,-2.00151509834787));
#38373=CARTESIAN_POINT('Origin',(227.5,0.,0.));
#38374=CARTESIAN_POINT('',(222.5,-6.70775203112678,-2.00151509834787));
#38375=CARTESIAN_POINT('',(225.,-6.70775203112678,-2.00151509834787));
#38376=CARTESIAN_POINT('Origin',(222.5,0.,0.));
#38377=CARTESIAN_POINT('',(222.5,-6.15838184641663,-3.32781204903854));
#38378=CARTESIAN_POINT('',(227.5,-6.15838184641663,-3.32781204903854));
#38379=CARTESIAN_POINT('',(225.,-6.15838184641663,-3.32781204903854));
#38380=CARTESIAN_POINT('',(227.5,-5.96116069669564,-3.66940910068244));
#38381=CARTESIAN_POINT('Origin',(227.5,0.,0.));
#38382=CARTESIAN_POINT('',(222.5,-5.96116069669564,-3.66940910068244));
#38383=CARTESIAN_POINT('',(225.,-5.96116069669564,-3.66940910068244));
#38384=CARTESIAN_POINT('Origin',(222.5,0.,0.));
#38385=CARTESIAN_POINT('',(222.5,-5.08723893679076,-4.80832611206852));
#38386=CARTESIAN_POINT('',(227.5,-5.08723893679076,-4.80832611206852));
#38387=CARTESIAN_POINT('',(225.,-5.08723893679076,-4.80832611206852));
#38388=CARTESIAN_POINT('',(227.5,-4.80832611206853,-5.08723893679076));
#38389=CARTESIAN_POINT('Origin',(227.5,0.,0.));
#38390=CARTESIAN_POINT('',(222.5,-4.80832611206853,-5.08723893679076));
#38391=CARTESIAN_POINT('',(225.,-4.80832611206853,-5.08723893679076));
#38392=CARTESIAN_POINT('Origin',(222.5,0.,0.));
#38393=CARTESIAN_POINT('',(222.5,-3.66940910068245,-5.96116069669564));
#38394=CARTESIAN_POINT('',(227.5,-3.66940910068245,-5.96116069669564));
#38395=CARTESIAN_POINT('',(225.,-3.66940910068245,-5.96116069669564));
#38396=CARTESIAN_POINT('',(227.5,-3.32781204903855,-6.15838184641663));
#38397=CARTESIAN_POINT('Origin',(227.5,0.,0.));
#38398=CARTESIAN_POINT('',(222.5,-3.32781204903855,-6.15838184641663));
#38399=CARTESIAN_POINT('',(225.,-3.32781204903855,-6.15838184641663));
#38400=CARTESIAN_POINT('Origin',(222.5,0.,0.));
#38401=CARTESIAN_POINT('',(222.5,-2.00151509834788,-6.70775203112678));
#38402=CARTESIAN_POINT('',(227.5,-2.00151509834788,-6.70775203112678));
#38403=CARTESIAN_POINT('',(225.,-2.00151509834788,-6.70775203112678));
#38404=CARTESIAN_POINT('',(227.5,-1.62051309433603,-6.8098412104164));
#38405=CARTESIAN_POINT('Origin',(227.5,0.,0.));
#38406=CARTESIAN_POINT('',(222.5,-1.62051309433603,-6.8098412104164));
#38407=CARTESIAN_POINT('',(225.,-1.62051309433603,-6.8098412104164));
#38408=CARTESIAN_POINT('Origin',(222.5,0.,0.));
#38409=CARTESIAN_POINT('',(222.5,1.62051309433602,-6.8098412104164));
#38410=CARTESIAN_POINT('',(227.5,1.62051309433602,-6.8098412104164));
#38411=CARTESIAN_POINT('',(225.,1.62051309433602,-6.8098412104164));
#38412=CARTESIAN_POINT('',(227.5,2.00151509834787,-6.70775203112678));
#38413=CARTESIAN_POINT('Origin',(227.5,0.,0.));
#38414=CARTESIAN_POINT('',(222.5,2.00151509834787,-6.70775203112678));
#38415=CARTESIAN_POINT('',(225.,2.00151509834787,-6.70775203112678));
#38416=CARTESIAN_POINT('Origin',(222.5,0.,0.));
#38417=CARTESIAN_POINT('',(222.5,3.32781204903854,-6.15838184641663));
#38418=CARTESIAN_POINT('',(227.5,3.32781204903854,-6.15838184641663));
#38419=CARTESIAN_POINT('',(225.,3.32781204903854,-6.15838184641663));
#38420=CARTESIAN_POINT('',(227.5,3.66940910068244,-5.96116069669564));
#38421=CARTESIAN_POINT('Origin',(227.5,0.,0.));
#38422=CARTESIAN_POINT('',(222.5,3.66940910068244,-5.96116069669564));
#38423=CARTESIAN_POINT('',(225.,3.66940910068244,-5.96116069669564));
#38424=CARTESIAN_POINT('Origin',(222.5,0.,0.));
#38425=CARTESIAN_POINT('',(222.5,4.80832611206852,-5.08723893679076));
#38426=CARTESIAN_POINT('',(227.5,4.80832611206852,-5.08723893679076));
#38427=CARTESIAN_POINT('',(225.,4.80832611206852,-5.08723893679076));
#38428=CARTESIAN_POINT('',(227.5,5.08723893679076,-4.80832611206852));
#38429=CARTESIAN_POINT('Origin',(227.5,0.,0.));
#38430=CARTESIAN_POINT('',(222.5,5.08723893679076,-4.80832611206852));
#38431=CARTESIAN_POINT('',(225.,5.08723893679076,-4.80832611206852));
#38432=CARTESIAN_POINT('Origin',(222.5,0.,0.));
#38433=CARTESIAN_POINT('',(222.5,5.96116069669564,-3.66940910068245));
#38434=CARTESIAN_POINT('',(227.5,5.96116069669564,-3.66940910068245));
#38435=CARTESIAN_POINT('',(225.,5.96116069669564,-3.66940910068245));
#38436=CARTESIAN_POINT('',(227.5,6.15838184641663,-3.32781204903855));
#38437=CARTESIAN_POINT('Origin',(227.5,0.,0.));
#38438=CARTESIAN_POINT('',(222.5,6.15838184641663,-3.32781204903855));
#38439=CARTESIAN_POINT('',(225.,6.15838184641663,-3.32781204903855));
#38440=CARTESIAN_POINT('Origin',(222.5,0.,0.));
#38441=CARTESIAN_POINT('',(222.5,6.70775203112678,-2.00151509834788));
#38442=CARTESIAN_POINT('',(227.5,6.70775203112678,-2.00151509834788));
#38443=CARTESIAN_POINT('',(225.,6.70775203112678,-2.00151509834788));
#38444=CARTESIAN_POINT('',(227.5,6.8098412104164,-1.62051309433603));
#38445=CARTESIAN_POINT('Origin',(227.5,0.,0.));
#38446=CARTESIAN_POINT('',(222.5,6.8098412104164,-1.62051309433603));
#38447=CARTESIAN_POINT('',(225.,6.8098412104164,-1.62051309433603));
#38448=CARTESIAN_POINT('Origin',(222.5,0.,0.));
#38449=CARTESIAN_POINT('Origin',(227.8,0.,0.));
#38450=CARTESIAN_POINT('Origin',(228.,0.,0.));
#38451=CARTESIAN_POINT('Origin',(228.,0.,0.));
#38452=CARTESIAN_POINT('Ctrl Pts',(209.012910346562,-1.91898364243922,3.92834389788505));
#38453=CARTESIAN_POINT('Ctrl Pts',(209.039306870248,-2.57051617251472,3.61007230552139));
#38454=CARTESIAN_POINT('Ctrl Pts',(209.092099917619,-3.7114647271083,2.64329361995669));
#38455=CARTESIAN_POINT('Ctrl Pts',(209.171289488677,-4.52311191657194,0.551127705008165));
#38456=CARTESIAN_POINT('Ctrl Pts',(209.250479059734,-4.23771212707877,-1.67438902528095));
#38457=CARTESIAN_POINT('Ctrl Pts',(209.329668630792,-2.92472974788555,-3.4940198648462));
#38458=CARTESIAN_POINT('Ctrl Pts',(209.40885820185,-0.90245430475216,-4.4662682355186));
#38459=CARTESIAN_POINT('Ctrl Pts',(209.488047772907,1.33865191662591,-4.35546678832985));
#38460=CARTESIAN_POINT('Ctrl Pts',(209.567237343965,3.25513899273275,-3.1884349607263));
#38461=CARTESIAN_POINT('Ctrl Pts',(209.646426915022,4.38224084314362,-1.24820523943406));
#38462=CARTESIAN_POINT('Ctrl Pts',(209.72561648608,4.4466373711158,0.994721723380339));
#38463=CARTESIAN_POINT('Ctrl Pts',(209.804806057137,3.43270956435134,2.99642387551628));
#38464=CARTESIAN_POINT('Ctrl Pts',(209.883995628195,1.58633933997099,4.27148464599025));
#38465=CARTESIAN_POINT('Ctrl Pts',(209.963185199253,-0.644723329766792,
4.51069664301433));
#38466=CARTESIAN_POINT('Ctrl Pts',(210.04237477031,-2.71943848460081,3.6560507558529));
#38467=CARTESIAN_POINT('Ctrl Pts',(210.121564341368,-4.1346813337972,1.91480103026804));
#38468=CARTESIAN_POINT('Ctrl Pts',(210.200753912425,-4.54725099365243,-0.29079390175578));
#38469=CARTESIAN_POINT('Ctrl Pts',(210.279943483483,-3.85709805879303,-2.425870420406));
#38470=CARTESIAN_POINT('Ctrl Pts',(210.35913305454,-2.23158676324473,-3.97266575777209));
#38471=CARTESIAN_POINT('Ctrl Pts',(210.438322625598,-0.0649086922827653,
-4.55607721401773));
#38472=CARTESIAN_POINT('Ctrl Pts',(210.517512196655,2.11750994076351,-4.0346256782917));
#38473=CARTESIAN_POINT('Ctrl Pts',(210.596701767713,3.7864257825248,-2.53476478355335));
#38474=CARTESIAN_POINT('Ctrl Pts',(210.67589133877,4.53712151645643,-0.420215491706979));
#38475=CARTESIAN_POINT('Ctrl Pts',(210.755080909828,4.18755107623993,1.79623737242675));
#38476=CARTESIAN_POINT('Ctrl Pts',(210.834270480885,2.82248638832623,3.57709704959276));
#38477=CARTESIAN_POINT('Ctrl Pts',(210.913460051943,0.77295991365603,4.49049949184098));
#38478=CARTESIAN_POINT('Ctrl Pts',(210.992649623001,-1.46401176030129,4.31494174701186));
#38479=CARTESIAN_POINT('Ctrl Pts',(211.071839194058,-3.34595599838294,3.09299711788944));
#38480=CARTESIAN_POINT('Ctrl Pts',(211.151028765116,-4.41649543023929,1.12099100311488));
#38481=CARTESIAN_POINT('Ctrl Pts',(211.230218336173,-4.41602089165307,-1.12285893988305));
#38482=CARTESIAN_POINT('Ctrl Pts',(211.309407907231,-3.34464745971568,-3.09441207414373));
#38483=CARTESIAN_POINT('Ctrl Pts',(211.388597478288,-1.46218654627958,-4.31556059142606));
#38484=CARTESIAN_POINT('Ctrl Pts',(211.467787049346,0.774859182922043,-4.49017215271657));
#38485=CARTESIAN_POINT('Ctrl Pts',(211.546976620403,2.82399913408206,-3.57590290767156));
#38486=CARTESIAN_POINT('Ctrl Pts',(211.626166191461,4.18831045292564,-1.79446601090796));
#38487=CARTESIAN_POINT('Ctrl Pts',(211.705355762519,4.53694337280039,0.42213451220282));
#38488=CARTESIAN_POINT('Ctrl Pts',(211.784545333576,3.78535331902254,2.53636609434741));
#38489=CARTESIAN_POINT('Ctrl Pts',(211.863734904634,2.11580323295756,4.03552095692693));
#38490=CARTESIAN_POINT('Ctrl Pts',(211.942924475691,-0.0668357619494714,
4.55604935172072));
#38491=CARTESIAN_POINT('Ctrl Pts',(212.022114046749,-2.23326687531246,3.97172151315046));
#38492=CARTESIAN_POINT('Ctrl Pts',(212.101303617806,-3.85812377876869,2.42423877167448));
#38493=CARTESIAN_POINT('Ctrl Pts',(212.180493188864,-4.54737358559575,0.28887053746655));
#38494=CARTESIAN_POINT('Ctrl Pts',(212.259682759921,-4.133871059509,-1.91654970656751));
#38495=CARTESIAN_POINT('Ctrl Pts',(212.338872330979,-2.71789185781366,-3.65720064579733));
#38496=CARTESIAN_POINT('Ctrl Pts',(212.418061902036,-0.642815370532352,
-4.51096897725948));
#38497=CARTESIAN_POINT('Ctrl Pts',(212.497251473094,1.58814585683998,-4.27081320731686));
#38498=CARTESIAN_POINT('Ctrl Pts',(212.576441044152,3.43397674124133,-2.99497186213889));
#38499=CARTESIAN_POINT('Ctrl Pts',(212.655630615209,4.44705751367238,-0.992840462753262));
#38500=CARTESIAN_POINT('Ctrl Pts',(212.734820186267,4.38171291473348,1.25005785756018));
#38501=CARTESIAN_POINT('Ctrl Pts',(212.814009757324,3.25378921426957,3.18981323332466));
#38502=CARTESIAN_POINT('Ctrl Pts',(212.893199328382,1.33681144131616,4.35602891229573));
#38503=CARTESIAN_POINT('Ctrl Pts',(212.972388899439,-0.904347291883607,
4.46589394075284));
#38504=CARTESIAN_POINT('Ctrl Pts',(213.051578470497,-2.92619897517484,3.4927657052937));
#38505=CARTESIAN_POINT('Ctrl Pts',(213.130768041554,-4.23843824468386,1.67263085000584));
#38506=CARTESIAN_POINT('Ctrl Pts',(213.209957612612,-4.5228429687662,-0.553122223629014));
#38507=CARTESIAN_POINT('Ctrl Pts',(213.28914718367,-3.71044411132438,-2.6447414261376));
#38508=CARTESIAN_POINT('Ctrl Pts',(213.368336754727,-1.99825093901252,-4.09500255178501));
#38509=CARTESIAN_POINT('Ctrl Pts',(213.447526325785,0.198524342788504,-4.55221273664913));
#38510=CARTESIAN_POINT('Ctrl Pts',(213.526715896842,2.34715684985826,-3.90549707931699));
#38511=CARTESIAN_POINT('Ctrl Pts',(213.6059054679,3.92659647158984,-2.31168615164089));
#38512=CARTESIAN_POINT('Ctrl Pts',(213.685095038957,4.55382415428641,-0.157284094007629));
#38513=CARTESIAN_POINT('Ctrl Pts',(213.764284610015,4.07673522096414,2.03525984889906));
#38514=CARTESIAN_POINT('Ctrl Pts',(213.843474181072,2.61102523177998,3.7342469057895));
#38515=CARTESIAN_POINT('Ctrl Pts',(213.92266375213,0.512133448436073,4.5276673956225));
#38516=CARTESIAN_POINT('Ctrl Pts',(214.001853323188,-1.71095229970873,4.22311436531282));
#38517=CARTESIAN_POINT('Ctrl Pts',(214.081042894245,-3.51912675796424,2.89444287830494));
#38518=CARTESIAN_POINT('Ctrl Pts',(214.160232465302,-4.4739019585786,0.863859930438193));
#38519=CARTESIAN_POINT('Ctrl Pts',(214.23942203636,-4.34374192587985,-1.37621175541547));
#38520=CARTESIAN_POINT('Ctrl Pts',(214.318611607418,-3.16021087534511,-3.28254778148629));
#38521=CARTESIAN_POINT('Ctrl Pts',(214.397801178475,-1.21031879251578,-4.39285569247082));
#38522=CARTESIAN_POINT('Ctrl Pts',(214.476990749533,1.03307938716119,-4.43788234343958));
#38523=CARTESIAN_POINT('Ctrl Pts',(214.55618032059,3.02595258074822,-3.40670863054845));
#38524=CARTESIAN_POINT('Ctrl Pts',(214.635369891648,4.28502279886023,-1.54939740790998));
#38525=CARTESIAN_POINT('Ctrl Pts',(214.714559462705,4.50496157129557,0.683647537507614));
#38526=CARTESIAN_POINT('Ctrl Pts',(214.793749033763,3.63243305708234,2.75090581449194));
#38527=CARTESIAN_POINT('Ctrl Pts',(214.872938604821,1.87902815291533,4.15106081802492));
#38528=CARTESIAN_POINT('Ctrl Pts',(214.952128175878,-0.330046961810515,
4.54457057568587));
#38529=CARTESIAN_POINT('Ctrl Pts',(215.031317746936,-2.45908465487818,3.83600773911274));
#38530=CARTESIAN_POINT('Ctrl Pts',(215.110507317993,-3.99178661943011,2.19720101477514));
#38531=CARTESIAN_POINT('Ctrl Pts',(215.189696889051,-4.55646782997706,0.0255661646378894));
#38532=CARTESIAN_POINT('Ctrl Pts',(215.268886460108,-4.0161913248725,-2.15226856047496));
#38533=CARTESIAN_POINT('Ctrl Pts',(215.348076031166,-2.50197584827897,-3.8081714206452));
#38534=CARTESIAN_POINT('Ctrl Pts',(215.427265602223,-0.381023394472204,
-4.54058078743843));
#38535=CARTESIAN_POINT('Ctrl Pts',(215.506455173281,1.83232842552693,-4.17188509614013));
#38536=CARTESIAN_POINT('Ctrl Pts',(215.585644744338,3.60133486508171,-2.79149420632338));
#38537=CARTESIAN_POINT('Ctrl Pts',(215.664834315396,4.49700632361528,-0.734157230948736));
#38538=CARTESIAN_POINT('Ctrl Pts',(215.744023886454,4.30213966797164,1.50121517167094));
#38539=CARTESIAN_POINT('Ctrl Pts',(215.823213457511,3.06399067229672,3.3725381946642));
#38540=CARTESIAN_POINT('Ctrl Pts',(215.902403028569,1.08281434484414,4.42601014560404));
#38541=CARTESIAN_POINT('Ctrl Pts',(215.981592599626,-1.16094785166298,4.40616077783247));
#38542=CARTESIAN_POINT('Ctrl Pts',(216.060782170684,-3.12317655906599,3.31780362518501));
#38543=CARTESIAN_POINT('Ctrl Pts',(216.139971741741,-4.32802517183125,1.42486870496378));
#38544=CARTESIAN_POINT('Ctrl Pts',(216.219161312799,-4.48331412882848,-0.813601337656876));
#38545=CARTESIAN_POINT('Ctrl Pts',(216.298350883856,-3.55138537175629,-2.85477050840615));
#38546=CARTESIAN_POINT('Ctrl Pts',(216.377540454914,-1.75823454219255,-4.20364889221627));
#38547=CARTESIAN_POINT('Ctrl Pts',(216.456730025972,0.46129366910955,-4.53312925750298));
#38548=CARTESIAN_POINT('Ctrl Pts',(216.535919597029,2.56895672128326,-3.76331158403921));
#38549=CARTESIAN_POINT('Ctrl Pts',(216.615109168087,4.05363972481456,-2.08087906803723));
#38550=CARTESIAN_POINT('Ctrl Pts',(216.694298739144,4.55530240261518,0.106173137461614));
#38551=CARTESIAN_POINT('Ctrl Pts',(216.773488310202,3.95228998454865,2.26747802468437));
#38552=CARTESIAN_POINT('Ctrl Pts',(216.852677881259,2.39083487010492,3.87891239115818));
#38553=CARTESIAN_POINT('Ctrl Pts',(216.931867452317,0.249594813651761,4.5496983574066));
#38554=CARTESIAN_POINT('Ctrl Pts',(217.011057023374,-1.95217276662517,4.11716822629792));
#38555=CARTESIAN_POINT('Ctrl Pts',(217.090246594432,-3.68053233849351,2.68621190893303));
#38556=CARTESIAN_POINT('Ctrl Pts',(217.16943616549,-4.51635129406087,0.603840792779706));
#38557=CARTESIAN_POINT('Ctrl Pts',(217.248625736547,-4.2569409195464,-1.62496360632525));
#38558=CARTESIAN_POINT('Ctrl Pts',(217.327815307605,-2.96520904301682,-3.45970924292799));
#38559=CARTESIAN_POINT('Ctrl Pts',(217.407004878662,-0.954404689107857,
-4.45546455532968));
#38560=CARTESIAN_POINT('Ctrl Pts',(217.48619444972,1.28784579027261,-4.37075576243597));
#38561=CARTESIAN_POINT('Ctrl Pts',(217.565384020777,3.21778963310249,-3.22612501175764));
#38562=CARTESIAN_POINT('Ctrl Pts',(217.644573591835,4.36740941459516,-1.2991488443191));
#38563=CARTESIAN_POINT('Ctrl Pts',(217.723763162892,4.45791873813246,0.942874985667582));
#38564=CARTESIAN_POINT('Ctrl Pts',(217.80295273395,3.46736880936034,2.95624867936802));
#38565=CARTESIAN_POINT('Ctrl Pts',(217.882142305007,1.63597108754423,4.25272281192996));
#38566=CARTESIAN_POINT('Ctrl Pts',(217.961331876065,-0.592154745435518,
4.5178983467812));
#38567=CARTESIAN_POINT('Ctrl Pts',(218.040521447122,-2.6766811985351,3.68746938642191));
#38568=CARTESIAN_POINT('Ctrl Pts',(218.11971101818,-4.11210407995962,1.96281755391823));
#38569=CARTESIAN_POINT('Ctrl Pts',(218.198900589238,-4.55032884647146,-0.237823681242803));
#38570=CARTESIAN_POINT('Ctrl Pts',(218.278090160295,-3.88508462005382,-2.38079192904617));
#38571=CARTESIAN_POINT('Ctrl Pts',(218.357279731353,-2.27769520857755,-3.94641067949257));
#38572=CARTESIAN_POINT('Ctrl Pts',(218.43646930241,-0.117957577266953,-4.55501248344671));
#38573=CARTESIAN_POINT('Ctrl Pts',(218.515658873468,2.07038513587111,-4.05900949783985));
#38574=CARTESIAN_POINT('Ctrl Pts',(218.594848444525,3.75665297092044,-2.57868399973024));
#38575=CARTESIAN_POINT('Ctrl Pts',(218.674038015583,4.53192069796186,-0.473019557497457));
#38576=CARTESIAN_POINT('Ctrl Pts',(218.75322758664,4.20818346572563,1.74735360851304));
#38577=CARTESIAN_POINT('Ctrl Pts',(218.832417157698,2.86394856669164,3.54398805327205));
#38578=CARTESIAN_POINT('Ctrl Pts',(218.911606728756,0.825197172846602,4.48119429843385));
#38579=CARTESIAN_POINT('Ctrl Pts',(218.990796299813,-1.41366711921135,4.33169689503441));
#38580=CARTESIAN_POINT('Ctrl Pts',(219.069985870871,-3.30971270848846,3.13174943149354));
#38581=CARTESIAN_POINT('Ctrl Pts',(219.149175441928,-4.4031426028244,1.17234292490846));
#38582=CARTESIAN_POINT('Ctrl Pts',(219.228365012986,-4.42879662917418,-1.07136041172219));
#38583=CARTESIAN_POINT('Ctrl Pts',(219.307554584043,-3.38045360582197,-3.05525549394406));
#38584=CARTESIAN_POINT('Ctrl Pts',(219.386744155101,-1.51233999842644,-4.29824155248976));
#38585=CARTESIAN_POINT('Ctrl Pts',(219.465933726158,0.722520793916989,-4.49889057621407));
#38586=CARTESIAN_POINT('Ctrl Pts',(219.545123297216,2.78216803143074,-3.60854454860609));
#38587=CARTESIAN_POINT('Ctrl Pts',(219.624312868274,4.16713080999959,-1.84311516914782));
#38588=CARTESIAN_POINT('Ctrl Pts',(219.703502439331,4.5415513193251,0.369275409857588));
#38589=CARTESIAN_POINT('Ctrl Pts',(219.782692010389,3.81463141353823,2.49211554572396));
#38590=CARTESIAN_POINT('Ctrl Pts',(219.861881581446,2.16265144586963,4.01060985862089));
#38591=CARTESIAN_POINT('Ctrl Pts',(219.941071152504,-0.0137782689576099,
4.55651872307046));
#38592=CARTESIAN_POINT('Ctrl Pts',(220.020260723561,-2.1868667104261,3.99745753013543));
#38593=CARTESIAN_POINT('Ctrl Pts',(220.099450294619,-3.82963312724697,2.46900036959006));
#38594=CARTESIAN_POINT('Ctrl Pts',(220.178639865676,-4.54370151966309,0.34180288867031));
#38595=CARTESIAN_POINT('Ctrl Pts',(220.257829436734,-4.15590806660398,-1.86828286299391));
#38596=CARTESIAN_POINT('Ctrl Pts',(220.337019007791,-2.76029389481659,-3.62530417052153));
#38597=CARTESIAN_POINT('Ctrl Pts',(220.416208578849,-0.695299810488197,
-4.50317786546855));
#38598=CARTESIAN_POINT('Ctrl Pts',(220.495398149907,1.53830665449812,-4.28901682788606));
#38599=CARTESIAN_POINT('Ctrl Pts',(220.574587720964,3.39886894010639,-3.03475578035621));
#38600=CARTESIAN_POINT('Ctrl Pts',(220.653777292022,4.43519486338251,-1.044556953301));
#38601=CARTESIAN_POINT('Ctrl Pts',(220.732966863079,4.39597214951006,1.19895020433616));
#38602=CARTESIAN_POINT('Ctrl Pts',(220.812156434137,3.29071241572633,3.15170818597724));
#38603=CARTESIAN_POINT('Ctrl Pts',(220.891346005194,1.38744463724644,4.34016705855231));
#38604=CARTESIAN_POINT('Ctrl Pts',(220.970535576252,-0.852282851982811,
4.47612184162993));
#38605=CARTESIAN_POINT('Ctrl Pts',(221.049725147309,-2.88532899192737,3.52660303771061));
#38606=CARTESIAN_POINT('Ctrl Pts',(221.128914718367,-4.21867400611988,1.72187200818135));
#38607=CARTESIAN_POINT('Ctrl Pts',(221.208104289424,-4.52897696306373,-0.500418487859158));
#38608=CARTESIAN_POINT('Ctrl Pts',(221.287293860482,-3.7409896782648,-2.60135569353455));
#38609=CARTESIAN_POINT('Ctrl Pts',(221.36648343154,-2.04579887264011,-4.07145650839735));
#38610=CARTESIAN_POINT('Ctrl Pts',(221.445673002597,0.14550072168771,-4.5542152892435));
#38611=CARTESIAN_POINT('Ctrl Pts',(221.524862573655,2.30152409777985,-3.93256490416486));
#38612=CARTESIAN_POINT('Ctrl Pts',(221.604052144712,3.89940335283094,-2.35725035066262));
#38613=CARTESIAN_POINT('Ctrl Pts',(221.68324171577,4.55170192744695,-0.210305677009054));
#38614=CARTESIAN_POINT('Ctrl Pts',(221.762431286827,4.10012073214107,1.98766009715916));
#38615=CARTESIAN_POINT('Ctrl Pts',(221.841620857885,2.65441560822601,3.70356057542857));
#38616=CARTESIAN_POINT('Ctrl Pts',(221.920810428942,0.56466538392668,4.52140736785216));
#38617=CARTESIAN_POINT('Ctrl Pts',(221.973603476314,-0.919183673409389,
4.33535198326386));
#38618=CARTESIAN_POINT('Ctrl Pts',(222.,-1.59436307123039,4.07092009220235));
#38619=CARTESIAN_POINT('Ctrl Pts',(209.122606897708,-2.00237954638784,4.0990633262012));
#38620=CARTESIAN_POINT('Ctrl Pts',(209.149003421394,-2.6822266191702,3.76696016875312));
#38621=CARTESIAN_POINT('Ctrl Pts',(209.201796468765,-3.87275893986003,2.75816685595665));
#38622=CARTESIAN_POINT('Ctrl Pts',(209.280986039823,-4.71967899437356,0.575078817531406));
#38623=CARTESIAN_POINT('Ctrl Pts',(209.360175610881,-4.4218761948155,-1.74715524550129));
#38624=CARTESIAN_POINT('Ctrl Pts',(209.439365181938,-3.05183373967382,-3.64586427800282));
#38625=CARTESIAN_POINT('Ctrl Pts',(209.518554752996,-0.941673499148998,
-4.66036497951415));
#38626=CARTESIAN_POINT('Ctrl Pts',(209.597744324053,1.39682754886719,-4.54474828187575));
#38627=CARTESIAN_POINT('Ctrl Pts',(209.676933895111,3.39660203221564,-3.32699915160874));
#38628=CARTESIAN_POINT('Ctrl Pts',(209.756123466168,4.57268589350896,-1.30245020638111));
#38629=CARTESIAN_POINT('Ctrl Pts',(209.835313037226,4.63988098971415,1.03795070952906));
#38630=CARTESIAN_POINT('Ctrl Pts',(209.914502608283,3.58188953169507,3.12664357733423));
#38631=CARTESIAN_POINT('Ctrl Pts',(209.993692179341,1.65527906426069,4.45711641239878));
#38632=CARTESIAN_POINT('Ctrl Pts',(210.072881750399,-0.672741955717303,
4.70672417324597));
#38633=CARTESIAN_POINT('Ctrl Pts',(210.152071321456,-2.83762085241282,3.81493676765804));
#38634=CARTESIAN_POINT('Ctrl Pts',(210.231260892514,-4.31436785104821,1.99801516470331));
#38635=CARTESIAN_POINT('Ctrl Pts',(210.310450463571,-4.74486711643238,-0.303431331155035));
#38636=CARTESIAN_POINT('Ctrl Pts',(210.389640034629,-4.02472125896932,-2.53129479823699));
#38637=CARTESIAN_POINT('Ctrl Pts',(210.468829605686,-2.32856788973525,-4.14531134193876));
#38638=CARTESIAN_POINT('Ctrl Pts',(210.548019176744,-0.067729518342643,
-4.75407690996086));
#38639=CARTESIAN_POINT('Ctrl Pts',(210.627208747801,2.20953347432824,-4.20996393969962));
#38640=CARTESIAN_POINT('Ctrl Pts',(210.706398318859,3.95097768066745,-2.64492153306734));
#38641=CARTESIAN_POINT('Ctrl Pts',(210.785587889916,4.73429742865376,-0.43847737263662));
#38642=CARTESIAN_POINT('Ctrl Pts',(210.864777460974,4.36953522639674,1.87429892337849));
#38643=CARTESIAN_POINT('Ctrl Pts',(210.943967032032,2.94514705021599,3.73255186190351));
#38644=CARTESIAN_POINT('Ctrl Pts',(211.023156603089,0.806551492703307,4.6856492867746));
#38645=CARTESIAN_POINT('Ctrl Pts',(211.102346174147,-1.52763532719452,4.50246208825895));
#38646=CARTESIAN_POINT('Ctrl Pts',(211.181535745204,-3.49136579703178,3.22741373554704));
#38647=CARTESIAN_POINT('Ctrl Pts',(211.260725316262,-4.60842912917466,1.16970744652565));
#38648=CARTESIAN_POINT('Ctrl Pts',(211.339914887319,-4.60793396791431,-1.17165656078372));
#38649=CARTESIAN_POINT('Ctrl Pts',(211.419104458377,-3.49000039140507,-3.2288901834958));
#38650=CARTESIAN_POINT('Ctrl Pts',(211.498294029434,-1.5257307923439,-4.50310782664356));
#38651=CARTESIAN_POINT('Ctrl Pts',(211.577483600492,0.808533301118549,-4.68530772202493));
#38652=CARTESIAN_POINT('Ctrl Pts',(211.65667317155,2.94672553743877,-3.73130582451915));
#38653=CARTESIAN_POINT('Ctrl Pts',(211.735862742607,4.37032760435653,-1.87245058137286));
#38654=CARTESIAN_POINT('Ctrl Pts',(211.815052313665,4.73411154316455,0.440479790637971));
#38655=CARTESIAN_POINT('Ctrl Pts',(211.894241884722,3.94985860964796,2.64659243422069));
#38656=CARTESIAN_POINT('Ctrl Pts',(211.97343145578,2.20775259578052,4.21089812568633));
#38657=CARTESIAN_POINT('Ctrl Pts',(212.052621026837,-0.0697403353187167,
4.75404783681379));
#38658=CARTESIAN_POINT('Ctrl Pts',(212.131810597895,-2.33032101673728,4.14432606198363));
#38659=CARTESIAN_POINT('Ctrl Pts',(212.211000168953,-4.02579155506466,2.52959224070883));
#38660=CARTESIAN_POINT('Ctrl Pts',(212.29018974001,-4.74499503602191,0.30142438058611));
#38661=CARTESIAN_POINT('Ctrl Pts',(212.369379311067,-4.31352236355903,-1.99983983562693));
#38662=CARTESIAN_POINT('Ctrl Pts',(212.448568882125,-2.83600701174427,-3.81613662994679));
#38663=CARTESIAN_POINT('Ctrl Pts',(212.527758453182,-0.670751079681758,
-4.7070083426939));
#38664=CARTESIAN_POINT('Ctrl Pts',(212.60694802424,1.65716408941078,-4.45641579409413));
#38665=CARTESIAN_POINT('Ctrl Pts',(212.686137595298,3.58321177802902,-3.12512846182015));
#38666=CARTESIAN_POINT('Ctrl Pts',(212.765327166355,4.64031939098202,-1.03598769237887));
#38667=CARTESIAN_POINT('Ctrl Pts',(212.844516737413,4.57213502218987,1.3043833362739));
#38668=CARTESIAN_POINT('Ctrl Pts',(212.92370630847,3.39519359457865,3.32843732168963));
#38669=CARTESIAN_POINT('Ctrl Pts',(213.002895879528,1.3949070894978,4.54533483483374));
#38670=CARTESIAN_POINT('Ctrl Pts',(213.082085450586,-0.943648752418333,
4.65997441850743));
#38671=CARTESIAN_POINT('Ctrl Pts',(213.161275021643,-3.05336681718838,3.64455561471865));
#38672=CARTESIAN_POINT('Ctrl Pts',(213.240464592701,-4.42263386830918,1.74532066279202));
#38673=CARTESIAN_POINT('Ctrl Pts',(213.319654163758,-4.71939835853417,-0.577160014683326));
#38674=CARTESIAN_POINT('Ctrl Pts',(213.398843734816,-3.87169396977627,-2.75967758143634));
#38675=CARTESIAN_POINT('Ctrl Pts',(213.478033305873,-2.08509167057987,-4.27296469378847));
#38676=CARTESIAN_POINT('Ctrl Pts',(213.557222876931,0.207151887420196,-4.7500444886993));
#38677=CARTESIAN_POINT('Ctrl Pts',(213.636412447988,2.44916046410186,-4.07522362210525));
#38678=CARTESIAN_POINT('Ctrl Pts',(213.715602019046,4.09723995960495,-2.41214826710563));
#38679=CARTESIAN_POINT('Ctrl Pts',(213.794791590103,4.75172593592283,-0.164119404588944));
#38680=CARTESIAN_POINT('Ctrl Pts',(213.873981161161,4.25390349451931,2.12370892741937));
#38681=CARTESIAN_POINT('Ctrl Pts',(213.953170732219,2.72449613618031,3.8965311949249));
#38682=CARTESIAN_POINT('Ctrl Pts',(214.032360303276,0.534389934072604,4.72443244712485));
#38683=CARTESIAN_POINT('Ctrl Pts',(214.111549874334,-1.78530750029075,4.40664403809632));
#38684=CARTESIAN_POINT('Ctrl Pts',(214.190739445391,-3.67206227580806,3.02023065206477));
#38685=CARTESIAN_POINT('Ctrl Pts',(214.269929016449,-4.66833045174647,0.901401876180031));
#38686=CARTESIAN_POINT('Ctrl Pts',(214.349118587506,-4.53251387599815,-1.43601967708264));
#38687=CARTESIAN_POINT('Ctrl Pts',(214.428308158564,-3.29754849344109,-3.42520196229195));
#38688=CARTESIAN_POINT('Ctrl Pts',(214.507497729621,-1.26291727617956,-4.58376204690116));
#38689=CARTESIAN_POINT('Ctrl Pts',(214.586687300679,1.07797533491064,-4.63074548279309));
#38690=CARTESIAN_POINT('Ctrl Pts',(214.665876871737,3.15745555200671,-3.55475863965281));
#38691=CARTESIAN_POINT('Ctrl Pts',(214.745066442794,4.47124291134501,-1.61673169599391));
#38692=CARTESIAN_POINT('Ctrl Pts',(214.824256013852,4.70073986465014,0.713357746136703));
#38693=CARTESIAN_POINT('Ctrl Pts',(214.903445584909,3.79029268216141,2.87045570121504));
#38694=CARTESIAN_POINT('Ctrl Pts',(214.982635155967,1.9606876563586,4.33145916098574));
#38695=CARTESIAN_POINT('Ctrl Pts',(215.061824727024,-0.344390265274361,
4.74207021186618));
#38696=CARTESIAN_POINT('Ctrl Pts',(215.141014298082,-2.56595246924845,4.00271438834225));
#38697=CARTESIAN_POINT('Ctrl Pts',(215.220203869139,-4.16526316510524,2.29268779263592));
#38698=CARTESIAN_POINT('Ctrl Pts',(215.299393440197,-4.75448450145365,0.0266772285174098));
#38699=CARTESIAN_POINT('Ctrl Pts',(215.378583011254,-4.19072845930201,-2.24580264704637));
#38700=CARTESIAN_POINT('Ctrl Pts',(215.457772582312,-2.61070764406421,-3.9736683488068));
#38701=CARTESIAN_POINT('Ctrl Pts',(215.536962153369,-0.397582050682125,
-4.73790703391906));
#38702=CARTESIAN_POINT('Ctrl Pts',(215.616151724427,1.91195843487049,-4.35318842831457));
#38703=CARTESIAN_POINT('Ctrl Pts',(215.695341295484,3.75784301338123,-2.91280799845547));
#38704=CARTESIAN_POINT('Ctrl Pts',(215.774530866542,4.69243889486114,-0.766062508597483));
#38705=CARTESIAN_POINT('Ctrl Pts',(215.8537204376,4.48910365171241,1.56645553823485));
#38706=CARTESIAN_POINT('Ctrl Pts',(215.932910008657,3.19714671706717,3.51910321227311));
#38707=CARTESIAN_POINT('Ctrl Pts',(216.012099579715,1.12987169285888,4.61835733857402));
#38708=CARTESIAN_POINT('Ctrl Pts',(216.091289150772,-1.21140075464009,4.5976453496047));
#38709=CARTESIAN_POINT('Ctrl Pts',(216.17047872183,-3.25890472608852,3.4619899675421));
#38710=CARTESIAN_POINT('Ctrl Pts',(216.249668292887,-4.51611409741403,1.4867911784183));
#38711=CARTESIAN_POINT('Ctrl Pts',(216.328857863945,-4.67815165958727,-0.848959126804803));
#38712=CARTESIAN_POINT('Ctrl Pts',(216.408047435003,-3.70572279642092,-2.97883418557841));
#38713=CARTESIAN_POINT('Ctrl Pts',(216.48723700606,-1.83464455203167,-4.38633262723938));
#38714=CARTESIAN_POINT('Ctrl Pts',(216.566426577118,0.481340740731405,-4.73013167262777));
#38715=CARTESIAN_POINT('Ctrl Pts',(216.645616148175,2.68059939672786,-3.92685897675821));
#38716=CARTESIAN_POINT('Ctrl Pts',(216.724805719233,4.22980430571912,-2.17131068352834));
#38717=CARTESIAN_POINT('Ctrl Pts',(216.80399529029,4.75326842651658,0.110787249107921));
#38718=CARTESIAN_POINT('Ctrl Pts',(216.883184861348,4.12405007079391,2.36601892694649));
#38719=CARTESIAN_POINT('Ctrl Pts',(216.962374432405,2.49473665997683,4.04748360669341));
#38720=CARTESIAN_POINT('Ctrl Pts',(217.041564003463,0.260441797776623,4.74742083862966));
#38721=CARTESIAN_POINT('Ctrl Pts',(217.120753574521,-2.03701101586092,4.29609365241792));
#38722=CARTESIAN_POINT('Ctrl Pts',(217.199943145578,-3.84048228001083,2.80295030387752));
#38723=CARTESIAN_POINT('Ctrl Pts',(217.279132716635,-4.71262456621813,0.630082730251849));
#38724=CARTESIAN_POINT('Ctrl Pts',(217.358322287693,-4.44194063928881,-1.69558187832931));
#38725=CARTESIAN_POINT('Ctrl Pts',(217.437511858751,-3.09407219904913,-3.61006257233245));
#38726=CARTESIAN_POINT('Ctrl Pts',(217.516701429808,-0.995881562605238,
-4.6490917889785));
#38727=CARTESIAN_POINT('Ctrl Pts',(217.595891000865,1.34381347100266,-4.56070168989774));
#38728=CARTESIAN_POINT('Ctrl Pts',(217.675080571923,3.35762953024097,-3.36632715087795));
#38729=CARTESIAN_POINT('Ctrl Pts',(217.754270142981,4.55720991522943,-1.3556077373705));
#38730=CARTESIAN_POINT('Ctrl Pts',(217.833459714038,4.65165262656914,0.983850797030065));
#38731=CARTESIAN_POINT('Ctrl Pts',(217.912649285096,3.61805501104801,3.08472243258849));
#38732=CARTESIAN_POINT('Ctrl Pts',(217.991838856153,1.70706772675591,4.43753921958473));
#38733=CARTESIAN_POINT('Ctrl Pts',(218.071028427211,-0.61788882632131,4.71423885133025));
#38734=CARTESIAN_POINT('Ctrl Pts',(218.150217998268,-2.79300540432687,3.84772080074492));
#38735=CARTESIAN_POINT('Ctrl Pts',(218.229407569326,-4.29080942652693,2.04811840827425));
#38736=CARTESIAN_POINT('Ctrl Pts',(218.308597140384,-4.74807872772251,-0.248159111122965));
#38737=CARTESIAN_POINT('Ctrl Pts',(218.387786711441,-4.05392407060511,-2.48425726905503));
#38738=CARTESIAN_POINT('Ctrl Pts',(218.466976282499,-2.37668013301254,-4.11791526071479));
#38739=CARTESIAN_POINT('Ctrl Pts',(218.546165853556,-0.123083821475732,
-4.75296590793319));
#38740=CARTESIAN_POINT('Ctrl Pts',(218.625355424614,2.16036070216009,-4.23540744033519));
#38741=CARTESIAN_POINT('Ctrl Pts',(218.704544995671,3.91991099115714,-2.69074940685485));
#38742=CARTESIAN_POINT('Ctrl Pts',(218.783734566729,4.72887059105718,-0.493576217132539));
#38743=CARTESIAN_POINT('Ctrl Pts',(218.862924137786,4.39106426592872,1.82329075069452));
#38744=CARTESIAN_POINT('Ctrl Pts',(218.942113708844,2.98841110733013,3.6980040025222));
#38745=CARTESIAN_POINT('Ctrl Pts',(219.021303279902,0.861058898107562,4.67593970481593));
#38746=CARTESIAN_POINT('Ctrl Pts',(219.100492850959,-1.47510278999134,4.51994538772804));
#38747=CARTESIAN_POINT('Ctrl Pts',(219.179682422017,-3.45354743278232,3.26785016159048));
#38748=CARTESIAN_POINT('Ctrl Pts',(219.258871993074,-4.594496009626,1.22329103921145));
#38749=CARTESIAN_POINT('Ctrl Pts',(219.338061564132,-4.62126491818221,-1.11791999045667));
#38750=CARTESIAN_POINT('Ctrl Pts',(219.417251135189,-3.52736261430921,-3.18803192208892));
#38751=CARTESIAN_POINT('Ctrl Pts',(219.496440706247,-1.57806383184389,-4.48503613047993));
#38752=CARTESIAN_POINT('Ctrl Pts',(219.575630277304,0.753920370962774,-4.69440503400928));
#38753=CARTESIAN_POINT('Ctrl Pts',(219.654819848362,2.90307652319007,-3.76536601801031));
#38754=CARTESIAN_POINT('Ctrl Pts',(219.73400941942,4.34822752864093,-1.92321395280247));
#38755=CARTESIAN_POINT('Ctrl Pts',(219.813198990477,4.73891974354097,0.385323517788255));
#38756=CARTESIAN_POINT('Ctrl Pts',(219.892388561535,3.98040908247059,2.60041882881808));
#38757=CARTESIAN_POINT('Ctrl Pts',(219.971578132592,2.25663675573131,4.18490443161675));
#38758=CARTESIAN_POINT('Ctrl Pts',(220.05076770365,-0.0143770500879572,
4.75453760627801));
#38759=CARTESIAN_POINT('Ctrl Pts',(220.129957274707,-2.28190437624973,4.17118052435449));
#38760=CARTESIAN_POINT('Ctrl Pts',(220.209146845765,-3.99606274622613,2.57629910477353));
#38761=CARTESIAN_POINT('Ctrl Pts',(220.288336416822,-4.74116338808395,0.356657085570453));
#38762=CARTESIAN_POINT('Ctrl Pts',(220.36752598788,-4.33651706309409,-1.94947539363636));
#38763=CARTESIAN_POINT('Ctrl Pts',(220.446715558937,-2.88025177222171,-3.78285398580036));
#38764=CARTESIAN_POINT('Ctrl Pts',(220.525905129995,-0.725516407924797,
-4.69887864187271));
#38765=CARTESIAN_POINT('Ctrl Pts',(220.605094701053,1.60515895650054,-4.47541051436785));
#38766=CARTESIAN_POINT('Ctrl Pts',(220.68428427211,3.54657824903141,-3.16664132433328));
#38767=CARTESIAN_POINT('Ctrl Pts',(220.763473843168,4.62794120922941,-1.08995169738317));
#38768=CARTESIAN_POINT('Ctrl Pts',(220.842663414225,4.58701394008804,1.25105462767189));
#38769=CARTESIAN_POINT('Ctrl Pts',(220.921852985283,3.4337214182396,3.28867629104029));
#38770=CARTESIAN_POINT('Ctrl Pts',(221.00104255634,1.44774072166475,4.52878365075838));
#38771=CARTESIAN_POINT('Ctrl Pts',(221.080232127398,-0.889321676748745,
4.67064680730003));
#38772=CARTESIAN_POINT('Ctrl Pts',(221.159421698456,-3.01072069102759,3.67986346249677));
#38773=CARTESIAN_POINT('Ctrl Pts',(221.238611269513,-4.40201070812417,1.79670176151038));
#38774=CARTESIAN_POINT('Ctrl Pts',(221.317800840571,-4.72579892623439,-0.522165860387332));
#38775=CARTESIAN_POINT('Ctrl Pts',(221.396990411628,-3.90356699731108,-2.71440637554999));
#38776=CARTESIAN_POINT('Ctrl Pts',(221.476179982686,-2.13470595996895,-4.24839537770098));
#38777=CARTESIAN_POINT('Ctrl Pts',(221.555369553743,0.151823946097727,-4.75213406896817));
#38778=CARTESIAN_POINT('Ctrl Pts',(221.634559124801,2.40154458693313,-4.10346777053982));
#38779=CARTESIAN_POINT('Ctrl Pts',(221.713748695858,4.06886507219001,-2.45969261201348));
#38780=CARTESIAN_POINT('Ctrl Pts',(221.792938266916,4.74951148056106,-0.219445219239563));
#38781=CARTESIAN_POINT('Ctrl Pts',(221.872127837973,4.27830530192763,2.0740405679872));
#38782=CARTESIAN_POINT('Ctrl Pts',(221.951317409031,2.76977218772349,3.86451128662056));
#38783=CARTESIAN_POINT('Ctrl Pts',(222.030506980089,0.589204821928996,4.71790036874235));
#38784=CARTESIAN_POINT('Ctrl Pts',(222.08330002746,-0.959129898923508,4.52375932013947));
#38785=CARTESIAN_POINT('Ctrl Pts',(222.109696551146,-1.66365149381358,4.24783564973174));
#38786=CARTESIAN_POINT('Ctrl Pts',(209.232303448854,-2.08577545033647,4.26978275451734));
#38787=CARTESIAN_POINT('Ctrl Pts',(209.25869997254,-2.79393706582568,3.92384803198484));
#38788=CARTESIAN_POINT('Ctrl Pts',(209.311493019911,-4.03405315261176,2.8730400919566));
#38789=CARTESIAN_POINT('Ctrl Pts',(209.390682590969,-4.91624607217517,0.599029930054648));
#38790=CARTESIAN_POINT('Ctrl Pts',(209.469872162026,-4.60604026255224,-1.81992146572163));
#38791=CARTESIAN_POINT('Ctrl Pts',(209.549061733084,-3.17893773146209,-3.79770869115944));
#38792=CARTESIAN_POINT('Ctrl Pts',(209.628251304142,-0.980892693545834,
-4.8544617235097));
#38793=CARTESIAN_POINT('Ctrl Pts',(209.707440875199,1.45500318110846,-4.73402977542166));
#38794=CARTESIAN_POINT('Ctrl Pts',(209.786630446257,3.53806507169852,-3.46556334249118));
#38795=CARTESIAN_POINT('Ctrl Pts',(209.865820017314,4.7631309438743,-1.35669517332817));
#38796=CARTESIAN_POINT('Ctrl Pts',(209.945009588372,4.83312460831251,1.08117969567778));
#38797=CARTESIAN_POINT('Ctrl Pts',(210.024199159429,3.7310694990388,3.25686327915217));
#38798=CARTESIAN_POINT('Ctrl Pts',(210.103388730487,1.72421878855038,4.64274817880732));
#38799=CARTESIAN_POINT('Ctrl Pts',(210.182578301545,-0.700760581667812,
4.90275170347761));
#38800=CARTESIAN_POINT('Ctrl Pts',(210.261767872602,-2.95580322022483,3.97382277946319));
#38801=CARTESIAN_POINT('Ctrl Pts',(210.34095744366,-4.49405436829923,2.08122929913857));
#38802=CARTESIAN_POINT('Ctrl Pts',(210.420147014717,-4.94248323921234,-0.316068760554286));
#38803=CARTESIAN_POINT('Ctrl Pts',(210.499336585775,-4.1923444591456,-2.63671917606798));
#38804=CARTESIAN_POINT('Ctrl Pts',(210.578526156832,-2.42554901622577,-4.31795692610543));
#38805=CARTESIAN_POINT('Ctrl Pts',(210.65771572789,-0.0705503444025215,
-4.952076605904));
#38806=CARTESIAN_POINT('Ctrl Pts',(210.736905298947,2.30155700789298,-4.38530220110755));
#38807=CARTESIAN_POINT('Ctrl Pts',(210.816094870005,4.1155295788101,-2.75507828258134));
#38808=CARTESIAN_POINT('Ctrl Pts',(210.895284441063,4.93147334085109,-0.456739253566259));
#38809=CARTESIAN_POINT('Ctrl Pts',(210.97447401212,4.55151937655356,1.95236047433024));
#38810=CARTESIAN_POINT('Ctrl Pts',(211.053663583178,3.06780771210575,3.88800667421426));
#38811=CARTESIAN_POINT('Ctrl Pts',(211.132853154235,0.840143071750589,4.88079908170822));
#38812=CARTESIAN_POINT('Ctrl Pts',(211.212042725293,-1.59125889408775,4.68998242950604));
#38813=CARTESIAN_POINT('Ctrl Pts',(211.29123229635,-3.63677559568062,3.36183035320464));
#38814=CARTESIAN_POINT('Ctrl Pts',(211.370421867408,-4.80036282811003,1.21842388993642));
#38815=CARTESIAN_POINT('Ctrl Pts',(211.449611438465,-4.79984704417553,-1.22045418168439));
#38816=CARTESIAN_POINT('Ctrl Pts',(211.528801009523,-3.63535332309447,-3.36336829284788));
#38817=CARTESIAN_POINT('Ctrl Pts',(211.60799058058,-1.58927503840821,-4.69065506186107));
#38818=CARTESIAN_POINT('Ctrl Pts',(211.687180151638,0.842207419315057,-4.88044329133328));
#38819=CARTESIAN_POINT('Ctrl Pts',(211.766369722696,3.06945194079548,-3.88670874136673));
#38820=CARTESIAN_POINT('Ctrl Pts',(211.845559293753,4.55234475578742,-1.95043515183777));
#38821=CARTESIAN_POINT('Ctrl Pts',(211.924748864811,4.9312797135287,0.458825069073119));
#38822=CARTESIAN_POINT('Ctrl Pts',(212.003938435868,4.11436390027337,2.75681877409396));
#38823=CARTESIAN_POINT('Ctrl Pts',(212.083128006926,2.29970195860349,4.38627529444573));
#38824=CARTESIAN_POINT('Ctrl Pts',(212.162317577983,-0.0726449086879616,
4.95204632190687));
#38825=CARTESIAN_POINT('Ctrl Pts',(212.241507149041,-2.4273751581621,4.31693061081681));
#38826=CARTESIAN_POINT('Ctrl Pts',(212.320696720099,-4.19345933136064,2.63494570974319));
#38827=CARTESIAN_POINT('Ctrl Pts',(212.399886291156,-4.94261648644808,0.313978223705665));
#38828=CARTESIAN_POINT('Ctrl Pts',(212.479075862214,-4.49317366760906,-2.08312996468635));
#38829=CARTESIAN_POINT('Ctrl Pts',(212.558265433271,-2.95412216567489,-3.97507261409625));
#38830=CARTESIAN_POINT('Ctrl Pts',(212.637455004329,-0.698686788831166,
-4.90304770812833));
#38831=CARTESIAN_POINT('Ctrl Pts',(212.716644575386,1.72618232198158,-4.6420183808714));
#38832=CARTESIAN_POINT('Ctrl Pts',(212.795834146444,3.73244681481672,-3.2552850615014));
#38833=CARTESIAN_POINT('Ctrl Pts',(212.875023717501,4.83358126829166,-1.07913492200449));
#38834=CARTESIAN_POINT('Ctrl Pts',(212.954213288559,4.76255712964628,1.35870881498762));
#38835=CARTESIAN_POINT('Ctrl Pts',(213.033402859616,3.53659797488772,3.4670614100546));
#38836=CARTESIAN_POINT('Ctrl Pts',(213.112592430674,1.45300273767944,4.73464075737175));
#38837=CARTESIAN_POINT('Ctrl Pts',(213.191782001731,-0.982950212953061,
4.85405489626201));
#38838=CARTESIAN_POINT('Ctrl Pts',(213.270971572789,-3.18053465920191,3.79634552414359));
#38839=CARTESIAN_POINT('Ctrl Pts',(213.350161143847,-4.60682949193451,1.81801047557819));
#38840=CARTESIAN_POINT('Ctrl Pts',(213.429350714904,-4.91595374830214,-0.601197805737639));
#38841=CARTESIAN_POINT('Ctrl Pts',(213.508540285962,-4.03294382822817,-2.87461373673508));
#38842=CARTESIAN_POINT('Ctrl Pts',(213.587729857019,-2.17193240214721,-4.45092683579193));
#38843=CARTESIAN_POINT('Ctrl Pts',(213.666919428077,0.215779432051886,-4.94787624074946));
#38844=CARTESIAN_POINT('Ctrl Pts',(213.746108999134,2.55116407834546,-4.24495016489351));
#38845=CARTESIAN_POINT('Ctrl Pts',(213.825298570192,4.26788344762005,-2.51261038257036));
#38846=CARTESIAN_POINT('Ctrl Pts',(213.904488141249,4.94962771755924,-0.17095471517026));
#38847=CARTESIAN_POINT('Ctrl Pts',(213.983677712307,4.43107176807448,2.21215800593967));
#38848=CARTESIAN_POINT('Ctrl Pts',(214.062867283364,2.83796704058064,4.0588154840603));
#38849=CARTESIAN_POINT('Ctrl Pts',(214.142056854422,0.556646419709134,4.9211974986272));
#38850=CARTESIAN_POINT('Ctrl Pts',(214.22124642548,-1.85966270087277,4.59017371087982));
#38851=CARTESIAN_POINT('Ctrl Pts',(214.300435996537,-3.82499779365188,3.14601842582461));
#38852=CARTESIAN_POINT('Ctrl Pts',(214.379625567595,-4.86275894491434,0.938943821921869));
#38853=CARTESIAN_POINT('Ctrl Pts',(214.458815138652,-4.72128582611645,-1.49582759874982));
#38854=CARTESIAN_POINT('Ctrl Pts',(214.53800470971,-3.43488611153707,-3.56785614309761));
#38855=CARTESIAN_POINT('Ctrl Pts',(214.617194280767,-1.31551575984334,-4.7746684013315));
#38856=CARTESIAN_POINT('Ctrl Pts',(214.696383851825,1.12287128266008,-4.82360862214659));
#38857=CARTESIAN_POINT('Ctrl Pts',(214.775573422882,3.2889585232652,-3.70280864875716));
#38858=CARTESIAN_POINT('Ctrl Pts',(214.85476299394,4.65746302382978,-1.68406598407784));
#38859=CARTESIAN_POINT('Ctrl Pts',(214.933952564997,4.89651815800471,0.743067954765796));
#38860=CARTESIAN_POINT('Ctrl Pts',(215.013142136055,3.94815230724047,2.99000558793815));
#38861=CARTESIAN_POINT('Ctrl Pts',(215.092331707113,2.04234715980187,4.51185750394656));
#38862=CARTESIAN_POINT('Ctrl Pts',(215.17152127817,-0.358733568738209,4.93956984804649));
#38863=CARTESIAN_POINT('Ctrl Pts',(215.250710849228,-2.67282028361871,4.16942103757177));
#38864=CARTESIAN_POINT('Ctrl Pts',(215.329900420285,-4.33873971078038,2.3881745704967));
#38865=CARTESIAN_POINT('Ctrl Pts',(215.409089991343,-4.95250117293023,0.027788292396928));
#38866=CARTESIAN_POINT('Ctrl Pts',(215.4882795624,-4.36526559373151,-2.33933673361777));
#38867=CARTESIAN_POINT('Ctrl Pts',(215.567469133458,-2.71943943984944,-4.13916527696841));
#38868=CARTESIAN_POINT('Ctrl Pts',(215.646658704515,-0.414140706892048,
-4.93523328039969));
#38869=CARTESIAN_POINT('Ctrl Pts',(215.725848275573,1.99158844421406,-4.53449176048901));
#38870=CARTESIAN_POINT('Ctrl Pts',(215.805037846631,3.91435116168074,-3.03412179058756));
#38871=CARTESIAN_POINT('Ctrl Pts',(215.884227417688,4.887871466107,-0.797967786246231));
#38872=CARTESIAN_POINT('Ctrl Pts',(215.963416988746,4.67606763545317,1.63169590479877));
#38873=CARTESIAN_POINT('Ctrl Pts',(216.042606559803,3.33030276183762,3.66566822988202));
#38874=CARTESIAN_POINT('Ctrl Pts',(216.121796130861,1.17692904087363,4.810704531544));
#38875=CARTESIAN_POINT('Ctrl Pts',(216.200985701918,-1.2618536576172,4.78912992137693));
#38876=CARTESIAN_POINT('Ctrl Pts',(216.280175272976,-3.39463289311104,3.60617630989919));
#38877=CARTESIAN_POINT('Ctrl Pts',(216.359364844033,-4.70420302299682,1.54871365187283));
#38878=CARTESIAN_POINT('Ctrl Pts',(216.438554415091,-4.87298919034606,-0.884316915952731));
#38879=CARTESIAN_POINT('Ctrl Pts',(216.517743986149,-3.86006022108554,-3.10289786275067));
#38880=CARTESIAN_POINT('Ctrl Pts',(216.596933557206,-1.91105456187079,-4.5690163622625));
#38881=CARTESIAN_POINT('Ctrl Pts',(216.676123128264,0.50138781235326,-4.92713408775256));
#38882=CARTESIAN_POINT('Ctrl Pts',(216.755312699321,2.79224207217245,-4.09040636947721));
#38883=CARTESIAN_POINT('Ctrl Pts',(216.834502270379,4.40596888662368,-2.26174229901945));
#38884=CARTESIAN_POINT('Ctrl Pts',(216.913691841436,4.95123445041797,0.115401360754224));
#38885=CARTESIAN_POINT('Ctrl Pts',(216.992881412494,4.29581015703917,2.4645598292086));
#38886=CARTESIAN_POINT('Ctrl Pts',(217.072070983551,2.59863844984874,4.21605482222864));
#38887=CARTESIAN_POINT('Ctrl Pts',(217.151260554609,0.271288781901483,4.94514331985273));
#38888=CARTESIAN_POINT('Ctrl Pts',(217.230450125666,-2.12184926509668,4.47501907853792));
#38889=CARTESIAN_POINT('Ctrl Pts',(217.309639696724,-4.00043222152815,2.91968869882202));
#38890=CARTESIAN_POINT('Ctrl Pts',(217.388829267781,-4.90889783837539,0.656324667723989));
#38891=CARTESIAN_POINT('Ctrl Pts',(217.468018838839,-4.62694035903123,-1.76620015033337));
#38892=CARTESIAN_POINT('Ctrl Pts',(217.547208409896,-3.22293535508144,-3.7604159017369));
#38893=CARTESIAN_POINT('Ctrl Pts',(217.626397980954,-1.03735843610262,-4.84271902262731));
#38894=CARTESIAN_POINT('Ctrl Pts',(217.705587552012,1.39978115173269,-4.75064761735951));
#38895=CARTESIAN_POINT('Ctrl Pts',(217.784777123069,3.49746942737946,-3.50652928999826));
#38896=CARTESIAN_POINT('Ctrl Pts',(217.863966694127,4.74701041586371,-1.41206663042189));
#38897=CARTESIAN_POINT('Ctrl Pts',(217.943156265184,4.84538651500583,1.02482660839255));
#38898=CARTESIAN_POINT('Ctrl Pts',(218.022345836242,3.76874121273569,3.21319618580896));
#38899=CARTESIAN_POINT('Ctrl Pts',(218.101535407299,1.77816436596759,4.62235562723951));
#38900=CARTESIAN_POINT('Ctrl Pts',(218.180724978357,-0.643622907207105,
4.91057935587929));
#38901=CARTESIAN_POINT('Ctrl Pts',(218.259914549415,-2.90932961011864,4.00797221506793));
#38902=CARTESIAN_POINT('Ctrl Pts',(218.339104120472,-4.46951477309425,2.13341926263027));
#38903=CARTESIAN_POINT('Ctrl Pts',(218.41829369153,-4.94582860897356,-0.258494541003129));
#38904=CARTESIAN_POINT('Ctrl Pts',(218.497483262587,-4.22276352115641,-2.58772260906389));
#38905=CARTESIAN_POINT('Ctrl Pts',(218.576672833645,-2.47566505744753,-4.28941984193701));
#38906=CARTESIAN_POINT('Ctrl Pts',(218.655862404702,-0.12821006568451,-4.95091933241967));
#38907=CARTESIAN_POINT('Ctrl Pts',(218.73505197576,2.25033626844908,-4.41180538283052));
#38908=CARTESIAN_POINT('Ctrl Pts',(218.814241546818,4.08316901139384,-2.80281481397946));
#38909=CARTESIAN_POINT('Ctrl Pts',(218.893431117875,4.9258204841525,-0.514132876767619));
#38910=CARTESIAN_POINT('Ctrl Pts',(218.972620688933,4.5739450661318,1.899227892876));
#38911=CARTESIAN_POINT('Ctrl Pts',(219.05181025999,3.11287364796861,3.85201995177236));
#38912=CARTESIAN_POINT('Ctrl Pts',(219.130999831048,0.896920623368521,4.870685111198));
#38913=CARTESIAN_POINT('Ctrl Pts',(219.210189402105,-1.53653846077132,4.70819388042167));
#38914=CARTESIAN_POINT('Ctrl Pts',(219.289378973163,-3.59738215707619,3.40395089168742));
#38915=CARTESIAN_POINT('Ctrl Pts',(219.36856854422,-4.78584941642761,1.27423915351443));
#38916=CARTESIAN_POINT('Ctrl Pts',(219.447758115278,-4.81373320719024,-1.16447956919115));
#38917=CARTESIAN_POINT('Ctrl Pts',(219.526947686335,-3.67427162279645,-3.32080835023378));
#38918=CARTESIAN_POINT('Ctrl Pts',(219.606137257393,-1.64378766526134,-4.67183070847011));
#38919=CARTESIAN_POINT('Ctrl Pts',(219.68532682845,0.785319948008557,-4.8899194918045));
#38920=CARTESIAN_POINT('Ctrl Pts',(219.764516399508,3.0239850149494,-3.92218748741451));
#38921=CARTESIAN_POINT('Ctrl Pts',(219.843705970566,4.52932424728226,-2.00331273645713));
#38922=CARTESIAN_POINT('Ctrl Pts',(219.922895541623,4.93628816775683,0.401371625718925));
#38923=CARTESIAN_POINT('Ctrl Pts',(220.002085112681,4.14618675140296,2.7087221119122));
#38924=CARTESIAN_POINT('Ctrl Pts',(220.081274683738,2.35062206559299,4.35919900461263));
#38925=CARTESIAN_POINT('Ctrl Pts',(220.160464254796,-0.0149758312183077,
4.95255648948555));
#38926=CARTESIAN_POINT('Ctrl Pts',(220.239653825853,-2.37694204207336,4.34490351857356));
#38927=CARTESIAN_POINT('Ctrl Pts',(220.318843396911,-4.1624923652053,2.68359783995701));
#38928=CARTESIAN_POINT('Ctrl Pts',(220.398032967968,-4.93862525650481,0.371511282470593));
#38929=CARTESIAN_POINT('Ctrl Pts',(220.477222539026,-4.5171260595842,-2.03066792427881));
#38930=CARTESIAN_POINT('Ctrl Pts',(220.556412110083,-3.00020964962683,-3.94040380107919));
#38931=CARTESIAN_POINT('Ctrl Pts',(220.635601681141,-0.755733005361399,
-4.89457941827688));
#38932=CARTESIAN_POINT('Ctrl Pts',(220.714791252199,1.67201125850296,-4.66180420084963));
#38933=CARTESIAN_POINT('Ctrl Pts',(220.793980823256,3.69428755795643,-3.29852686831034));
#38934=CARTESIAN_POINT('Ctrl Pts',(220.873170394314,4.82068755507631,-1.13534644146534));
#38935=CARTESIAN_POINT('Ctrl Pts',(220.952359965371,4.77805573066601,1.30315905100762));
#38936=CARTESIAN_POINT('Ctrl Pts',(221.031549536429,3.57673042075288,3.42564439610333));
#38937=CARTESIAN_POINT('Ctrl Pts',(221.110739107487,1.50803680608307,4.71740024296444));
#38938=CARTESIAN_POINT('Ctrl Pts',(221.189928678544,-0.926360501514684,
4.86517177297014));
#38939=CARTESIAN_POINT('Ctrl Pts',(221.269118249601,-3.1361123901278,3.83312388728291));
#38940=CARTESIAN_POINT('Ctrl Pts',(221.348307820659,-4.58534741012846,1.87153151483941));
#38941=CARTESIAN_POINT('Ctrl Pts',(221.427497391717,-4.92262088940505,-0.543913232915508));
#38942=CARTESIAN_POINT('Ctrl Pts',(221.506686962774,-4.06614431635736,-2.82745705756544));
#38943=CARTESIAN_POINT('Ctrl Pts',(221.585876533832,-2.22361304729779,-4.42533424700461));
#38944=CARTESIAN_POINT('Ctrl Pts',(221.665066104889,0.158147170507748,-4.95005284869285));
#38945=CARTESIAN_POINT('Ctrl Pts',(221.744255675947,2.5015650760864,-4.27437063691479));
#38946=CARTESIAN_POINT('Ctrl Pts',(221.823445247004,4.23832679154908,-2.56213487336434));
#38947=CARTESIAN_POINT('Ctrl Pts',(221.902634818062,4.94732103367518,-0.22858476147007));
#38948=CARTESIAN_POINT('Ctrl Pts',(221.981824389119,4.45648987171418,2.16042103881523));
#38949=CARTESIAN_POINT('Ctrl Pts',(222.061013960177,2.88512876722097,4.02546199781256));
#38950=CARTESIAN_POINT('Ctrl Pts',(222.140203531234,0.613744259931314,4.91439336963254));
#38951=CARTESIAN_POINT('Ctrl Pts',(222.192996578606,-0.999076124437626,
4.71216665701508));
#38952=CARTESIAN_POINT('Ctrl Pts',(222.219393102292,-1.73293991639677,4.42475120726112));
#38953=CARTESIAN_POINT('Ctrl Pts',(209.342,-2.1691713542851,4.44050218283349));
#38954=CARTESIAN_POINT('Ctrl Pts',(209.368396523686,-2.90564751248116,4.08073589521657));
#38955=CARTESIAN_POINT('Ctrl Pts',(209.421189571058,-4.19534736536348,2.98791332795656));
#38956=CARTESIAN_POINT('Ctrl Pts',(209.500379142115,-5.11281314997678,0.62298104257789));
#38957=CARTESIAN_POINT('Ctrl Pts',(209.579568713173,-4.79020433028897,-1.89268768594197));
#38958=CARTESIAN_POINT('Ctrl Pts',(209.65875828423,-3.30604172325035,-3.94955310431605));
#38959=CARTESIAN_POINT('Ctrl Pts',(209.737947855288,-1.02011188794267,-5.04855846750524));
#38960=CARTESIAN_POINT('Ctrl Pts',(209.817137426345,1.51317881334974,-4.92331126896756));
#38961=CARTESIAN_POINT('Ctrl Pts',(209.896326997403,3.67952811118141,-3.60412753337363));
#38962=CARTESIAN_POINT('Ctrl Pts',(209.975516568461,4.95357599423964,-1.41094014027523));
#38963=CARTESIAN_POINT('Ctrl Pts',(210.054706139518,5.02636822691087,1.1244086818265));
#38964=CARTESIAN_POINT('Ctrl Pts',(210.133895710575,3.88024946638254,3.38708298097011));
#38965=CARTESIAN_POINT('Ctrl Pts',(210.213085281633,1.79315851284007,4.82837994521586));
#38966=CARTESIAN_POINT('Ctrl Pts',(210.292274852691,-0.728779207618322,
5.09877923370925));
#38967=CARTESIAN_POINT('Ctrl Pts',(210.371464423748,-3.07398558803684,4.13270879126833));
#38968=CARTESIAN_POINT('Ctrl Pts',(210.450653994806,-4.67374088555024,2.16444343357384));
#38969=CARTESIAN_POINT('Ctrl Pts',(210.529843565863,-5.1400993619923,-0.328706189953541));
#38970=CARTESIAN_POINT('Ctrl Pts',(210.609033136921,-4.35996765932188,-2.74214355389897));
#38971=CARTESIAN_POINT('Ctrl Pts',(210.688222707978,-2.52253014271629,-4.4906025102721));
#38972=CARTESIAN_POINT('Ctrl Pts',(210.767412279036,-0.0733711704623997,
-5.15007630184713));
#38973=CARTESIAN_POINT('Ctrl Pts',(210.846601850093,2.39358054145771,-4.56064046251547));
#38974=CARTESIAN_POINT('Ctrl Pts',(210.925791421151,4.28008147695276,-2.86523503209533));
#38975=CARTESIAN_POINT('Ctrl Pts',(211.004980992208,5.12864925304842,-0.475001134495899));
#38976=CARTESIAN_POINT('Ctrl Pts',(211.084170563266,4.73350352671038,2.03042202528198));
#38977=CARTESIAN_POINT('Ctrl Pts',(211.163360134324,3.19046837399552,4.04346148652501));
#38978=CARTESIAN_POINT('Ctrl Pts',(211.242549705381,0.873734650797867,5.07594887664184));
#38979=CARTESIAN_POINT('Ctrl Pts',(211.321739276439,-1.65488246098097,4.87750277075313));
#38980=CARTESIAN_POINT('Ctrl Pts',(211.400928847496,-3.78218539432946,3.49624697086225));
#38981=CARTESIAN_POINT('Ctrl Pts',(211.480118418554,-4.99229652704541,1.26714033334719));
#38982=CARTESIAN_POINT('Ctrl Pts',(211.559307989611,-4.99176012043676,-1.26925180258506));
#38983=CARTESIAN_POINT('Ctrl Pts',(211.638497560669,-3.78070625478386,-3.49784640219995));
#38984=CARTESIAN_POINT('Ctrl Pts',(211.717687131727,-1.65281928447252,-4.87820229707857));
#38985=CARTESIAN_POINT('Ctrl Pts',(211.796876702784,0.875881537511563,-5.07557886064165));
#38986=CARTESIAN_POINT('Ctrl Pts',(211.876066273842,3.1921783441522,-4.04211165821431));
#38987=CARTESIAN_POINT('Ctrl Pts',(211.955255844899,4.73436190721831,-2.02841972230267));
#38988=CARTESIAN_POINT('Ctrl Pts',(212.034445415957,5.12844788389286,0.47717034750827));
#38989=CARTESIAN_POINT('Ctrl Pts',(212.113634987014,4.27886919089879,2.86704511396724));
#38990=CARTESIAN_POINT('Ctrl Pts',(212.192824558072,2.39165132142645,4.56165246320512));
#38991=CARTESIAN_POINT('Ctrl Pts',(212.272014129129,-0.0755494820572054,
5.15004480699995));
#38992=CARTESIAN_POINT('Ctrl Pts',(212.351203700187,-2.52442929958692,4.48953515964998));
#38993=CARTESIAN_POINT('Ctrl Pts',(212.430393271245,-4.36112710765662,2.74029917877754));
#38994=CARTESIAN_POINT('Ctrl Pts',(212.509582842302,-5.14023793687424,0.326532066825224));
#38995=CARTESIAN_POINT('Ctrl Pts',(212.588772413359,-4.67282497165909,-2.16642009374577));
#38996=CARTESIAN_POINT('Ctrl Pts',(212.667961984417,-3.0722373196055,-4.13400859824571));
#38997=CARTESIAN_POINT('Ctrl Pts',(212.747151555475,-0.726622497980572,
-5.09908707356275));
#38998=CARTESIAN_POINT('Ctrl Pts',(212.826341126532,1.79520055455238,-4.82762096764867));
#38999=CARTESIAN_POINT('Ctrl Pts',(212.90553069759,3.88168185160442,-3.38544166118265));
#39000=CARTESIAN_POINT('Ctrl Pts',(212.984720268647,5.0268431456013,-1.1222821516301));
#39001=CARTESIAN_POINT('Ctrl Pts',(213.063909839705,4.95297923710267,1.41303429370134));
#39002=CARTESIAN_POINT('Ctrl Pts',(213.143099410763,3.67800235519679,3.60568549841956));
#39003=CARTESIAN_POINT('Ctrl Pts',(213.22228898182,1.51109838586108,4.92394667990976));
#39004=CARTESIAN_POINT('Ctrl Pts',(213.301478552878,-1.02225167348779,5.0481353740166));
#39005=CARTESIAN_POINT('Ctrl Pts',(213.380668123935,-3.30770250121545,3.94813543356853));
#39006=CARTESIAN_POINT('Ctrl Pts',(213.459857694993,-4.79102511555983,1.89070028836437));
#39007=CARTESIAN_POINT('Ctrl Pts',(213.53904726605,-5.11250913807012,-0.625235596791949));
#39008=CARTESIAN_POINT('Ctrl Pts',(213.618236837108,-4.19419368668006,-2.98954989203382));
#39009=CARTESIAN_POINT('Ctrl Pts',(213.697426408165,-2.25877313371456,-4.62888897779538));
#39010=CARTESIAN_POINT('Ctrl Pts',(213.776615979223,0.224406976683579,-5.14570799279964));
#39011=CARTESIAN_POINT('Ctrl Pts',(213.85580555028,2.65316769258906,-4.41467670768176));
#39012=CARTESIAN_POINT('Ctrl Pts',(213.934995121338,4.43852693563516,-2.6130724980351));
#39013=CARTESIAN_POINT('Ctrl Pts',(214.014184692395,5.14752949919566,-0.177790025751574));
#39014=CARTESIAN_POINT('Ctrl Pts',(214.093374263453,4.60824004162965,2.30060708445997));
#39015=CARTESIAN_POINT('Ctrl Pts',(214.172563834511,2.95143794498097,4.2210997731957));
#39016=CARTESIAN_POINT('Ctrl Pts',(214.251753405568,0.578902905345666,5.11796255012955));
#39017=CARTESIAN_POINT('Ctrl Pts',(214.330942976626,-1.9340179014548,4.77370338366332));
#39018=CARTESIAN_POINT('Ctrl Pts',(214.410132547683,-3.97793331149569,3.27180619958444));
#39019=CARTESIAN_POINT('Ctrl Pts',(214.489322118741,-5.05718743808221,0.976485767663708));
#39020=CARTESIAN_POINT('Ctrl Pts',(214.568511689798,-4.91005777623474,-1.55563552041699));
#39021=CARTESIAN_POINT('Ctrl Pts',(214.647701260856,-3.57222372963305,-3.71051032390327));
#39022=CARTESIAN_POINT('Ctrl Pts',(214.726890831913,-1.36811424350713,-4.96557475576184));
#39023=CARTESIAN_POINT('Ctrl Pts',(214.806080402971,1.16776723040952,-5.0164717615001));
#39024=CARTESIAN_POINT('Ctrl Pts',(214.885269974028,3.42046149452369,-3.85085865786152));
#39025=CARTESIAN_POINT('Ctrl Pts',(214.964459545086,4.84368313631455,-1.75140027216177));
#39026=CARTESIAN_POINT('Ctrl Pts',(215.043649116144,5.09229645135928,0.772778163394885));
#39027=CARTESIAN_POINT('Ctrl Pts',(215.122838687201,4.10601193231954,3.10955547466126));
#39028=CARTESIAN_POINT('Ctrl Pts',(215.202028258259,2.12400666324514,4.69225584690738));
#39029=CARTESIAN_POINT('Ctrl Pts',(215.281217829316,-0.373076872202056,
5.1370694842268));
#39030=CARTESIAN_POINT('Ctrl Pts',(215.360407400374,-2.77968809798898,4.33612768680129));
#39031=CARTESIAN_POINT('Ctrl Pts',(215.439596971431,-4.51221625645552,2.48366134835748));
#39032=CARTESIAN_POINT('Ctrl Pts',(215.518786542489,-5.15051784440682,0.0288993562764492));
#39033=CARTESIAN_POINT('Ctrl Pts',(215.597976113546,-4.53980272816102,-2.43287082018918));
#39034=CARTESIAN_POINT('Ctrl Pts',(215.677165684604,-2.82817123563468,-4.30466220513002));
#39035=CARTESIAN_POINT('Ctrl Pts',(215.756355255662,-0.430699363101971,
-5.13255952688031));
#39036=CARTESIAN_POINT('Ctrl Pts',(215.835544826719,2.07121845355762,-4.71579509266345));
#39037=CARTESIAN_POINT('Ctrl Pts',(215.914734397777,4.07085930998026,-3.15543558271965));
#39038=CARTESIAN_POINT('Ctrl Pts',(215.993923968834,5.08330403735285,-0.829873063894976));
#39039=CARTESIAN_POINT('Ctrl Pts',(216.073113539892,4.86303161919394,1.69693627136268));
#39040=CARTESIAN_POINT('Ctrl Pts',(216.152303110949,3.46345880660808,3.81223324749093));
#39041=CARTESIAN_POINT('Ctrl Pts',(216.231492682007,1.22398638888836,5.00305172451398));
#39042=CARTESIAN_POINT('Ctrl Pts',(216.310682253064,-1.3123065605943,4.98061449314915));
#39043=CARTESIAN_POINT('Ctrl Pts',(216.389871824122,-3.53036106013357,3.75036265225628));
#39044=CARTESIAN_POINT('Ctrl Pts',(216.469061395179,-4.8922919485796,1.61063612532735));
#39045=CARTESIAN_POINT('Ctrl Pts',(216.548250966237,-5.06782672110485,-0.919674705100661));
#39046=CARTESIAN_POINT('Ctrl Pts',(216.627440537294,-4.01439764575017,-3.22696153992293));
#39047=CARTESIAN_POINT('Ctrl Pts',(216.706630108352,-1.98746457170991,-4.75170009728562));
#39048=CARTESIAN_POINT('Ctrl Pts',(216.78581967941,0.521434883975116,-5.12413650287735));
#39049=CARTESIAN_POINT('Ctrl Pts',(216.865009250467,2.90388474761705,-4.25395376219621));
#39050=CARTESIAN_POINT('Ctrl Pts',(216.944198821525,4.58213346752824,-2.35217391451056));
#39051=CARTESIAN_POINT('Ctrl Pts',(217.023388392582,5.14920047431936,0.120015472400531));
#39052=CARTESIAN_POINT('Ctrl Pts',(217.10257796364,4.46757024328443,2.56310073147072));
#39053=CARTESIAN_POINT('Ctrl Pts',(217.181767534698,2.70254023972065,4.38462603776387));
#39054=CARTESIAN_POINT('Ctrl Pts',(217.260957105755,0.282135766026347,5.1428658010758));
#39055=CARTESIAN_POINT('Ctrl Pts',(217.340146676812,-2.20668751433244,4.65394450465791));
#39056=CARTESIAN_POINT('Ctrl Pts',(217.41933624787,-4.16038216304547,3.03642709376651));
#39057=CARTESIAN_POINT('Ctrl Pts',(217.498525818927,-5.10517111053266,0.682566605196131));
#39058=CARTESIAN_POINT('Ctrl Pts',(217.577715389985,-4.81194007877364,-1.83681842233742));
#39059=CARTESIAN_POINT('Ctrl Pts',(217.656904961043,-3.35179851111375,-3.91076923114136));
#39060=CARTESIAN_POINT('Ctrl Pts',(217.7360945321,-1.0788353096,-5.03634625627613));
#39061=CARTESIAN_POINT('Ctrl Pts',(217.815284103158,1.45574883246274,-4.94059354482127));
#39062=CARTESIAN_POINT('Ctrl Pts',(217.894473674215,3.63730932451793,-3.64673142911857));
#39063=CARTESIAN_POINT('Ctrl Pts',(217.973663245273,4.93681091649799,-1.46852552347328));
#39064=CARTESIAN_POINT('Ctrl Pts',(218.05285281633,5.03912040344251,1.06580241975503));
#39065=CARTESIAN_POINT('Ctrl Pts',(218.132042387388,3.91942741442336,3.34166993902942));
#39066=CARTESIAN_POINT('Ctrl Pts',(218.211231958445,1.84926100517927,4.80717203489428));
#39067=CARTESIAN_POINT('Ctrl Pts',(218.290421529503,-0.669356988092899,
5.10691986042834));
#39068=CARTESIAN_POINT('Ctrl Pts',(218.369611100561,-3.02565381591041,4.16822362939094));
#39069=CARTESIAN_POINT('Ctrl Pts',(218.448800671618,-4.64822011966157,2.2187201169863));
#39070=CARTESIAN_POINT('Ctrl Pts',(218.527990242676,-5.1435784902246,-0.268829970883292));
#39071=CARTESIAN_POINT('Ctrl Pts',(218.607179813733,-4.3916029717077,-2.69118794907274));
#39072=CARTESIAN_POINT('Ctrl Pts',(218.686369384791,-2.57464998188252,-4.46092442315924));
#39073=CARTESIAN_POINT('Ctrl Pts',(218.765558955848,-0.13333630989329,-5.14887275690614));
#39074=CARTESIAN_POINT('Ctrl Pts',(218.844748526906,2.34031183473807,-4.58820332532585));
#39075=CARTESIAN_POINT('Ctrl Pts',(218.923938097963,4.24642703163054,-2.91488022110407));
#39076=CARTESIAN_POINT('Ctrl Pts',(219.003127669021,5.12277037724782,-0.534689536402703));
#39077=CARTESIAN_POINT('Ctrl Pts',(219.082317240078,4.75682586633489,1.97516503505748));
#39078=CARTESIAN_POINT('Ctrl Pts',(219.161506811136,3.2373361886071,4.0060359010225));
#39079=CARTESIAN_POINT('Ctrl Pts',(219.240696382194,0.93278234862948,5.06543051758008));
#39080=CARTESIAN_POINT('Ctrl Pts',(219.319885953251,-1.59797413155131,4.8964423731153));
#39081=CARTESIAN_POINT('Ctrl Pts',(219.399075524309,-3.74121688137005,3.54005162178436));
#39082=CARTESIAN_POINT('Ctrl Pts',(219.478265095366,-4.97720282322922,1.32518726781742));
#39083=CARTESIAN_POINT('Ctrl Pts',(219.557454666424,-5.00620149619827,-1.21103914792564));
#39084=CARTESIAN_POINT('Ctrl Pts',(219.636644237481,-3.82118063128369,-3.45358477837864));
#39085=CARTESIAN_POINT('Ctrl Pts',(219.715833808539,-1.70951149867879,-4.85862528646028));
#39086=CARTESIAN_POINT('Ctrl Pts',(219.795023379597,0.816719525054341,-5.08543394959972));
#39087=CARTESIAN_POINT('Ctrl Pts',(219.874212950654,3.14489350670873,-4.07900895681872));
#39088=CARTESIAN_POINT('Ctrl Pts',(219.953402521712,4.71042096592359,-2.08341152011178));
#39089=CARTESIAN_POINT('Ctrl Pts',(220.032592092769,5.1336565919727,0.417419733649592));
#39090=CARTESIAN_POINT('Ctrl Pts',(220.111781663827,4.31196442033532,2.81702539500632));
#39091=CARTESIAN_POINT('Ctrl Pts',(220.190971234884,2.44460737545468,4.53349357760849));
#39092=CARTESIAN_POINT('Ctrl Pts',(220.270160805942,-0.0155746123486556,
5.1505753726931));
#39093=CARTESIAN_POINT('Ctrl Pts',(220.349350376999,-2.47197970789699,4.51862651279263));
#39094=CARTESIAN_POINT('Ctrl Pts',(220.428539948057,-4.32892198418446,2.79089657514049));
#39095=CARTESIAN_POINT('Ctrl Pts',(220.507729519114,-5.13608712492566,0.386365479370735));
#39096=CARTESIAN_POINT('Ctrl Pts',(220.586919090172,-4.69773505607432,-2.11186045492126));
#39097=CARTESIAN_POINT('Ctrl Pts',(220.66610866123,-3.12016752703196,-4.09795361635802));
#39098=CARTESIAN_POINT('Ctrl Pts',(220.745298232287,-0.785949602798,-5.09028019468105));
#39099=CARTESIAN_POINT('Ctrl Pts',(220.824487803345,1.73886356050538,-4.84819788733142));
#39100=CARTESIAN_POINT('Ctrl Pts',(220.903677374402,3.84199686688144,-3.43041241228741));
#39101=CARTESIAN_POINT('Ctrl Pts',(220.98286694546,5.01343390092321,-1.18074118554751));
#39102=CARTESIAN_POINT('Ctrl Pts',(221.062056516517,4.96909752124399,1.35526347434335));
#39103=CARTESIAN_POINT('Ctrl Pts',(221.141246087575,3.71973942326616,3.56261250116638));
#39104=CARTESIAN_POINT('Ctrl Pts',(221.220435658633,1.56833289050138,4.90601683517051));
#39105=CARTESIAN_POINT('Ctrl Pts',(221.29962522969,-0.963399326280619,5.05969673864025));
#39106=CARTESIAN_POINT('Ctrl Pts',(221.378814800748,-3.26150408922802,3.98638431206907));
#39107=CARTESIAN_POINT('Ctrl Pts',(221.458004371805,-4.76868411213275,1.94636126816844));
#39108=CARTESIAN_POINT('Ctrl Pts',(221.537193942863,-5.11944285257571,-0.565660605443682));
#39109=CARTESIAN_POINT('Ctrl Pts',(221.61638351392,-4.22872163540365,-2.94050773958088));
#39110=CARTESIAN_POINT('Ctrl Pts',(221.695573084978,-2.31252013462662,-4.60227311630824));
#39111=CARTESIAN_POINT('Ctrl Pts',(221.774762656035,0.164470394917766,-5.14797162841751));
#39112=CARTESIAN_POINT('Ctrl Pts',(221.853952227093,2.60158556523968,-4.44527350328976));
#39113=CARTESIAN_POINT('Ctrl Pts',(221.93314179815,4.40778851090815,-2.6645771347152));
#39114=CARTESIAN_POINT('Ctrl Pts',(222.012331369208,5.1451305867893,-0.237724303700579));
#39115=CARTESIAN_POINT('Ctrl Pts',(222.091520940265,4.63467444150074,2.24680150964327));
#39116=CARTESIAN_POINT('Ctrl Pts',(222.170710511323,3.00048534671845,4.18641270900455));
#39117=CARTESIAN_POINT('Ctrl Pts',(222.24990008238,0.638283697933631,5.11088637052273));
#39118=CARTESIAN_POINT('Ctrl Pts',(222.302693129752,-1.03902234995174,4.90057399389068));
#39119=CARTESIAN_POINT('Ctrl Pts',(222.329089653438,-1.80222833897997,4.6016667647905));
#39120=CARTESIAN_POINT('',(222.,4.90426805507063,-0.609523456491791));
#39121=CARTESIAN_POINT('Ctrl Pts',(222.,4.90448285458831,-0.609441531220142));
#39122=CARTESIAN_POINT('Ctrl Pts',(222.,4.91326917733984,-0.482075978558733));
#39123=CARTESIAN_POINT('Ctrl Pts',(222.,4.91707785477246,-0.354546138090381));
#39124=CARTESIAN_POINT('Ctrl Pts',(222.,4.91582655810574,-0.227126274667179));
#39125=CARTESIAN_POINT('Ctrl Pts',(222.,4.9143947739523,-0.0813273237593178));
#39126=CARTESIAN_POINT('Ctrl Pts',(222.,4.90633894433518,0.0643283824542994));
#39127=CARTESIAN_POINT('Ctrl Pts',(222.,4.89177207858516,0.209411418078174));
#39128=CARTESIAN_POINT('Ctrl Pts',(222.,4.88353154766168,0.291485438807731));
#39129=CARTESIAN_POINT('Ctrl Pts',(222.,4.87320640955617,0.373376035009041));
#39130=CARTESIAN_POINT('Ctrl Pts',(222.,4.86081007005833,0.455003302996157));
#39131=CARTESIAN_POINT('Ctrl Pts',(222.,4.85194006741065,0.513410390289533));
#39132=CARTESIAN_POINT('Ctrl Pts',(222.,4.84200952702687,0.571682622382685));
#39133=CARTESIAN_POINT('Ctrl Pts',(222.,4.8310218344987,0.629789994814728));
#39134=CARTESIAN_POINT('Ctrl Pts',(222.,4.82673488428677,0.652461125438654));
#39135=CARTESIAN_POINT('Ctrl Pts',(222.,4.8222869719834,0.675106928971051));
#39136=CARTESIAN_POINT('Ctrl Pts',(222.,4.81768123655949,0.697711955872851));
#39137=CARTESIAN_POINT('Ctrl Pts',(222.,4.78883957014647,0.83926733957451));
#39138=CARTESIAN_POINT('Ctrl Pts',(222.,4.75378779279869,0.979361892009339));
#39139=CARTESIAN_POINT('Ctrl Pts',(222.,4.71263944483955,1.11757740639638));
#39140=CARTESIAN_POINT('Ctrl Pts',(222.,4.67174027328832,1.25495594804698));
#39141=CARTESIAN_POINT('Ctrl Pts',(222.,4.62481784578113,1.3904788562509));
#39142=CARTESIAN_POINT('Ctrl Pts',(222.,4.57193686941057,1.52371480352769));
#39143=CARTESIAN_POINT('Ctrl Pts',(222.,4.53175843227578,1.62494614415654));
#39144=CARTESIAN_POINT('Ctrl Pts',(222.,4.48813926663806,1.72485692666779));
#39145=CARTESIAN_POINT('Ctrl Pts',(222.,4.44109105421273,1.82324608763217));
#39146=CARTESIAN_POINT('Ctrl Pts',(222.,4.43330321241965,1.83953234337379));
#39147=CARTESIAN_POINT('Ctrl Pts',(222.,4.42542221910461,1.85577505560334));
#39148=CARTESIAN_POINT('Ctrl Pts',(222.,4.41745220772723,1.87196530421876));
#39149=CARTESIAN_POINT('Ctrl Pts',(222.,4.38168626708121,1.94462009021658));
#39150=CARTESIAN_POINT('Ctrl Pts',(222.,4.34410598143193,2.016264933338));
#39151=CARTESIAN_POINT('Ctrl Pts',(222.,4.30473188164448,2.08682740943665));
#39152=CARTESIAN_POINT('Ctrl Pts',(222.,4.23575714136261,2.21043730753777));
#39153=CARTESIAN_POINT('Ctrl Pts',(222.,4.16128012266586,2.33072748027458));
#39154=CARTESIAN_POINT('Ctrl Pts',(222.,4.08162279945473,2.44740940981428));
#39155=CARTESIAN_POINT('Ctrl Pts',(222.,4.00157270449037,2.56466667083873));
#39156=CARTESIAN_POINT('Ctrl Pts',(222.,3.91629052773537,2.67828059710419));
#39157=CARTESIAN_POINT('Ctrl Pts',(222.,3.82606285547984,2.78792472525375));
#39158=CARTESIAN_POINT('Ctrl Pts',(222.,3.74674547067526,2.88431073728974));
#39159=CARTESIAN_POINT('Ctrl Pts',(222.,3.66360545427877,2.97762870520231));
#39160=CARTESIAN_POINT('Ctrl Pts',(222.,3.57681726235579,3.06763019115416));
#39161=CARTESIAN_POINT('Ctrl Pts',(222.,3.51172611841355,3.13513130561804));
#39162=CARTESIAN_POINT('Ctrl Pts',(222.,3.44458246403701,3.20076641165242));
#39163=CARTESIAN_POINT('Ctrl Pts',(222.,3.37545454247196,3.26441991676624));
#39164=CARTESIAN_POINT('Ctrl Pts',(222.,3.36073243108146,3.27797614660021));
#39165=CARTESIAN_POINT('Ctrl Pts',(222.,3.34591878431476,3.29144382870828));
#39166=CARTESIAN_POINT('Ctrl Pts',(222.,3.33101906241501,3.30481746426802));
#39167=CARTESIAN_POINT('Ctrl Pts',(222.,3.22694638125945,3.39823062451785));
#39168=CARTESIAN_POINT('Ctrl Pts',(222.,3.1189736864245,3.48679412040944));
#39169=CARTESIAN_POINT('Ctrl Pts',(222.,3.00739305624753,3.57022036306246));
#39170=CARTESIAN_POINT('Ctrl Pts',(222.,2.90992116374936,3.64309783061666));
#39171=CARTESIAN_POINT('Ctrl Pts',(222.,2.80969522479396,3.71205475252624));
#39172=CARTESIAN_POINT('Ctrl Pts',(222.,2.7068907197599,3.77687313241435));
#39173=CARTESIAN_POINT('Ctrl Pts',(222.,2.58891295229675,3.85125827484798));
#39174=CARTESIAN_POINT('Ctrl Pts',(222.,2.46753906543956,3.92019422568834));
#39175=CARTESIAN_POINT('Ctrl Pts',(222.,2.34317914443504,3.98353319537002));
#39176=CARTESIAN_POINT('Ctrl Pts',(222.,2.21947820439344,4.04653653300165));
#39177=CARTESIAN_POINT('Ctrl Pts',(222.,2.09282200300289,4.10400221753901));
#39178=CARTESIAN_POINT('Ctrl Pts',(222.,1.96360433617035,4.15573443747871));
#39179=CARTESIAN_POINT('Ctrl Pts',(222.,1.91350917960701,4.1757900051172));
#39180=CARTESIAN_POINT('Ctrl Pts',(222.,1.86302900287319,4.19498330383357));
#39181=CARTESIAN_POINT('Ctrl Pts',(222.,1.81218673898867,4.21330078673186));
#39182=CARTESIAN_POINT('Ctrl Pts',(222.,1.79518182048063,4.21942732949686));
#39183=CARTESIAN_POINT('Ctrl Pts',(222.,1.77813690967813,4.2254556476935));
#39184=CARTESIAN_POINT('Ctrl Pts',(222.,1.76106556469781,4.23138098370753));
#39185=CARTESIAN_POINT('Ctrl Pts',(222.,1.63109802355043,4.27649174405501));
#39186=CARTESIAN_POINT('Ctrl Pts',(222.,1.49941025889044,4.31570662400781));
#39187=CARTESIAN_POINT('Ctrl Pts',(222.,1.36640605860325,4.34892093575254));
#39188=CARTESIAN_POINT('Ctrl Pts',(222.,1.23393413223417,4.38200232604207));
#39189=CARTESIAN_POINT('Ctrl Pts',(222.,1.10015550342008,4.40913122338652));
#39190=CARTESIAN_POINT('Ctrl Pts',(222.,0.965458418930057,4.43015396750657));
#39191=CARTESIAN_POINT('Ctrl Pts',(222.,0.830761334440031,4.45117671162661));
#39192=CARTESIAN_POINT('Ctrl Pts',(222.,0.695145040010488,4.46609348868625));
#39193=CARTESIAN_POINT('Ctrl Pts',(222.,0.558998530275823,4.47469779566404));
#39194=CARTESIAN_POINT('Ctrl Pts',(222.,0.467028797805401,4.48051017978159));
#39195=CARTESIAN_POINT('Ctrl Pts',(222.,0.374817124048172,4.48344078212688));
#39196=CARTESIAN_POINT('Ctrl Pts',(222.,0.282495436056599,4.48349800210454));
#39197=CARTESIAN_POINT('Ctrl Pts',(222.,0.239680782870147,4.48352453816071));
#39198=CARTESIAN_POINT('Ctrl Pts',(222.,0.196842516440346,4.48293295657145));
#39199=CARTESIAN_POINT('Ctrl Pts',(222.,0.153994089551905,4.48172336523466));
#39200=CARTESIAN_POINT('Ctrl Pts',(222.,0.12621552348811,4.48093918912134));
#39201=CARTESIAN_POINT('Ctrl Pts',(222.,0.0984326912053478,4.4798952598853));
#39202=CARTESIAN_POINT('Ctrl Pts',(222.,0.0706493101151461,4.47859150531125));
#39203=CARTESIAN_POINT('Ctrl Pts',(222.,0.0514392659198498,4.47769006056246));
#39204=CARTESIAN_POINT('Ctrl Pts',(222.,0.032237116105233,4.47666475864222));
#39205=CARTESIAN_POINT('Ctrl Pts',(222.,0.0130498828690303,4.47551629094421));
#39206=CARTESIAN_POINT('Ctrl Pts',(222.,-0.126040864975259,4.46719089931406));
#39207=CARTESIAN_POINT('Ctrl Pts',(222.,-0.264445813962418,4.45239355914002));
#39208=CARTESIAN_POINT('Ctrl Pts',(222.,-0.401723720439985,4.43124956761349));
#39209=CARTESIAN_POINT('Ctrl Pts',(222.,-0.534675001036407,4.4107719771366));
#39210=CARTESIAN_POINT('Ctrl Pts',(222.,-0.666569928590543,4.38434097588717));
#39211=CARTESIAN_POINT('Ctrl Pts',(222.,-0.796997369050306,4.35201860521038));
#39212=CARTESIAN_POINT('Ctrl Pts',(222.,-0.926299184341642,4.31997518560255));
#39213=CARTESIAN_POINT('Ctrl Pts',(222.,-1.0541594515063,4.28214138070619));
#39214=CARTESIAN_POINT('Ctrl Pts',(222.,-1.18015635582318,4.23853132977908));
#39215=CARTESIAN_POINT('Ctrl Pts',(222.,-1.30349968543307,4.1958397341802));
#39216=CARTESIAN_POINT('Ctrl Pts',(222.,-1.4250578919995,4.14761231940487));
#39217=CARTESIAN_POINT('Ctrl Pts',(222.,-1.54440537989462,4.0938221719545));
#39218=CARTESIAN_POINT('Ctrl Pts',(222.,-1.5611016741838,4.08629711929081));
#39219=CARTESIAN_POINT('Ctrl Pts',(222.,-1.57775464564182,4.07866313700196));
#39220=CARTESIAN_POINT('Ctrl Pts',(222.,-1.59436307123033,4.07092009220237));
#39221=CARTESIAN_POINT('Ctrl Pts',(221.519679545343,-4.94203042585278,-0.000125883567849882));
#39222=CARTESIAN_POINT('Ctrl Pts',(221.52551767785,-4.94221599753283,-0.181402702505943));
#39223=CARTESIAN_POINT('Ctrl Pts',(221.531355810356,-4.93243348869434,-0.362659600138765));
#39224=CARTESIAN_POINT('Ctrl Pts',(221.537193942863,-4.91252952630654,-0.542798148864529));
#39225=CARTESIAN_POINT('Ctrl Pts',(221.563590466548,-4.82253578018502,-1.35727631682275));
#39226=CARTESIAN_POINT('Ctrl Pts',(221.589986990234,-4.52562870779433,-2.14889202820181));
#39227=CARTESIAN_POINT('Ctrl Pts',(221.61638351392,-4.05780825480282,-2.82166078001257));
#39228=CARTESIAN_POINT('Ctrl Pts',(221.642780037606,-3.58998780181129,-3.49442953182335));
#39229=CARTESIAN_POINT('Ctrl Pts',(221.669176561292,-2.95125396821893,-4.04835132406582));
#39230=CARTESIAN_POINT('Ctrl Pts',(221.695573084978,-2.21905529649866,-4.41626197220526));
#39231=CARTESIAN_POINT('Ctrl Pts',(221.721969608664,-1.48685662477844,-4.78417262034468));
#39232=CARTESIAN_POINT('Ctrl Pts',(221.748366132349,-0.661193114930324,
-4.96607212438109));
#39233=CARTESIAN_POINT('Ctrl Pts',(221.774762656035,0.157824501714043,-4.93990552221134));
#39234=CARTESIAN_POINT('Ctrl Pts',(221.801159179721,0.976842118358411,-4.91373892004159));
#39235=CARTESIAN_POINT('Ctrl Pts',(221.827555703407,1.78921384179903,-4.67950621166568));
#39236=CARTESIAN_POINT('Ctrl Pts',(221.853952227093,2.49643352779742,-4.26560712938197));
#39237=CARTESIAN_POINT('Ctrl Pts',(221.880348750779,3.20365321379582,-3.85170804709825));
#39238=CARTESIAN_POINT('Ctrl Pts',(221.906745274465,3.80572086235198,-3.25814259090672));
#39239=CARTESIAN_POINT('Ctrl Pts',(221.93314179815,4.22964503261026,-2.55688439097519));
#39240=CARTESIAN_POINT('Ctrl Pts',(221.955427865434,4.58755589594206,-1.9648258452143));
#39241=CARTESIAN_POINT('Ctrl Pts',(221.977713932717,4.81848441783212,-1.29600290208645));
#39242=CARTESIAN_POINT('Ctrl Pts',(222.,4.90448285458833,-0.609441531219933));
#39243=CARTESIAN_POINT('',(209.342,-2.53854069360603,-3.55974239505386));
#39244=CARTESIAN_POINT('Ctrl Pts',(209.342,-2.53854069360617,-3.55974239505377));
#39245=CARTESIAN_POINT('Ctrl Pts',(209.342,-2.6349877013993,-3.49987489435206));
#39246=CARTESIAN_POINT('Ctrl Pts',(209.342,-2.72895943133216,-3.43630922016219));
#39247=CARTESIAN_POINT('Ctrl Pts',(209.342,-2.82022491817566,-3.36916885592227));
#39248=CARTESIAN_POINT('Ctrl Pts',(209.342,-2.92748910751928,-3.29025888686925));
#39249=CARTESIAN_POINT('Ctrl Pts',(209.342,-3.03101625922222,-3.20641213996167));
#39250=CARTESIAN_POINT('Ctrl Pts',(209.342,-3.13058845059508,-3.11799396863395));
#39251=CARTESIAN_POINT('Ctrl Pts',(209.342,-3.18739359422047,-3.06755210477501));
#39252=CARTESIAN_POINT('Ctrl Pts',(209.342,-3.24291112510208,-3.01562153815868));
#39253=CARTESIAN_POINT('Ctrl Pts',(209.342,-3.29709651834796,-2.96226376957147));
#39254=CARTESIAN_POINT('Ctrl Pts',(209.342,-3.33383376776623,-2.92608764284123));
#39255=CARTESIAN_POINT('Ctrl Pts',(209.342,-3.3699586062124,-2.88925537752558));
#39256=CARTESIAN_POINT('Ctrl Pts',(209.342,-3.40545624307948,-2.85178508415988));
#39257=CARTESIAN_POINT('Ctrl Pts',(209.342,-3.41889230282954,-2.83760236257764));
#39258=CARTESIAN_POINT('Ctrl Pts',(209.342,-3.43223749900502,-2.8233292174573));
#39259=CARTESIAN_POINT('Ctrl Pts',(209.342,-3.44548459322086,-2.80897381138868));
#39260=CARTESIAN_POINT('Ctrl Pts',(209.342,-3.53764467726692,-2.70910319763421));
#39261=CARTESIAN_POINT('Ctrl Pts',(209.342,-3.62514721021095,-2.60516218242286));
#39262=CARTESIAN_POINT('Ctrl Pts',(209.342,-3.70776805623344,-2.49753092189412));
#39263=CARTESIAN_POINT('Ctrl Pts',(209.342,-3.79069451449376,-2.38950153629195));
#39264=CARTESIAN_POINT('Ctrl Pts',(209.342,-3.86870367845508,-2.27775398082505));
#39265=CARTESIAN_POINT('Ctrl Pts',(209.342,-3.9415356848087,-2.1626319845035));
#39266=CARTESIAN_POINT('Ctrl Pts',(209.342,-3.97091706474444,-2.11619027182486));
#39267=CARTESIAN_POINT('Ctrl Pts',(209.342,-3.99945547881667,-2.06919898329292));
#39268=CARTESIAN_POINT('Ctrl Pts',(209.342,-4.02713201378103,-2.02167914966254));
#39269=CARTESIAN_POINT('Ctrl Pts',(209.342,-4.04218110507543,-1.99584028235061));
#39270=CARTESIAN_POINT('Ctrl Pts',(209.342,-4.05697535079495,-1.96984512974782));
#39271=CARTESIAN_POINT('Ctrl Pts',(209.342,-4.07151156318289,-1.94369697898506));
#39272=CARTESIAN_POINT('Ctrl Pts',(209.342,-4.08507675832336,-1.91929552156319));
#39273=CARTESIAN_POINT('Ctrl Pts',(209.342,-4.09841961397682,-1.89475615326754));
#39274=CARTESIAN_POINT('Ctrl Pts',(209.342,-4.11152305824316,-1.87010919482169));
#39275=CARTESIAN_POINT('Ctrl Pts',(209.342,-4.14743612631779,-1.80255841362961));
#39276=CARTESIAN_POINT('Ctrl Pts',(209.342,-4.18157046256384,-1.73416632118921));
#39277=CARTESIAN_POINT('Ctrl Pts',(209.342,-4.2138886632462,-1.66499821702773));
#39278=CARTESIAN_POINT('Ctrl Pts',(209.342,-4.27122750314795,-1.54228040579181));
#39279=CARTESIAN_POINT('Ctrl Pts',(209.342,-4.32285214674876,-1.41712175506451));
#39280=CARTESIAN_POINT('Ctrl Pts',(209.342,-4.36877501690254,-1.289957099055));
#39281=CARTESIAN_POINT('Ctrl Pts',(209.342,-4.41534596983229,-1.16099784216372));
#39282=CARTESIAN_POINT('Ctrl Pts',(209.342,-4.45605337158386,-1.029974895541));
#39283=CARTESIAN_POINT('Ctrl Pts',(209.342,-4.49086552156863,-0.89731224357485));
#39284=CARTESIAN_POINT('Ctrl Pts',(209.342,-4.52200890075814,-0.778630597187785));
#39285=CARTESIAN_POINT('Ctrl Pts',(209.342,-4.54843362771313,-0.658635879371086));
#39286=CARTESIAN_POINT('Ctrl Pts',(209.342,-4.57008457584423,-0.537618862846069));
#39287=CARTESIAN_POINT('Ctrl Pts',(209.342,-4.58632278694256,-0.446856100452307));
#39288=CARTESIAN_POINT('Ctrl Pts',(209.342,-4.59987513097013,-0.355518010485838));
#39289=CARTESIAN_POINT('Ctrl Pts',(209.342,-4.61070640337213,-0.263725114165152));
#39290=CARTESIAN_POINT('Ctrl Pts',(209.342,-4.61385708563983,-0.237023703656357));
#39291=CARTESIAN_POINT('Ctrl Pts',(209.342,-4.61677798423051,-0.210277609469452));
#39292=CARTESIAN_POINT('Ctrl Pts',(209.342,-4.61946488160656,-0.183524245181616));
#39293=CARTESIAN_POINT('Ctrl Pts',(209.342,-4.63351223708837,-0.0436551077019361));
#39294=CARTESIAN_POINT('Ctrl Pts',(209.342,-4.64118722474554,0.0965531284597916));
#39295=CARTESIAN_POINT('Ctrl Pts',(209.342,-4.64248214861728,0.2366538474554));
#39296=CARTESIAN_POINT('Ctrl Pts',(209.342,-4.64349398598631,0.346126802585117));
#39297=CARTESIAN_POINT('Ctrl Pts',(209.342,-4.64060947998757,0.455534806659313));
#39298=CARTESIAN_POINT('Ctrl Pts',(209.342,-4.63380417679374,0.564672361043244));
#39299=CARTESIAN_POINT('Ctrl Pts',(209.342,-4.62513626605827,0.703680800835413));
#39300=CARTESIAN_POINT('Ctrl Pts',(209.342,-4.61010947807627,0.84225083434342));
#39301=CARTESIAN_POINT('Ctrl Pts',(209.342,-4.5889023314112,0.979995389180269));
#39302=CARTESIAN_POINT('Ctrl Pts',(209.342,-4.56757070635119,1.11854845547648));
#39303=CARTESIAN_POINT('Ctrl Pts',(209.342,-4.5399858294126,1.25626708770862));
#39304=CARTESIAN_POINT('Ctrl Pts',(209.342,-4.50627697501283,1.39275336470125));
#39305=CARTESIAN_POINT('Ctrl Pts',(209.342,-4.49324560349942,1.44551704990042));
#39306=CARTESIAN_POINT('Ctrl Pts',(209.342,-4.47929846871971,1.49809645764725));
#39307=CARTESIAN_POINT('Ctrl Pts',(209.342,-4.46444102040819,1.55046805929348));
#39308=CARTESIAN_POINT('Ctrl Pts',(209.342,-4.45834510918231,1.5719557756024));
#39309=CARTESIAN_POINT('Ctrl Pts',(209.342,-4.45209528668334,1.59341042954444));
#39310=CARTESIAN_POINT('Ctrl Pts',(209.342,-4.44569855505466,1.61480883852867));
#39311=CARTESIAN_POINT('Ctrl Pts',(209.342,-4.40499058452271,1.75098553827577));
#39312=CARTESIAN_POINT('Ctrl Pts',(209.342,-4.35828425914468,1.88507637301277));
#39313=CARTESIAN_POINT('Ctrl Pts',(209.342,-4.30579956169708,2.01668804744628));
#39314=CARTESIAN_POINT('Ctrl Pts',(209.342,-4.25229708069577,2.15085193622469));
#39315=CARTESIAN_POINT('Ctrl Pts',(209.342,-4.19278989677581,2.28244039276155));
#39316=CARTESIAN_POINT('Ctrl Pts',(209.342,-4.12745611479573,2.41103351755446));
#39317=CARTESIAN_POINT('Ctrl Pts',(209.342,-4.06212233281564,2.53962664234737));
#39318=CARTESIAN_POINT('Ctrl Pts',(209.342,-3.99096173488706,2.66522526969368));
#39319=CARTESIAN_POINT('Ctrl Pts',(209.342,-3.91410031164534,2.78739382776747));
#39320=CARTESIAN_POINT('Ctrl Pts',(209.342,-3.86029917566832,2.87290886154941));
#39321=CARTESIAN_POINT('Ctrl Pts',(209.342,-3.80370370371757,2.95674294064152));
#39322=CARTESIAN_POINT('Ctrl Pts',(209.342,-3.74442332099379,3.03879836555337));
#39323=CARTESIAN_POINT('Ctrl Pts',(209.342,-3.71848815355214,3.07469761395231));
#39324=CARTESIAN_POINT('Ctrl Pts',(209.342,-3.69203893552856,3.110256321026));
#39325=CARTESIAN_POINT('Ctrl Pts',(209.342,-3.66508419824396,3.14546582364801));
#39326=CARTESIAN_POINT('Ctrl Pts',(209.342,-3.64819963435168,3.16752120821214));
#39327=CARTESIAN_POINT('Ctrl Pts',(209.342,-3.6311167062146,3.18943956499776));
#39328=CARTESIAN_POINT('Ctrl Pts',(209.342,-3.61383743942568,3.21121869963276));
#39329=CARTESIAN_POINT('Ctrl Pts',(209.342,-3.60229869835278,3.22576236044978));
#39330=CARTESIAN_POINT('Ctrl Pts',(209.342,-3.59067553940754,3.24023993544928));
#39331=CARTESIAN_POINT('Ctrl Pts',(209.342,-3.57897369494969,3.25464484972412));
#39332=CARTESIAN_POINT('Ctrl Pts',(209.342,-3.48891908829218,3.36550163761165));
#39333=CARTESIAN_POINT('Ctrl Pts',(209.342,-3.39412108048915,3.47216689410339));
#39334=CARTESIAN_POINT('Ctrl Pts',(209.342,-3.29496106328392,3.57441629318392));
#39335=CARTESIAN_POINT('Ctrl Pts',(209.342,-3.19397353135956,3.67855014415453));
#39336=CARTESIAN_POINT('Ctrl Pts',(209.342,-3.08846133700036,3.77810448924538));
#39337=CARTESIAN_POINT('Ctrl Pts',(209.342,-2.9787792577949,3.87281847405827));
#39338=CARTESIAN_POINT('Ctrl Pts',(209.342,-2.86895681661178,3.96765366592994));
#39339=CARTESIAN_POINT('Ctrl Pts',(209.342,-2.75495327666192,4.05763668470962));
#39340=CARTESIAN_POINT('Ctrl Pts',(209.342,-2.6370841846052,4.14247293811633));
#39341=CARTESIAN_POINT('Ctrl Pts',(209.342,-2.52058663017021,4.2263220276177));
#39342=CARTESIAN_POINT('Ctrl Pts',(209.342,-2.4003123772207,4.30514392692405));
#39343=CARTESIAN_POINT('Ctrl Pts',(209.342,-2.27653488851178,4.37861434524912));
#39344=CARTESIAN_POINT('Ctrl Pts',(209.342,-2.24103337778535,4.39968692372401));
#39345=CARTESIAN_POINT('Ctrl Pts',(209.342,-2.20524350840695,4.42031898826745));
#39346=CARTESIAN_POINT('Ctrl Pts',(209.342,-2.16917135428551,4.44050218283329));
#39347=CARTESIAN_POINT('Ctrl Pts',(209.342,-2.53854069360603,-3.55974239505386));
#39348=CARTESIAN_POINT('Ctrl Pts',(209.364286067283,-2.03981491325066,-3.91465767403852));
#39349=CARTESIAN_POINT('Ctrl Pts',(209.412968658252,-0.786126241680141,
-4.46051691609693));
#39350=CARTESIAN_POINT('Ctrl Pts',(209.488047772907,1.33865191662591,-4.35546678832985));
#39351=CARTESIAN_POINT('Ctrl Pts',(209.567237343965,3.25513899273275,-3.1884349607263));
#39352=CARTESIAN_POINT('Ctrl Pts',(209.646426915022,4.38224084314362,-1.24820523943406));
#39353=CARTESIAN_POINT('Ctrl Pts',(209.72561648608,4.4466373711158,0.994721723380339));
#39354=CARTESIAN_POINT('Ctrl Pts',(209.804806057137,3.43270956435134,2.99642387551628));
#39355=CARTESIAN_POINT('Ctrl Pts',(209.883995628195,1.58633933997099,4.27148464599025));
#39356=CARTESIAN_POINT('Ctrl Pts',(209.963185199253,-0.644723329766792,
4.51069664301433));
#39357=CARTESIAN_POINT('Ctrl Pts',(210.04237477031,-2.71943848460081,3.6560507558529));
#39358=CARTESIAN_POINT('Ctrl Pts',(210.118176334528,-4.07413229445598,1.98929778409173));
#39359=CARTESIAN_POINT('Ctrl Pts',(210.167581375059,-4.3716724462746,0.631855615331185));
#39360=CARTESIAN_POINT('Ctrl Pts',(210.190589891905,-4.37223008469844,-8.48050595506078E-5));
#39361=CARTESIAN_POINT('Origin',(209.342,-4.51336705371395E-16,0.));
#39362=CARTESIAN_POINT('',(209.342,-4.94200000000001,-6.05220448138623E-16));
#39363=CARTESIAN_POINT('Origin',(209.342,0.,0.));
#39364=CARTESIAN_POINT('Origin',(209.342,0.,0.));
#39365=CARTESIAN_POINT('',(209.342,2.5383587572263,-3.55965150255085));
#39366=CARTESIAN_POINT('Ctrl Pts',(209.342,2.16935732978974,4.44063731407447));
#39367=CARTESIAN_POINT('Ctrl Pts',(209.342,2.28083034847072,4.37840428778324));
#39368=CARTESIAN_POINT('Ctrl Pts',(209.342,2.38972120560265,4.31191257789851));
#39369=CARTESIAN_POINT('Ctrl Pts',(209.342,2.4957552127191,4.24124308848005));
#39370=CARTESIAN_POINT('Ctrl Pts',(209.342,2.61708360362285,4.16038020618121));
#39371=CARTESIAN_POINT('Ctrl Pts',(209.342,2.73467268219725,4.07404776792419));
#39372=CARTESIAN_POINT('Ctrl Pts',(209.342,2.84822453982244,3.98257505818366));
#39373=CARTESIAN_POINT('Ctrl Pts',(209.342,2.91246125417312,3.9308286011078));
#39374=CARTESIAN_POINT('Ctrl Pts',(209.342,2.97540532777855,3.87743644914975));
#39375=CARTESIAN_POINT('Ctrl Pts',(209.342,3.03699716389969,3.82245348897652));
#39376=CARTESIAN_POINT('Ctrl Pts',(209.342,3.08106821799472,3.78311131045575));
#39377=CARTESIAN_POINT('Ctrl Pts',(209.342,3.12444685526241,3.74295458595479));
#39378=CARTESIAN_POINT('Ctrl Pts',(209.342,3.16710979599021,3.70200254527677));
#39379=CARTESIAN_POINT('Ctrl Pts',(209.342,3.18375513858242,3.68602472623038));
#39380=CARTESIAN_POINT('Ctrl Pts',(209.342,3.20029132024471,3.66992593549385));
#39381=CARTESIAN_POINT('Ctrl Pts',(209.342,3.21670711667039,3.65371724358499));
#39382=CARTESIAN_POINT('Ctrl Pts',(209.342,3.31950479669339,3.55221647680933));
#39383=CARTESIAN_POINT('Ctrl Pts',(209.342,3.41768582005176,3.44631275793146));
#39384=CARTESIAN_POINT('Ctrl Pts',(209.342,3.51096196457959,3.33632968608582));
#39385=CARTESIAN_POINT('Ctrl Pts',(209.342,3.60367326944256,3.22701262377301));
#39386=CARTESIAN_POINT('Ctrl Pts',(209.342,3.69153935620988,3.11366482343842));
#39387=CARTESIAN_POINT('Ctrl Pts',(209.342,3.77423433156167,2.996576154091));
#39388=CARTESIAN_POINT('Ctrl Pts',(209.342,3.83706514758663,2.90761335301298));
#39389=CARTESIAN_POINT('Ctrl Pts',(209.342,3.89690996444767,2.81649039091281));
#39390=CARTESIAN_POINT('Ctrl Pts',(209.342,3.95360676868133,2.72332691152732));
#39391=CARTESIAN_POINT('Ctrl Pts',(209.342,3.96299173203349,2.70790565716191));
#39392=CARTESIAN_POINT('Ctrl Pts',(209.342,3.97228932900057,2.69243017771718));
#39393=CARTESIAN_POINT('Ctrl Pts',(209.342,3.98149434724664,2.67690880897368));
#39394=CARTESIAN_POINT('Ctrl Pts',(209.342,4.02280245884576,2.60725566814465));
#39395=CARTESIAN_POINT('Ctrl Pts',(209.342,4.06227336715778,2.53663478972804));
#39396=CARTESIAN_POINT('Ctrl Pts',(209.342,4.0998576328727,2.46510294105804));
#39397=CARTESIAN_POINT('Ctrl Pts',(209.342,4.16569698017407,2.33979491286836));
#39398=CARTESIAN_POINT('Ctrl Pts',(209.342,4.22574955040824,2.21169245175744));
#39399=CARTESIAN_POINT('Ctrl Pts',(209.342,4.27994962666695,2.08122286415638));
#39400=CARTESIAN_POINT('Ctrl Pts',(209.342,4.33441695131631,1.95010996035133));
#39401=CARTESIAN_POINT('Ctrl Pts',(209.342,4.3829741009233,1.81660573893223));
#39402=CARTESIAN_POINT('Ctrl Pts',(209.342,4.42550424254866,1.68112860143975));
#39403=CARTESIAN_POINT('Ctrl Pts',(209.342,4.46289165918603,1.56203329654074));
#39404=CARTESIAN_POINT('Ctrl Pts',(209.342,4.49562083867352,1.44141279236264));
#39405=CARTESIAN_POINT('Ctrl Pts',(209.342,4.52357902926892,1.31954894560292));
#39406=CARTESIAN_POINT('Ctrl Pts',(209.342,4.54454767221548,1.22815106053312));
#39407=CARTESIAN_POINT('Ctrl Pts',(209.342,4.56283200080972,1.13605371672259));
#39408=CARTESIAN_POINT('Ctrl Pts',(209.342,4.57837249086842,1.04337722880969));
#39409=CARTESIAN_POINT('Ctrl Pts',(209.342,4.58168213497945,1.02364000100714));
#39410=CARTESIAN_POINT('Ctrl Pts',(209.342,4.58486760349077,1.00387449172836));
#39411=CARTESIAN_POINT('Ctrl Pts',(209.342,4.58792727443095,0.984088278604412));
#39412=CARTESIAN_POINT('Ctrl Pts',(209.342,4.60929869169466,0.845884064815334));
#39413=CARTESIAN_POINT('Ctrl Pts',(209.342,4.62447743383398,0.707063308822669));
#39414=CARTESIAN_POINT('Ctrl Pts',(209.342,4.63338222718942,0.568027771136266));
#39415=CARTESIAN_POINT('Ctrl Pts',(209.342,4.6411610596881,0.446572492405312));
#39416=CARTESIAN_POINT('Ctrl Pts',(209.342,4.64415153042464,0.324952785915422));
#39417=CARTESIAN_POINT('Ctrl Pts',(209.342,4.64226694290985,0.203434733211828));
#39418=CARTESIAN_POINT('Ctrl Pts',(209.342,4.64010420278125,0.0639814221460967));
#39419=CARTESIAN_POINT('Ctrl Pts',(209.342,4.63152199228626,-0.075338827690575));
#39420=CARTESIAN_POINT('Ctrl Pts',(209.342,4.61662060143202,-0.214101806503654));
#39421=CARTESIAN_POINT('Ctrl Pts',(209.342,4.60179817353413,-0.352129475764245));
#39422=CARTESIAN_POINT('Ctrl Pts',(209.342,4.58072306891116,-0.489606517490044));
#39423=CARTESIAN_POINT('Ctrl Pts',(209.342,4.55344645744459,-0.626096125820327));
#39424=CARTESIAN_POINT('Ctrl Pts',(209.342,4.5428718464784,-0.679010488397532));
#39425=CARTESIAN_POINT('Ctrl Pts',(209.342,4.53136468778828,-0.731776177221943));
#39426=CARTESIAN_POINT('Ctrl Pts',(209.342,4.51892616592192,-0.784366583247235));
#39427=CARTESIAN_POINT('Ctrl Pts',(209.342,4.51476592663783,-0.801956187177935));
#39428=CARTESIAN_POINT('Ctrl Pts',(209.342,4.51050156997105,-0.81952561642285));
#39429=CARTESIAN_POINT('Ctrl Pts',(209.342,4.50613651936222,-0.83706091614901));
#39430=CARTESIAN_POINT('Ctrl Pts',(209.342,4.47290452011878,-0.970560643747779));
#39431=CARTESIAN_POINT('Ctrl Pts',(209.342,4.43379463524881,-1.10227963075694));
#39432=CARTESIAN_POINT('Ctrl Pts',(209.342,4.38893981285202,-1.23182249216731));
#39433=CARTESIAN_POINT('Ctrl Pts',(209.342,4.34426449583392,-1.3608469335026));
#39434=CARTESIAN_POINT('Ctrl Pts',(209.342,4.29388982367071,-1.48771336542518));
#39435=CARTESIAN_POINT('Ctrl Pts',(209.342,4.2378992370765,-1.61201266075259));
#39436=CARTESIAN_POINT('Ctrl Pts',(209.342,4.18190865048229,-1.73631195607999));
#39437=CARTESIAN_POINT('Ctrl Pts',(209.342,4.12030189324976,-1.85804484824877));
#39438=CARTESIAN_POINT('Ctrl Pts',(209.342,4.05311855743346,-1.97677271072609));
#39439=CARTESIAN_POINT('Ctrl Pts',(209.342,4.00773484962232,-2.05697579314588));
#39440=CARTESIAN_POINT('Ctrl Pts',(209.342,3.95980537285593,-2.13580691803772));
#39441=CARTESIAN_POINT('Ctrl Pts',(209.342,3.90940924621182,-2.21316018241094));
#39442=CARTESIAN_POINT('Ctrl Pts',(209.342,3.88603778600824,-2.24903315242473));
#39443=CARTESIAN_POINT('Ctrl Pts',(209.342,3.86213573272516,-2.2845881630747));
#39444=CARTESIAN_POINT('Ctrl Pts',(209.342,3.83771052726995,-2.31981400625445));
#39445=CARTESIAN_POINT('Ctrl Pts',(209.342,3.82187570579579,-2.34265086382156));
#39446=CARTESIAN_POINT('Ctrl Pts',(209.342,3.80582100272928,-2.3653493667811));
#39447=CARTESIAN_POINT('Ctrl Pts',(209.342,3.78954838876465,-2.38790636224504));
#39448=CARTESIAN_POINT('Ctrl Pts',(209.342,3.77829714314839,-2.40350276838367));
#39449=CARTESIAN_POINT('Ctrl Pts',(209.342,3.76694647710257,-2.419024887875));
#39450=CARTESIAN_POINT('Ctrl Pts',(209.342,3.75550080658077,-2.4344672172057));
#39451=CARTESIAN_POINT('Ctrl Pts',(209.342,3.67252965594557,-2.54641066609451));
#39452=CARTESIAN_POINT('Ctrl Pts',(209.342,3.58451278293967,-2.65424350219139));
#39453=CARTESIAN_POINT('Ctrl Pts',(209.342,3.49179622102669,-2.75766463405047));
#39454=CARTESIAN_POINT('Ctrl Pts',(209.342,3.40200182763164,-2.85782621907811));
#39455=CARTESIAN_POINT('Ctrl Pts',(209.342,3.30779847052118,-2.95385016824527));
#39456=CARTESIAN_POINT('Ctrl Pts',(209.342,3.20946275289611,-3.04542604497319));
#39457=CARTESIAN_POINT('Ctrl Pts',(209.342,3.11197569393019,-3.1362116019411));
#39458=CARTESIAN_POINT('Ctrl Pts',(209.342,3.01042667809337,-3.22262598770536));
#39459=CARTESIAN_POINT('Ctrl Pts',(209.342,2.90505802513543,-3.30432364681823));
#39460=CARTESIAN_POINT('Ctrl Pts',(209.342,2.80190849661856,-3.38430070623636));
#39461=CARTESIAN_POINT('Ctrl Pts',(209.342,2.69509794498561,-3.45975793435593));
#39462=CARTESIAN_POINT('Ctrl Pts',(209.342,2.58483637303122,-3.53032417801676));
#39463=CARTESIAN_POINT('Ctrl Pts',(209.342,2.56941120866939,-3.5401961205945));
#39464=CARTESIAN_POINT('Ctrl Pts',(209.342,2.55391848441358,-3.54997226108128));
#39465=CARTESIAN_POINT('Ctrl Pts',(209.342,2.53835875722666,-3.5596515025506));
#39466=CARTESIAN_POINT('Origin',(209.342,0.,0.));
#39467=CARTESIAN_POINT('Origin',(207.493410108095,0.,0.));
#39468=CARTESIAN_POINT('Ctrl Pts',(209.342,2.5383587572263,-3.55965150255085));
#39469=CARTESIAN_POINT('Ctrl Pts',(209.368396523686,3.12874208667276,-3.13865391518958));
#39470=CARTESIAN_POINT('Ctrl Pts',(209.421189571058,4.09533550545485,-1.99754846162188));
#39471=CARTESIAN_POINT('Ctrl Pts',(209.500379142115,4.55219349719505,0.199542953564506));
#39472=CARTESIAN_POINT('Ctrl Pts',(209.579568713173,3.90500385774559,2.34791981561545));
#39473=CARTESIAN_POINT('Ctrl Pts',(209.65875828423,2.31088729255791,3.92708782806959));
#39474=CARTESIAN_POINT('Ctrl Pts',(209.737947855288,0.156348682839113,4.55384789993644));
#39475=CARTESIAN_POINT('Ctrl Pts',(209.817137426345,-2.03609361756371,4.07632219349179));
#39476=CARTESIAN_POINT('Ctrl Pts',(209.896326997403,-3.73478222633324,2.61025841618883));
#39477=CARTESIAN_POINT('Ctrl Pts',(209.955084557986,-4.32316955247597,1.05279137782476));
#39478=CARTESIAN_POINT('Ctrl Pts',(209.987445594884,-4.37218337323086,0.16395346347465));
#39479=CARTESIAN_POINT('Ctrl Pts',(209.993410108095,-4.37201596611874,0.000111980929712943));
#39480=CARTESIAN_POINT('Ctrl Pts',(209.012910346562,2.86929757049685,-4.02374147429241));
#39481=CARTESIAN_POINT('Ctrl Pts',(209.039306870248,3.53665219403857,-3.5478562783319));
#39482=CARTESIAN_POINT('Ctrl Pts',(209.09209991762,4.62926534033801,-2.25797907075377));
#39483=CARTESIAN_POINT('Ctrl Pts',(209.171289488677,5.14568624499954,0.225558388955994));
#39484=CARTESIAN_POINT('Ctrl Pts',(209.250479059734,4.41411918229158,2.6540301300941));
#39485=CARTESIAN_POINT('Ctrl Pts',(209.329668630792,2.61216948760781,4.43908235277214));
#39486=CARTESIAN_POINT('Ctrl Pts',(209.40885820185,0.176732660244985,5.14755634068753));
#39487=CARTESIAN_POINT('Ctrl Pts',(209.488047772907,-2.30154955580963,4.60777316565336));
#39488=CARTESIAN_POINT('Ctrl Pts',(209.567237343965,-4.22170488621655,2.95057115571943));
#39489=CARTESIAN_POINT('Ctrl Pts',(209.646426915022,-5.11808070198921,0.577855556617751));
#39490=CARTESIAN_POINT('Ctrl Pts',(209.72561648608,-4.77330727068225,-1.93499613460064));
#39491=CARTESIAN_POINT('Ctrl Pts',(209.804806057137,-3.27099124539652,-3.97860317407427));
#39492=CARTESIAN_POINT('Ctrl Pts',(209.883995628195,-0.975449900320081,
-5.0573874425955));
#39493=CARTESIAN_POINT('Ctrl Pts',(209.963185199253,1.55664124071889,-4.90973897055166));
#39494=CARTESIAN_POINT('Ctrl Pts',(210.04237477031,3.71124194048778,-3.57146363727227));
#39495=CARTESIAN_POINT('Ctrl Pts',(210.121564341368,4.96585488056877,-1.367097089327));
#39496=CARTESIAN_POINT('Ctrl Pts',(210.200753912425,5.01623244866681,1.16879473627364));
#39497=CARTESIAN_POINT('Ctrl Pts',(210.279943483483,3.85015794843245,3.42125020084859));
#39498=CARTESIAN_POINT('Ctrl Pts',(210.35913305454,1.75040808710203,4.84404176890668));
#39499=CARTESIAN_POINT('Ctrl Pts',(210.438322625598,-0.773821214563635,
5.09213804560949));
#39500=CARTESIAN_POINT('Ctrl Pts',(210.517512196655,-3.11039644948909,4.10537489980206));
#39501=CARTESIAN_POINT('Ctrl Pts',(210.596701767713,-4.69269080602413,2.12304548743095));
#39502=CARTESIAN_POINT('Ctrl Pts',(210.67589133877,-5.13699294884545,-0.374129103682252));
#39503=CARTESIAN_POINT('Ctrl Pts',(210.755080909828,-4.33555821691576,-2.78057621546455));
#39504=CARTESIAN_POINT('Ctrl Pts',(210.834270480886,-2.48273704223376,-4.51272488877181));
#39505=CARTESIAN_POINT('Ctrl Pts',(210.913460051943,-0.0278443610268617,
-5.15052364658087));
#39506=CARTESIAN_POINT('Ctrl Pts',(210.992649623001,2.43380066490539,-4.53930429317273));
#39507=CARTESIAN_POINT('Ctrl Pts',(211.071839194058,4.30524140906143,-2.82728943551745));
#39508=CARTESIAN_POINT('Ctrl Pts',(211.151028765116,5.13264763125822,-0.429648037150878));
#39509=CARTESIAN_POINT('Ctrl Pts',(211.230218336173,4.71537073190118,2.07218435551025));
#39510=CARTESIAN_POINT('Ctrl Pts',(211.309407907231,3.15460166563038,4.0715055536853));
#39511=CARTESIAN_POINT('Ctrl Pts',(211.388597478288,0.828831817984134,5.08347390668895));
#39512=CARTESIAN_POINT('Ctrl Pts',(211.467787049346,-1.69793234070152,4.86268392031491));
#39513=CARTESIAN_POINT('Ctrl Pts',(211.546976620404,-3.81294259032423,3.46267785758093));
#39514=CARTESIAN_POINT('Ctrl Pts',(211.626166191461,-5.00330232298365,1.22296157229737));
#39515=CARTESIAN_POINT('Ctrl Pts',(211.705355762519,-4.98034557634164,-1.31332672351697));
#39516=CARTESIAN_POINT('Ctrl Pts',(211.784545333576,-3.74963943333942,-3.53112917668494));
#39517=CARTESIAN_POINT('Ctrl Pts',(211.863734904634,-1.60963398715295,-4.89262174809087));
#39518=CARTESIAN_POINT('Ctrl Pts',(211.942924475691,0.92071274088747,-5.06763822616188));
#39519=CARTESIAN_POINT('Ctrl Pts',(212.022114046749,3.22778374639364,-4.01373656696683));
#39520=CARTESIAN_POINT('Ctrl Pts',(212.101303617806,4.75210708679663,-1.98649122276108));
#39521=CARTESIAN_POINT('Ctrl Pts',(212.180493188864,5.1240295791979,0.522484462921665));
#39522=CARTESIAN_POINT('Ctrl Pts',(212.259682759921,4.25335885465338,2.9047560303804));
#39523=CARTESIAN_POINT('Ctrl Pts',(212.338872330979,2.3512352900462,4.5826151653102));
#39524=CARTESIAN_POINT('Ctrl Pts',(212.418061902037,-0.121070194414848,
5.14917577389955));
#39525=CARTESIAN_POINT('Ctrl Pts',(212.497251473094,-2.56401577764407,4.46704513459198));
#39526=CARTESIAN_POINT('Ctrl Pts',(212.576441044152,-4.38517950653409,2.70164206325766));
#39527=CARTESIAN_POINT('Ctrl Pts',(212.655630615209,-5.1429234745331,0.281082332397397));
#39528=CARTESIAN_POINT('Ctrl Pts',(212.734820186267,-4.65349239680834,-2.20764074417387));
#39529=CARTESIAN_POINT('Ctrl Pts',(212.814009757324,-3.03557484217919,-4.16100402787818));
#39530=CARTESIAN_POINT('Ctrl Pts',(212.893199328382,-0.68152088354947,-5.10531080618757));
#39531=CARTESIAN_POINT('Ctrl Pts',(212.972388899439,1.83780402326983,-4.81156372861701));
#39532=CARTESIAN_POINT('Ctrl Pts',(213.051578470497,3.91145570004733,-3.35099738123695));
#39533=CARTESIAN_POINT('Ctrl Pts',(213.130768041555,5.03656712229653,-1.07780367650663));
#39534=CARTESIAN_POINT('Ctrl Pts',(213.209957612612,4.94029524725464,1.45676079451735));
#39535=CARTESIAN_POINT('Ctrl Pts',(213.28914718367,3.64598630605882,3.638056211567));
#39536=CARTESIAN_POINT('Ctrl Pts',(213.368336754727,1.46751426959545,4.93711160609353));
#39537=CARTESIAN_POINT('Ctrl Pts',(213.447526325785,-1.06683457221922,5.03890197741606));
#39538=CARTESIAN_POINT('Ctrl Pts',(213.526715896842,-3.34247268987556,3.91874284177026));
#39539=CARTESIAN_POINT('Ctrl Pts',(213.6059054679,-4.80755071452867,1.84827629691139));
#39540=CARTESIAN_POINT('Ctrl Pts',(213.685095038957,-5.10678263785396,-0.670403037137365));
#39541=CARTESIAN_POINT('Ctrl Pts',(213.764284610015,-4.16760378151171,-3.02650753556288));
#39542=CARTESIAN_POINT('Ctrl Pts',(213.843474181072,-2.21776795885376,-4.64867448023318));
#39543=CARTESIAN_POINT('Ctrl Pts',(213.92266375213,0.269883537940656,-5.14352330785409));
#39544=CARTESIAN_POINT('Ctrl Pts',(214.001853323188,2.69208743174467,-4.39105162829271));
#39545=CARTESIAN_POINT('Ctrl Pts',(214.081042894245,4.46145169408141,-2.5737361799275));
#39546=CARTESIAN_POINT('Ctrl Pts',(214.160232465303,5.14889995122897,-0.132281649233546));
#39547=CARTESIAN_POINT('Ctrl Pts',(214.23942203636,4.58772384834088,2.34125159559026));
#39548=CARTESIAN_POINT('Ctrl Pts',(214.318611607418,2.91401034748148,4.24702399772599));
#39549=CARTESIAN_POINT('Ctrl Pts',(214.397801178475,0.533640213219658,5.12287978243923));
#39550=CARTESIAN_POINT('Ctrl Pts',(214.476990749533,-1.97613934364353,4.75642117952077));
#39551=CARTESIAN_POINT('Ctrl Pts',(214.55618032059,-4.00669892212876,3.236515547607));
#39552=CARTESIAN_POINT('Ctrl Pts',(214.635369891648,-5.06562146651227,0.931744761455457));
#39553=CARTESIAN_POINT('Ctrl Pts',(214.714559462705,-4.89611494415949,-1.59897704676074));
#39554=CARTESIAN_POINT('Ctrl Pts',(214.793749033763,-3.53928521748753,-3.74194191453633));
#39555=CARTESIAN_POINT('Ctrl Pts',(214.87293860482,-1.3241677436213,-4.97747415153937));
#39556=CARTESIAN_POINT('Ctrl Pts',(214.952128175878,1.21206455421126,-5.00595332168752));
#39557=CARTESIAN_POINT('Ctrl Pts',(215.031317746935,3.45436740251883,-3.82047313704794));
#39558=CARTESIAN_POINT('Ctrl Pts',(215.110507317993,4.85897533965053,-1.70851625428545));
#39559=CARTESIAN_POINT('Ctrl Pts',(215.189696889051,5.08526654284531,0.817761169723606));
#39560=CARTESIAN_POINT('Ctrl Pts',(215.268886460108,4.07836468678181,3.14572894956014));
#39561=CARTESIAN_POINT('Ctrl Pts',(215.348076031166,2.08244662429357,4.7108476094497));
#39562=CARTESIAN_POINT('Ctrl Pts',(215.427265602223,-0.418471264991916,
5.13357097378284));
#39563=CARTESIAN_POINT('Ctrl Pts',(215.506455173281,-2.81790856222995,4.31138730310799));
#39564=CARTESIAN_POINT('Ctrl Pts',(215.585644744339,-4.53399420989599,2.44367871192578));
#39565=CARTESIAN_POINT('Ctrl Pts',(215.664834315396,-5.15057206514796,-0.0166296183682295));
#39566=CARTESIAN_POINT('Ctrl Pts',(215.744023886454,-4.51812006750333,-2.47290521413848));
#39567=CARTESIAN_POINT('Ctrl Pts',(215.823213457511,-2.79000980667881,-4.32949355249846));
#39568=CARTESIAN_POINT('Ctrl Pts',(215.902403028569,-0.385313431858017,
-5.1361661481809));
#39569=CARTESIAN_POINT('Ctrl Pts',(215.981592599626,2.11282265665386,-4.697302370938));
#39570=CARTESIAN_POINT('Ctrl Pts',(216.060782170684,4.09859263540988,-3.11932806088965));
#39571=CARTESIAN_POINT('Ctrl Pts',(216.139971741741,5.09044106686257,-0.784906929061443));
#39572=CARTESIAN_POINT('Ctrl Pts',(216.219161312799,4.8478416007807,1.73985659070789));
#39573=CARTESIAN_POINT('Ctrl Pts',(216.298350883857,3.42962536729897,3.84269943951761));
#39574=CARTESIAN_POINT('Ctrl Pts',(216.377540454914,1.1797142436527,5.01367564226213));
#39575=CARTESIAN_POINT('Ctrl Pts',(216.456730025972,-1.35628127791517,4.96881980330002));
#39576=CARTESIAN_POINT('Ctrl Pts',(216.535919597029,-3.56337434289889,3.71900960402894));
#39577=CARTESIAN_POINT('Ctrl Pts',(216.615109168087,-4.90633797234996,1.56732793108732));
#39578=CARTESIAN_POINT('Ctrl Pts',(216.694298739144,-5.05949928113605,-0.964435672646684));
#39579=CARTESIAN_POINT('Ctrl Pts',(216.773488310202,-3.98571617230891,-3.26232060599274));
#39580=CARTESIAN_POINT('Ctrl Pts',(216.852677881259,-1.94538441191105,-4.76908257764353));
#39581=CARTESIAN_POINT('Ctrl Pts',(216.931867452317,0.566709159622022,-5.11932709160981));
#39582=CARTESIAN_POINT('Ctrl Pts',(217.011057023375,2.94137398550808,-4.22811875659447));
#39583=CARTESIAN_POINT('Ctrl Pts',(217.090246594432,4.60274641009122,-2.31157838432574));
#39584=CARTESIAN_POINT('Ctrl Pts',(217.169436165489,5.14793841844104,0.165526983988809));
#39585=CARTESIAN_POINT('Ctrl Pts',(217.248625736547,4.44473924146695,2.60249154039997));
#39586=CARTESIAN_POINT('Ctrl Pts',(217.327815307605,2.66367688139153,4.4083437495311));
#39587=CARTESIAN_POINT('Ctrl Pts',(217.407004878662,0.236664537266517,5.14515879631426));
#39588=CARTESIAN_POINT('Ctrl Pts',(217.48619444972,-2.24773969817247,4.63425672484263));
#39589=CARTESIAN_POINT('Ctrl Pts',(217.565384020777,-4.18706001884488,2.99953288714764));
#39590=CARTESIAN_POINT('Ctrl Pts',(217.644573591835,-5.11100517472834,0.637412932399219));
#39591=CARTESIAN_POINT('Ctrl Pts',(217.723763162892,-4.79551557253093,-1.87928165427725));
#39592=CARTESIAN_POINT('Ctrl Pts',(217.80295273395,-3.3170984286237,-3.94024455552087));
#39593=CARTESIAN_POINT('Ctrl Pts',(217.882142305007,-1.03427452951688,-5.04568581464227));
#39594=CARTESIAN_POINT('Ctrl Pts',(217.961331876065,1.49936418144328,-4.92753246502694));
#39595=CARTESIAN_POINT('Ctrl Pts',(218.040521447122,3.66940238370292,-3.61443706390981));
#39596=CARTESIAN_POINT('Ctrl Pts',(218.11971101818,4.94959901854762,-1.42482935753097));
#39597=CARTESIAN_POINT('Ctrl Pts',(218.198900589237,5.02950239356853,1.11030392937163));
#39598=CARTESIAN_POINT('Ctrl Pts',(218.278090160295,3.88973569013542,3.37618503689836));
#39599=CARTESIAN_POINT('Ctrl Pts',(218.357279731353,1.80669590258578,4.82333070171115));
#39600=CARTESIAN_POINT('Ctrl Pts',(218.436469302411,-0.714473298336281,
5.10080356889521));
#39601=CARTESIAN_POINT('Ctrl Pts',(218.515658873468,-3.06238048730475,4.14131559935545));
#39602=CARTESIAN_POINT('Ctrl Pts',(218.594848444525,-4.66765081939779,2.17754562998453));
#39603=CARTESIAN_POINT('Ctrl Pts',(218.674038015583,-5.14100121277669,-0.3142859728308));
#39604=CARTESIAN_POINT('Ctrl Pts',(218.753227586641,-4.36764271492659,-2.72990224316519));
#39605=CARTESIAN_POINT('Ctrl Pts',(218.832417157698,-2.53511718306022,-4.48350867185984));
#39606=CARTESIAN_POINT('Ctrl Pts',(218.911606728756,-0.0878177965264293,
-5.14985020919084));
#39607=CARTESIAN_POINT('Ctrl Pts',(218.990796299813,2.38077768063373,-4.56733694595503));
#39608=CARTESIAN_POINT('Ctrl Pts',(219.069985870871,4.27202711572156,-2.8772301724105));
#39609=CARTESIAN_POINT('Ctrl Pts',(219.149175441928,5.12729659898502,-0.48938607308168));
#39610=CARTESIAN_POINT('Ctrl Pts',(219.228365012986,4.73918060277484,2.0171356812997));
#39611=CARTESIAN_POINT('Ctrl Pts',(219.307554584043,3.20179847141267,4.03449571705674));
#39612=CARTESIAN_POINT('Ctrl Pts',(219.386744155101,0.887970185493443,5.07347790890671));
#39613=CARTESIAN_POINT('Ctrl Pts',(219.465933726158,-1.64119365075591,4.88212582214021));
#39614=CARTESIAN_POINT('Ctrl Pts',(219.545123297216,-3.77236288791018,3.5068429369459));
#39615=CARTESIAN_POINT('Ctrl Pts',(219.624312868273,-4.9887223129969,1.28113965916958));
#39616=CARTESIAN_POINT('Ctrl Pts',(219.703502439331,-4.99530095685557,-1.25524399736708));
#39617=CARTESIAN_POINT('Ctrl Pts',(219.782692010389,-3.79050347775281,-3.48722705421306));
#39618=CARTESIAN_POINT('Ctrl Pts',(219.861881581446,-1.66649703674374,-4.87354663145974));
#39619=CARTESIAN_POINT('Ctrl Pts',(219.941071152504,0.861640153687791,-5.07801589088088));
#39620=CARTESIAN_POINT('Ctrl Pts',(220.020260723561,3.18082690895062,-4.05105039684845));
#39621=CARTESIAN_POINT('Ctrl Pts',(220.099450294619,4.72865317920565,-2.0416924972233));
#39622=CARTESIAN_POINT('Ctrl Pts',(220.178639865676,5.12976624751329,0.462782225775264));
#39623=CARTESIAN_POINT('Ctrl Pts',(220.257829436734,4.2868949387905,2.85503080999931));
#39624=CARTESIAN_POINT('Ctrl Pts',(220.337019007791,2.40443818471475,4.55492548331974));
#39625=CARTESIAN_POINT('Ctrl Pts',(220.416208578849,-0.0611023580090773,
5.15023646491014));
#39626=CARTESIAN_POINT('Ctrl Pts',(220.495398149907,-2.51182538706132,4.49659897765337));
#39627=CARTESIAN_POINT('Ctrl Pts',(220.574587720964,-4.35342289604155,2.75252215901591));
#39628=CARTESIAN_POINT('Ctrl Pts',(220.653777292022,-5.13930171919711,0.340950098053002));
#39629=CARTESIAN_POINT('Ctrl Pts',(220.732966863079,-4.67888378875926,-2.15330342868111));
#39630=CARTESIAN_POINT('Ctrl Pts',(220.812156434137,-3.08382187849219,-4.12537413289167));
#39631=CARTESIAN_POINT('Ctrl Pts',(220.891346005194,-0.740923529936072,
-5.09702869025692));
#39632=CARTESIAN_POINT('Ctrl Pts',(220.970535576252,1.78165114356852,-4.83263783619408));
#39633=CARTESIAN_POINT('Ctrl Pts',(221.049725147309,3.87216973211928,-3.39631716377015));
#39634=CARTESIAN_POINT('Ctrl Pts',(221.128914718367,5.02367525731088,-1.13637896919977));
#39635=CARTESIAN_POINT('Ctrl Pts',(221.208104289424,4.9569233337539,1.39913473529202));
#39636=CARTESIAN_POINT('Ctrl Pts',(221.287293860482,3.6881029769245,3.59535377575949));
#39637=CARTESIAN_POINT('Ctrl Pts',(221.36648343154,1.52490398573333,4.91968850138736));
#39638=CARTESIAN_POINT('Ctrl Pts',(221.445673002597,-1.00808450753534,5.05098286642663));
#39639=CARTESIAN_POINT('Ctrl Pts',(221.524862573655,-3.2966188845772,3.95739912490663));
#39640=CARTESIAN_POINT('Ctrl Pts',(221.604052144712,-4.78569263413133,1.90413148846678));
#39641=CARTESIAN_POINT('Ctrl Pts',(221.68324171577,-5.11426397585892,-0.610889148630078));
#39642=CARTESIAN_POINT('Ctrl Pts',(221.762431286827,-4.20251954963569,-2.97777660711001));
#39643=CARTESIAN_POINT('Ctrl Pts',(221.841620857885,-2.27184811611898,-4.62251767504382));
#39644=CARTESIAN_POINT('Ctrl Pts',(221.920810428943,0.210147207048501,-5.14630014929042));
#39645=CARTESIAN_POINT('Ctrl Pts',(221.973603476314,1.83010136182592,-4.66325228984448));
#39646=CARTESIAN_POINT('Ctrl Pts',(222.,2.53382212491006,-4.24300712223256));
#39647=CARTESIAN_POINT('Ctrl Pts',(209.122606897708,2.75898463274,-3.86904481704522));
#39648=CARTESIAN_POINT('Ctrl Pts',(209.149003421394,3.40068215824997,-3.41145549061779));
#39649=CARTESIAN_POINT('Ctrl Pts',(209.201796468766,4.45128872871029,-2.17116886770981));
#39650=CARTESIAN_POINT('Ctrl Pts',(209.280986039823,4.94785532906471,0.216886577158832));
#39651=CARTESIAN_POINT('Ctrl Pts',(209.360175610881,4.24441407410958,2.55199335860121));
#39652=CARTESIAN_POINT('Ctrl Pts',(209.439365181938,2.51174208925784,4.26841751120462));
#39653=CARTESIAN_POINT('Ctrl Pts',(209.518554752996,0.169938001109696,4.94965352710383));
#39654=CARTESIAN_POINT('Ctrl Pts',(209.597744324053,-2.21306424306099,4.43062284159951));
#39655=CARTESIAN_POINT('Ctrl Pts',(209.676933895111,-4.05939733292211,2.83713357587589));
#39656=CARTESIAN_POINT('Ctrl Pts',(209.756123466168,-4.92131110802362,0.555639337322439));
#39657=CARTESIAN_POINT('Ctrl Pts',(209.835313037226,-4.58979282684784,-1.86060332489322));
#39658=CARTESIAN_POINT('Ctrl Pts',(209.914502608283,-3.14523480334363,-3.82564190271164));
#39659=CARTESIAN_POINT('Ctrl Pts',(209.993692179341,-0.937947779506468,
-4.86295126005946));
#39660=CARTESIAN_POINT('Ctrl Pts',(210.072881750399,1.49679465315585,-4.72097927722814));
#39661=CARTESIAN_POINT('Ctrl Pts',(210.152071321456,3.56855963197046,-3.43415524166689));
#39662=CARTESIAN_POINT('Ctrl Pts',(210.231260892514,4.77493775646759,-1.31453771114566));
#39663=CARTESIAN_POINT('Ctrl Pts',(210.310450463571,4.8233785099281,1.12385928506119));
#39664=CARTESIAN_POINT('Ctrl Pts',(210.389640034629,3.70213487878409,3.2897169070078));
#39665=CARTESIAN_POINT('Ctrl Pts',(210.468829605686,1.6831119445384,4.65780786844285));
#39666=CARTESIAN_POINT('Ctrl Pts',(210.548019176744,-0.744070904817171,
4.89636584231815));
#39667=CARTESIAN_POINT('Ctrl Pts',(210.627208747802,-2.99081423067021,3.94753976605815));
#39668=CARTESIAN_POINT('Ctrl Pts',(210.706398318859,-4.51227574063673,2.04142293732736));
#39669=CARTESIAN_POINT('Ctrl Pts',(210.785587889917,-4.93949625514236,-0.359745346155024));
#39670=CARTESIAN_POINT('Ctrl Pts',(210.864777460974,-4.16887346151025,-2.67367425655354));
#39671=CARTESIAN_POINT('Ctrl Pts',(210.943967032032,-2.38728580022152,-4.33922878823222));
#39672=CARTESIAN_POINT('Ctrl Pts',(211.023156603089,-0.0267738574665273,
-4.95250675203405));
#39673=CARTESIAN_POINT('Ctrl Pts',(211.102346174147,2.34023082954886,-4.36478632156147));
#39674=CARTESIAN_POINT('Ctrl Pts',(211.181535745204,4.13972221284094,-2.71859154139596));
#39675=CARTESIAN_POINT('Ctrl Pts',(211.260725316262,4.93531799751903,-0.41312980019039));
#39676=CARTESIAN_POINT('Ctrl Pts',(211.339914887319,4.53408371468927,1.99251721112601));
#39677=CARTESIAN_POINT('Ctrl Pts',(211.419104458377,3.03331993425243,3.91497255991756));
#39678=CARTESIAN_POINT('Ctrl Pts',(211.498294029434,0.796966572047865,4.88803480465114));
#39679=CARTESIAN_POINT('Ctrl Pts',(211.577483600492,-1.63265367928241,4.67573330419596));
#39680=CARTESIAN_POINT('Ctrl Pts',(211.656673171549,-3.6663503013397,3.32955183715591));
#39681=CARTESIAN_POINT('Ctrl Pts',(211.735862742607,-4.8109454955116,1.17594362435392));
#39682=CARTESIAN_POINT('Ctrl Pts',(211.815052313665,-4.78887134333782,-1.26283459938339));
#39683=CARTESIAN_POINT('Ctrl Pts',(211.894241884722,-3.60548089583749,-3.39537147867399));
#39684=CARTESIAN_POINT('Ctrl Pts',(211.97343145578,-1.54775004187592,-4.70452014304488));
#39685=CARTESIAN_POINT('Ctrl Pts',(212.052621026837,0.885315043443409,-4.87280794227463));
#39686=CARTESIAN_POINT('Ctrl Pts',(212.131810597895,3.10368845869336,-3.85942455811946));
#39687=CARTESIAN_POINT('Ctrl Pts',(212.211000168952,4.56940770466565,-1.91011863426965));
#39688=CARTESIAN_POINT('Ctrl Pts',(212.29018974001,4.92703127485804,0.502397039215665));
#39689=CARTESIAN_POINT('Ctrl Pts',(212.369379311067,4.08983433373387,2.79307985762196));
#39690=CARTESIAN_POINT('Ctrl Pts',(212.448568882125,2.26083976088618,4.40643206506557));
#39691=CARTESIAN_POINT('Ctrl Pts',(212.527758453183,-0.116415532954153,
4.95121069962984));
#39692=CARTESIAN_POINT('Ctrl Pts',(212.60694802424,-2.46543969554121,4.29530523666149));
#39693=CARTESIAN_POINT('Ctrl Pts',(212.686137595298,-4.2165870123533,2.59777480465405));
#39694=CARTESIAN_POINT('Ctrl Pts',(212.765327166355,-4.94519877599783,0.270275848553698));
#39695=CARTESIAN_POINT('Ctrl Pts',(212.844516737413,-4.47458435241465,-2.12276584708909));
#39696=CARTESIAN_POINT('Ctrl Pts',(212.92370630847,-2.91886921287646,-4.00103017816211));
#39697=CARTESIAN_POINT('Ctrl Pts',(213.002895879528,-0.655319149863825,
-4.90903216329489));
#39698=CARTESIAN_POINT('Ctrl Pts',(213.082085450585,1.76714785887865,-4.62657847802267));
#39699=CARTESIAN_POINT('Ctrl Pts',(213.161275021643,3.76107597867765,-3.22216502542249));
#39700=CARTESIAN_POINT('Ctrl Pts',(213.240464592701,4.84293139723859,-1.0363664651476));
#39701=CARTESIAN_POINT('Ctrl Pts',(213.319654163758,4.75036078813315,1.40075420792119));
#39702=CARTESIAN_POINT('Ctrl Pts',(213.398843734816,3.50581281391976,3.49818759962898));
#39703=CARTESIAN_POINT('Ctrl Pts',(213.478033305873,1.41109425518363,4.74729954515509));
#39704=CARTESIAN_POINT('Ctrl Pts',(213.557222876931,-1.02581907875067,4.84517648658055));
#39705=CARTESIAN_POINT('Ctrl Pts',(213.636412447988,-3.21396807411751,3.76808295914452));
#39706=CARTESIAN_POINT('Ctrl Pts',(213.715602019046,-4.62271974816679,1.77721751576748));
#39707=CARTESIAN_POINT('Ctrl Pts',(213.794791590103,-4.91044740896034,-0.644628739877947));
#39708=CARTESIAN_POINT('Ctrl Pts',(213.873981161161,-4.00737619784371,-2.91015050768815));
#39709=CARTESIAN_POINT('Ctrl Pts',(213.953170732218,-2.13250371114387,-4.46995166533147));
#39710=CARTESIAN_POINT('Ctrl Pts',(214.032360303276,0.259507602649545,-4.94577554814299));
#39711=CARTESIAN_POINT('Ctrl Pts',(214.111549874334,2.58858751024904,-4.22223337467562));
#39712=CARTESIAN_POINT('Ctrl Pts',(214.190739445391,4.28992684141539,-2.47478638749806));
#39713=CARTESIAN_POINT('Ctrl Pts',(214.269929016449,4.95094548123029,-0.127195952480322));
#39714=CARTESIAN_POINT('Ctrl Pts',(214.349118587506,4.4113443398049,2.25123989928065));
#39715=CARTESIAN_POINT('Ctrl Pts',(214.428308158564,2.80197838349493,4.08374302654674));
#39716=CARTESIAN_POINT('Ctrl Pts',(214.507497729621,0.513123895835644,4.92592568315483));
#39717=CARTESIAN_POINT('Ctrl Pts',(214.586687300679,-1.90016474322018,4.57355593789613));
#39718=CARTESIAN_POINT('Ctrl Pts',(214.665876871736,-3.85265748238687,3.11208455731049));
#39719=CARTESIAN_POINT('Ctrl Pts',(214.745066442794,-4.87086871891265,0.895922927243278));
#39720=CARTESIAN_POINT('Ctrl Pts',(214.824256013852,-4.70787903979075,-1.5375028179294));
#39721=CARTESIAN_POINT('Ctrl Pts',(214.903445584909,-3.40321395254972,-3.59807931563672));
#39722=CARTESIAN_POINT('Ctrl Pts',(214.982635155967,-1.27325882591832,-4.7861103132568));
#39723=CARTESIAN_POINT('Ctrl Pts',(215.061824727024,1.16546555273411,-4.8134945739901));
#39724=CARTESIAN_POINT('Ctrl Pts',(215.141014298082,3.32156088562718,-3.6735913288652));
#39725=CARTESIAN_POINT('Ctrl Pts',(215.220203869139,4.67216730352476,-1.64283068400737));
#39726=CARTESIAN_POINT('Ctrl Pts',(215.299393440197,4.8897585211657,0.78632154563469));
#39727=CARTESIAN_POINT('Ctrl Pts',(215.378583011254,3.92156798696623,3.02478833838726));
#39728=CARTESIAN_POINT('Ctrl Pts',(215.457772582312,2.00238493699778,4.52973448808276));
#39729=CARTESIAN_POINT('Ctrl Pts',(215.53696215337,-0.402382729915348,4.93620584124162));
#39730=CARTESIAN_POINT('Ctrl Pts',(215.616151724427,-2.70957132491234,4.14563182200913));
#39731=CARTESIAN_POINT('Ctrl Pts',(215.695341295485,-4.35968038960457,2.34972910543732));
#39732=CARTESIAN_POINT('Ctrl Pts',(215.774530866542,-4.95255330910221,-0.0159902765046303));
#39733=CARTESIAN_POINT('Ctrl Pts',(215.8537204376,-4.34441654406633,-2.37783196632661));
#39734=CARTESIAN_POINT('Ctrl Pts',(215.932910008657,-2.68274516417193,-4.16304195901916));
#39735=CARTESIAN_POINT('Ctrl Pts',(216.012099579715,-0.370499681948449,
-4.93870124163409));
#39736=CARTESIAN_POINT('Ctrl Pts',(216.091289150772,2.0315931332293,-4.51671000944908));
#39737=CARTESIAN_POINT('Ctrl Pts',(216.17047872183,3.94101825242164,-2.99940245757741));
#39738=CARTESIAN_POINT('Ctrl Pts',(216.249668292887,4.89473410557081,-0.754730418231469));
#39739=CARTESIAN_POINT('Ctrl Pts',(216.328857863945,4.66146161208212,1.67296611069283));
#39740=CARTESIAN_POINT('Ctrl Pts',(216.408047435003,3.29777008203251,3.69496311950379));
#39741=CARTESIAN_POINT('Ctrl Pts',(216.48723700606,1.13435898135118,4.82092000243417));
#39742=CARTESIAN_POINT('Ctrl Pts',(216.566426577118,-1.3041377241305,4.7777886898587));
#39743=CARTESIAN_POINT('Ctrl Pts',(216.645616148175,-3.42637694808895,3.57602866012657));
#39744=CARTESIAN_POINT('Ctrl Pts',(216.724805719233,-4.71770903371247,1.50707048331179));
#39745=CARTESIAN_POINT('Ctrl Pts',(216.80399529029,-4.86498190691188,-0.927357004536036));
#39746=CARTESIAN_POINT('Ctrl Pts',(216.883184861348,-3.83248143480613,-3.13689751511079));
#39747=CARTESIAN_POINT('Ctrl Pts',(216.962374432405,-1.8705922147716,-4.58573055624486));
#39748=CARTESIAN_POINT('Ctrl Pts',(217.041564003463,0.544921474407914,-4.92250957898215));
#39749=CARTESIAN_POINT('Ctrl Pts',(217.120753574521,2.82828999982485,-4.06556461581078));
#39750=CARTESIAN_POINT('Ctrl Pts',(217.199943145578,4.42578934454745,-2.22270750350381));
#39751=CARTESIAN_POINT('Ctrl Pts',(217.279132716636,4.95002091550624,0.159163137983585));
#39752=CARTESIAN_POINT('Ctrl Pts',(217.358322287693,4.27385691530776,2.50243622014988));
#39753=CARTESIAN_POINT('Ctrl Pts',(217.437511858751,2.56126923115591,4.23886068348277));
#39754=CARTESIAN_POINT('Ctrl Pts',(217.516701429808,0.227565738788027,4.9473481586575));
#39755=CARTESIAN_POINT('Ctrl Pts',(217.595891000866,-2.1613231577733,4.45608821457955));
#39756=CARTESIAN_POINT('Ctrl Pts',(217.675080571923,-4.02608442119606,2.88421292588538));
#39757=CARTESIAN_POINT('Ctrl Pts',(217.754270142981,-4.91450760629484,0.61290697182538));
#39758=CARTESIAN_POINT('Ctrl Pts',(217.833459714038,-4.61114730891682,-1.80703084199222));
#39759=CARTESIAN_POINT('Ctrl Pts',(217.912649285096,-3.18956935103597,-3.7887580185826));
#39760=CARTESIAN_POINT('Ctrl Pts',(217.991838856153,-0.99451083858036,-4.85169951258196));
#39761=CARTESIAN_POINT('Ctrl Pts',(218.071028427211,1.4417196661713,-4.73808868349009));
#39762=CARTESIAN_POINT('Ctrl Pts',(218.150217998269,3.52832863766821,-3.47547651309174));
#39763=CARTESIAN_POINT('Ctrl Pts',(218.229407569326,4.75930686688351,-1.37005040610828));
#39764=CARTESIAN_POINT('Ctrl Pts',(218.308597140384,4.83613827888256,1.06761721415906));
#39765=CARTESIAN_POINT('Ctrl Pts',(218.387786711441,3.74019101568666,3.24638431714711));
#39766=CARTESIAN_POINT('Ctrl Pts',(218.466976282499,1.7372357201715,4.63789305838353));
#39767=CARTESIAN_POINT('Ctrl Pts',(218.546165853556,-0.68700467699192,4.90469821112708));
#39768=CARTESIAN_POINT('Ctrl Pts',(218.625355424614,-2.94464428888551,3.98209869043647));
#39769=CARTESIAN_POINT('Ctrl Pts',(218.704544995671,-4.4881984406674,2.09382776885602));
#39770=CARTESIAN_POINT('Ctrl Pts',(218.783734566729,-4.94335041746557,-0.302202942713887));
#39771=CARTESIAN_POINT('Ctrl Pts',(218.862924137787,-4.19972443976753,-2.62494849443971));
#39772=CARTESIAN_POINT('Ctrl Pts',(218.942113708844,-2.43765213555284,-4.3111358172153));
#39773=CARTESIAN_POINT('Ctrl Pts',(219.021303279902,-0.0844415558667597,
-4.95185920559993));
#39774=CARTESIAN_POINT('Ctrl Pts',(219.100492850959,2.28924636551427,-4.39174123172365));
#39775=CARTESIAN_POINT('Ctrl Pts',(219.179682422017,4.10778487533567,-2.76661225805234));
#39776=CARTESIAN_POINT('Ctrl Pts',(219.258871993074,4.93017269088968,-0.470571149187391));
#39777=CARTESIAN_POINT('Ctrl Pts',(219.338061564132,4.55697819190328,1.93958493677382));
#39778=CARTESIAN_POINT('Ctrl Pts',(219.417251135189,3.07870221290023,3.87938560247949));
#39779=CARTESIAN_POINT('Ctrl Pts',(219.496440706247,0.853831307459487,4.87842311273264));
#39780=CARTESIAN_POINT('Ctrl Pts',(219.575630277305,-1.57809636349497,4.69442774318297));
#39781=CARTESIAN_POINT('Ctrl Pts',(219.654819848362,-3.62733072508078,3.37201894705926));
#39782=CARTESIAN_POINT('Ctrl Pts',(219.73400941942,-4.79692602819937,1.23188499805217));
#39783=CARTESIAN_POINT('Ctrl Pts',(219.813198990477,-4.80325174969195,-1.20698492017167));
#39784=CARTESIAN_POINT('Ctrl Pts',(219.892388561535,-3.64477388229083,-3.35315721603005));
#39785=CARTESIAN_POINT('Ctrl Pts',(219.971578132592,-1.60242693618093,-4.68617838783826));
#39786=CARTESIAN_POINT('Ctrl Pts',(220.05076770365,0.828513559353387,-4.88278662757303));
#39787=CARTESIAN_POINT('Ctrl Pts',(220.129957274707,3.05853692256848,-3.89530382149409));
#39788=CARTESIAN_POINT('Ctrl Pts',(220.209146845765,4.54685550537946,-1.96319764200831));
#39789=CARTESIAN_POINT('Ctrl Pts',(220.288336416822,4.9325473913766,0.444990112683956));
#39790=CARTESIAN_POINT('Ctrl Pts',(220.36752598788,4.12208109047601,2.74526637173549));
#39791=CARTESIAN_POINT('Ctrl Pts',(220.446715558938,2.31199721848734,4.37980693984934));
#39792=CARTESIAN_POINT('Ctrl Pts',(220.525905129995,-0.0587532183851061,
4.95223061134216));
#39793=CARTESIAN_POINT('Ctrl Pts',(220.605094701053,-2.41525581532081,4.32372285346192));
#39794=CARTESIAN_POINT('Ctrl Pts',(220.68428427211,-4.18605131565955,2.64669876560978));
#39795=CARTESIAN_POINT('Ctrl Pts',(220.763473843168,-4.94171626257075,0.327841939689966));
#39796=CARTESIAN_POINT('Ctrl Pts',(220.842663414225,-4.49899954758883,-2.07051758257643));
#39797=CARTESIAN_POINT('Ctrl Pts',(220.921852985283,-2.96526134492004,-3.96677010916658));
#39798=CARTESIAN_POINT('Ctrl Pts',(221.00104255634,-0.712438003694083,-4.90106846137209));
#39799=CARTESIAN_POINT('Ctrl Pts',(221.080232127398,1.7131538312905,-4.64684237102271));
#39800=CARTESIAN_POINT('Ctrl Pts',(221.159421698455,3.72330039802324,-3.2657424448069));
#39801=CARTESIAN_POINT('Ctrl Pts',(221.238611269513,4.83053517254985,-1.09268977370239));
#39802=CARTESIAN_POINT('Ctrl Pts',(221.317800840571,4.76634959166299,1.34534363862965));
#39803=CARTESIAN_POINT('Ctrl Pts',(221.396990411628,3.54631026838228,3.45712690052796));
#39804=CARTESIAN_POINT('Ctrl Pts',(221.476179982686,1.46627756782774,4.73054628866709));
#39805=CARTESIAN_POINT('Ctrl Pts',(221.555369553743,-0.969327717484422,
4.8567929140549));
#39806=CARTESIAN_POINT('Ctrl Pts',(221.634559124801,-3.1698771629929,3.80525306385193));
#39807=CARTESIAN_POINT('Ctrl Pts',(221.713748695858,-4.60170202294458,1.83092530012021));
#39808=CARTESIAN_POINT('Ctrl Pts',(221.792938266916,-4.91764111964419,-0.587402920738604));
#39809=CARTESIAN_POINT('Ctrl Pts',(221.872127837973,-4.04094959527899,-2.86329308720899));
#39810=CARTESIAN_POINT('Ctrl Pts',(221.951317409031,-2.18450470412734,-4.44480048397577));
#39811=CARTESIAN_POINT('Ctrl Pts',(222.030506980089,0.202067893139325,-4.94844563120763));
#39812=CARTESIAN_POINT('Ctrl Pts',(222.08330002746,1.75974133375087,-4.48396901686381));
#39813=CARTESIAN_POINT('Ctrl Pts',(222.109696551146,2.43640686717375,-4.07988058374122));
#39814=CARTESIAN_POINT('Ctrl Pts',(209.232303448854,2.64867169498315,-3.71434815979804));
#39815=CARTESIAN_POINT('Ctrl Pts',(209.25869997254,3.26471212246136,-3.27505470290369));
#39816=CARTESIAN_POINT('Ctrl Pts',(209.311493019912,4.27331211708257,-2.08435866466584));
#39817=CARTESIAN_POINT('Ctrl Pts',(209.390682590969,4.75002441312988,0.208214765361669));
#39818=CARTESIAN_POINT('Ctrl Pts',(209.469872162027,4.07470896592758,2.44995658710833));
#39819=CARTESIAN_POINT('Ctrl Pts',(209.549061733084,2.41131469090788,4.09775266963711));
#39820=CARTESIAN_POINT('Ctrl Pts',(209.628251304142,0.163143341974401,4.75175071352013));
#39821=CARTESIAN_POINT('Ctrl Pts',(209.707440875199,-2.12457893031235,4.25347251754565));
#39822=CARTESIAN_POINT('Ctrl Pts',(209.786630446257,-3.89708977962767,2.72369599603236));
#39823=CARTESIAN_POINT('Ctrl Pts',(209.865820017314,-4.72454151405803,0.533423118027127));
#39824=CARTESIAN_POINT('Ctrl Pts',(209.945009588372,-4.40627838301343,-1.7862105151858));
#39825=CARTESIAN_POINT('Ctrl Pts',(210.02419915943,-3.01947836129074,-3.67268063134902));
#39826=CARTESIAN_POINT('Ctrl Pts',(210.103388730487,-0.900445658692855,
-4.66851507752341));
#39827=CARTESIAN_POINT('Ctrl Pts',(210.182578301545,1.43694806559282,-4.53221958390462));
#39828=CARTESIAN_POINT('Ctrl Pts',(210.261767872602,3.42587732345312,-3.29684684606151));
#39829=CARTESIAN_POINT('Ctrl Pts',(210.34095744366,4.5840206323664,-1.26197833296432));
#39830=CARTESIAN_POINT('Ctrl Pts',(210.420147014717,4.63052457118939,1.07892383384874));
#39831=CARTESIAN_POINT('Ctrl Pts',(210.499336585775,3.55411180913573,3.15818361316701));
#39832=CARTESIAN_POINT('Ctrl Pts',(210.578526156832,1.61581580197477,4.47157396797902));
#39833=CARTESIAN_POINT('Ctrl Pts',(210.65771572789,-0.714320595070703,4.7005936390268));
#39834=CARTESIAN_POINT('Ctrl Pts',(210.736905298947,-2.87123201185134,3.78970463231423));
#39835=CARTESIAN_POINT('Ctrl Pts',(210.816094870005,-4.33186067524932,1.95980038722377));
#39836=CARTESIAN_POINT('Ctrl Pts',(210.895284441062,-4.74199956143928,-0.345361588627793));
#39837=CARTESIAN_POINT('Ctrl Pts',(210.97447401212,-4.00218870610474,-2.56677229764253));
#39838=CARTESIAN_POINT('Ctrl Pts',(211.053663583178,-2.29183455820929,-4.16573268769264));
#39839=CARTESIAN_POINT('Ctrl Pts',(211.132853154235,-0.0257033539061957,
-4.75448985748724));
#39840=CARTESIAN_POINT('Ctrl Pts',(211.212042725293,2.24666099419233,-4.19026834995021));
#39841=CARTESIAN_POINT('Ctrl Pts',(211.29123229635,3.97420301662046,-2.60989364727448));
#39842=CARTESIAN_POINT('Ctrl Pts',(211.370421867408,4.73798836377985,-0.396611563229904));
#39843=CARTESIAN_POINT('Ctrl Pts',(211.449611438465,4.35279669747736,1.91285006674178));
#39844=CARTESIAN_POINT('Ctrl Pts',(211.528801009523,2.91203820287448,3.75843956614982));
#39845=CARTESIAN_POINT('Ctrl Pts',(211.60799058058,0.765101326111594,4.69259570261332));
#39846=CARTESIAN_POINT('Ctrl Pts',(211.687180151638,-1.5673750178633,4.48878268807701));
#39847=CARTESIAN_POINT('Ctrl Pts',(211.766369722695,-3.51975801235516,3.1964258167309));
#39848=CARTESIAN_POINT('Ctrl Pts',(211.845559293753,-4.61858866803955,1.12892567641046));
#39849=CARTESIAN_POINT('Ctrl Pts',(211.924748864811,-4.59739711033398,-1.21234247524981));
#39850=CARTESIAN_POINT('Ctrl Pts',(212.003938435868,-3.46132235833556,-3.25961378066305));
#39851=CARTESIAN_POINT('Ctrl Pts',(212.083128006926,-1.48586609659888,-4.5164185379989));
#39852=CARTESIAN_POINT('Ctrl Pts',(212.162317577983,0.849917345999346,-4.67797765838739));
#39853=CARTESIAN_POINT('Ctrl Pts',(212.241507149041,2.97959317099309,-3.70511254927208));
#39854=CARTESIAN_POINT('Ctrl Pts',(212.320696720098,4.38670832253466,-1.83374604577822));
#39855=CARTESIAN_POINT('Ctrl Pts',(212.399886291156,4.73003297051818,0.482309615509662));
#39856=CARTESIAN_POINT('Ctrl Pts',(212.479075862213,3.92630981281437,2.68140368486352));
#39857=CARTESIAN_POINT('Ctrl Pts',(212.558265433271,2.17044423172616,4.23024896482096));
#39858=CARTESIAN_POINT('Ctrl Pts',(212.637455004329,-0.111760871493455,
4.75324562536013));
#39859=CARTESIAN_POINT('Ctrl Pts',(212.716644575386,-2.36686361343836,4.12356533873099));
#39860=CARTESIAN_POINT('Ctrl Pts',(212.795834146444,-4.04799451817251,2.49390754605045));
#39861=CARTESIAN_POINT('Ctrl Pts',(212.875023717501,-4.74747407746257,0.259469364709995));
#39862=CARTESIAN_POINT('Ctrl Pts',(212.954213288559,-4.29567630802097,-2.03789095000431));
#39863=CARTESIAN_POINT('Ctrl Pts',(213.033402859616,-2.80216358357373,-3.84105632844604));
#39864=CARTESIAN_POINT('Ctrl Pts',(213.112592430674,-0.629117416178179,
-4.71275352040221));
#39865=CARTESIAN_POINT('Ctrl Pts',(213.191782001732,1.69649169448747,-4.44159322742832));
#39866=CARTESIAN_POINT('Ctrl Pts',(213.270971572789,3.61069625730797,-3.09333266960803));
#39867=CARTESIAN_POINT('Ctrl Pts',(213.350161143847,4.64929567218066,-0.994929253788572));
#39868=CARTESIAN_POINT('Ctrl Pts',(213.429350714904,4.56042632901166,1.34474762132502));
#39869=CARTESIAN_POINT('Ctrl Pts',(213.508540285962,3.3656393217807,3.35831898769097));
#39870=CARTESIAN_POINT('Ctrl Pts',(213.587729857019,1.35467424077182,4.55748748421665));
#39871=CARTESIAN_POINT('Ctrl Pts',(213.666919428077,-0.984803585282112,
4.65145099574505));
#39872=CARTESIAN_POINT('Ctrl Pts',(213.746108999134,-3.08546345835945,3.61742307651878));
#39873=CARTESIAN_POINT('Ctrl Pts',(213.825298570192,-4.4378887818049,1.70615873462357));
#39874=CARTESIAN_POINT('Ctrl Pts',(213.90448814125,-4.71411218006672,-0.618854442618533));
#39875=CARTESIAN_POINT('Ctrl Pts',(213.983677712307,-3.84714861417571,-2.79379347981342));
#39876=CARTESIAN_POINT('Ctrl Pts',(214.062867283365,-2.04723946343398,-4.29122885042975));
#39877=CARTESIAN_POINT('Ctrl Pts',(214.142056854422,0.249131667358439,-4.74802778843188));
#39878=CARTESIAN_POINT('Ctrl Pts',(214.22124642548,2.48508758875339,-4.05341512105853));
#39879=CARTESIAN_POINT('Ctrl Pts',(214.300435996537,4.11840198874938,-2.37583659506863));
#39880=CARTESIAN_POINT('Ctrl Pts',(214.379625567595,4.7529910112316,-0.122110255727096));
#39881=CARTESIAN_POINT('Ctrl Pts',(214.458815138652,4.23496483126893,2.16122820297104));
#39882=CARTESIAN_POINT('Ctrl Pts',(214.53800470971,2.68994641950838,3.92046205536747));
#39883=CARTESIAN_POINT('Ctrl Pts',(214.617194280768,0.492607578451629,4.72897158387045));
#39884=CARTESIAN_POINT('Ctrl Pts',(214.696383851825,-1.82419014279682,4.39069069627149));
#39885=CARTESIAN_POINT('Ctrl Pts',(214.775573422882,-3.69861604264498,2.98765356701397));
#39886=CARTESIAN_POINT('Ctrl Pts',(214.85476299394,-4.67611597131303,0.860101093031097));
#39887=CARTESIAN_POINT('Ctrl Pts',(214.933952564997,-4.51964313542201,-1.47602858909806));
#39888=CARTESIAN_POINT('Ctrl Pts',(215.013142136055,-3.2671426876119,-3.45421671673712));
#39889=CARTESIAN_POINT('Ctrl Pts',(215.092331707113,-1.22234990821534,-4.59474647497423));
#39890=CARTESIAN_POINT('Ctrl Pts',(215.17152127817,1.11886655125696,-4.62103582629268));
#39891=CARTESIAN_POINT('Ctrl Pts',(215.250710849228,3.18875436873553,-3.52670952068245));
#39892=CARTESIAN_POINT('Ctrl Pts',(215.329900420285,4.48535926739899,-1.57714511372928));
#39893=CARTESIAN_POINT('Ctrl Pts',(215.409089991343,4.69425049948609,0.754881921545774));
#39894=CARTESIAN_POINT('Ctrl Pts',(215.4882795624,3.76477128715065,2.90384772721438));
#39895=CARTESIAN_POINT('Ctrl Pts',(215.567469133458,1.92232324970198,4.34862136671582));
#39896=CARTESIAN_POINT('Ctrl Pts',(215.646658704516,-0.386294194838778,
4.73884070870039));
#39897=CARTESIAN_POINT('Ctrl Pts',(215.725848275573,-2.60123408759472,3.97987634091028));
#39898=CARTESIAN_POINT('Ctrl Pts',(215.805037846631,-4.18536656931315,2.25577949894886));
#39899=CARTESIAN_POINT('Ctrl Pts',(215.884227417688,-4.75453455305645,-0.0153509346410333));
#39900=CARTESIAN_POINT('Ctrl Pts',(215.963416988746,-4.17071302062933,-2.28275871851474));
#39901=CARTESIAN_POINT('Ctrl Pts',(216.042606559803,-2.57548052166504,-3.99659036553987));
#39902=CARTESIAN_POINT('Ctrl Pts',(216.121796130861,-0.355685932038883,
-4.74123633508727));
#39903=CARTESIAN_POINT('Ctrl Pts',(216.200985701918,1.95036360980474,-4.33611764796016));
#39904=CARTESIAN_POINT('Ctrl Pts',(216.280175272976,3.78344386943341,-2.87947685426517));
#39905=CARTESIAN_POINT('Ctrl Pts',(216.359364844033,4.69902714427905,-0.724553907401494));
#39906=CARTESIAN_POINT('Ctrl Pts',(216.438554415091,4.47508162338355,1.60607563067777));
#39907=CARTESIAN_POINT('Ctrl Pts',(216.517743986149,3.16591479676605,3.54722679948997));
#39908=CARTESIAN_POINT('Ctrl Pts',(216.596933557206,1.08900371904967,4.6281643626062));
#39909=CARTESIAN_POINT('Ctrl Pts',(216.676123128263,-1.25199417034584,4.58675757641737));
#39910=CARTESIAN_POINT('Ctrl Pts',(216.755312699321,-3.289379553279,3.43304771622419));
#39911=CARTESIAN_POINT('Ctrl Pts',(216.834502270379,-4.52908009507498,1.44681303553627));
#39912=CARTESIAN_POINT('Ctrl Pts',(216.913691841436,-4.6704645326877,-0.890278336425393));
#39913=CARTESIAN_POINT('Ctrl Pts',(216.992881412494,-3.67924669730335,-3.01147442422885));
#39914=CARTESIAN_POINT('Ctrl Pts',(217.072070983551,-1.79580001763215,-4.40237853484619));
#39915=CARTESIAN_POINT('Ctrl Pts',(217.151260554609,0.523133789193805,-4.7256920663545));
#39916=CARTESIAN_POINT('Ctrl Pts',(217.230450125666,2.71520601414163,-3.9030104750271));
#39917=CARTESIAN_POINT('Ctrl Pts',(217.309639696724,4.24883227900368,-2.13383662268189));
#39918=CARTESIAN_POINT('Ctrl Pts',(217.388829267782,4.75210341257143,0.152799291978363));
#39919=CARTESIAN_POINT('Ctrl Pts',(217.468018838839,4.10297458914856,2.40238089989979));
#39920=CARTESIAN_POINT('Ctrl Pts',(217.547208409897,2.45886158092028,4.06937761743443));
#39921=CARTESIAN_POINT('Ctrl Pts',(217.626397980954,0.218466940309538,4.74953752100075));
#39922=CARTESIAN_POINT('Ctrl Pts',(217.705587552012,-2.07490661737412,4.27791970431648));
#39923=CARTESIAN_POINT('Ctrl Pts',(217.784777123069,-3.86510882354723,2.76889296462312));
#39924=CARTESIAN_POINT('Ctrl Pts',(217.863966694127,-4.71801003786133,0.588401011251541));
#39925=CARTESIAN_POINT('Ctrl Pts',(217.943156265184,-4.42677904530272,-1.73478002970719));
#39926=CARTESIAN_POINT('Ctrl Pts',(218.022345836242,-3.06204027344824,-3.63727148164433));
#39927=CARTESIAN_POINT('Ctrl Pts',(218.101535407299,-0.95474714764384,-4.65771321052166));
#39928=CARTESIAN_POINT('Ctrl Pts',(218.180724978357,1.3840751508993,-4.54864490195323));
#39929=CARTESIAN_POINT('Ctrl Pts',(218.259914549415,3.38725489163351,-3.33651596227367));
#39930=CARTESIAN_POINT('Ctrl Pts',(218.339104120472,4.5690147152194,-1.31527145468558));
#39931=CARTESIAN_POINT('Ctrl Pts',(218.41829369153,4.6427741641966,1.02493049894648));
#39932=CARTESIAN_POINT('Ctrl Pts',(218.497483262587,3.5906463412379,3.11658359739587));
#39933=CARTESIAN_POINT('Ctrl Pts',(218.576672833645,1.66777553775722,4.45245541505591));
#39934=CARTESIAN_POINT('Ctrl Pts',(218.655862404702,-0.659536055647559,
4.70859285335895));
#39935=CARTESIAN_POINT('Ctrl Pts',(218.73505197576,-2.82690809046628,3.8228817815175));
#39936=CARTESIAN_POINT('Ctrl Pts',(218.814241546817,-4.30874606193702,2.0101099077275));
#39937=CARTESIAN_POINT('Ctrl Pts',(218.893431117875,-4.74569962215444,-0.29011991259697));
#39938=CARTESIAN_POINT('Ctrl Pts',(218.972620688933,-4.03180616460846,-2.51999474571423));
#39939=CARTESIAN_POINT('Ctrl Pts',(219.05181025999,-2.34018708804546,-4.13876296257075));
#39940=CARTESIAN_POINT('Ctrl Pts',(219.130999831048,-0.0810653152070915,
-4.75386820200902));
#39941=CARTESIAN_POINT('Ctrl Pts',(219.210189402105,2.19771505039481,-4.21614551749227));
#39942=CARTESIAN_POINT('Ctrl Pts',(219.289378973163,3.94354263494978,-2.65599434369417));
#39943=CARTESIAN_POINT('Ctrl Pts',(219.36856854422,4.73304878279435,-0.4517562252931));
#39944=CARTESIAN_POINT('Ctrl Pts',(219.447758115278,4.37477578103172,1.86203419224794));
#39945=CARTESIAN_POINT('Ctrl Pts',(219.526947686335,2.9556059543878,3.72427548790225));
#39946=CARTESIAN_POINT('Ctrl Pts',(219.606137257393,0.819692429425529,4.68336831655856));
#39947=CARTESIAN_POINT('Ctrl Pts',(219.68532682845,-1.51499907623403,4.50672966422574));
#39948=CARTESIAN_POINT('Ctrl Pts',(219.764516399508,-3.48229856225139,3.23719495717262));
#39949=CARTESIAN_POINT('Ctrl Pts',(219.843705970566,-4.60512974340184,1.18263033693475));
#39950=CARTESIAN_POINT('Ctrl Pts',(219.922895541623,-4.61120254252834,-1.15872584297627));
#39951=CARTESIAN_POINT('Ctrl Pts',(220.002085112681,-3.49904428682886,-3.21908737784704));
#39952=CARTESIAN_POINT('Ctrl Pts',(220.081274683738,-1.53835683561813,-4.49881014421679));
#39953=CARTESIAN_POINT('Ctrl Pts',(220.160464254796,0.795386965018984,-4.68755736426519));
#39954=CARTESIAN_POINT('Ctrl Pts',(220.239653825853,2.93624693618633,-3.73955724613973));
#39955=CARTESIAN_POINT('Ctrl Pts',(220.318843396911,4.36505783155326,-1.88470278679332));
#39956=CARTESIAN_POINT('Ctrl Pts',(220.398032967968,4.73532853523991,0.42719799959265));
#39957=CARTESIAN_POINT('Ctrl Pts',(220.477222539026,3.95726724216151,2.63550193347166));
#39958=CARTESIAN_POINT('Ctrl Pts',(220.556412110083,2.21955625225993,4.20468839637894));
#39959=CARTESIAN_POINT('Ctrl Pts',(220.635601681141,-0.0564040787611365,
4.75422475777419));
#39960=CARTESIAN_POINT('Ctrl Pts',(220.714791252199,-2.3186862435803,4.15084672927046));
#39961=CARTESIAN_POINT('Ctrl Pts',(220.793980823256,-4.01867973527754,2.54087537220366));
#39962=CARTESIAN_POINT('Ctrl Pts',(220.873170394314,-4.7441308059444,0.314733781326927));
#39963=CARTESIAN_POINT('Ctrl Pts',(220.952359965371,-4.31911530641839,-1.98773173647174));
#39964=CARTESIAN_POINT('Ctrl Pts',(221.031549536429,-2.8467008113479,-3.8081660854415));
#39965=CARTESIAN_POINT('Ctrl Pts',(221.110739107486,-0.683952477452091,
-4.70510823248726));
#39966=CARTESIAN_POINT('Ctrl Pts',(221.189928678544,1.64465651901248,-4.46104690585135));
#39967=CARTESIAN_POINT('Ctrl Pts',(221.269118249601,3.57443106392721,-3.13516772584365));
#39968=CARTESIAN_POINT('Ctrl Pts',(221.348307820659,4.63739508778881,-1.04900057820502));
#39969=CARTESIAN_POINT('Ctrl Pts',(221.427497391716,4.57577584957209,1.29155254196728));
#39970=CARTESIAN_POINT('Ctrl Pts',(221.506686962774,3.40451755984005,3.31890002529642));
#39971=CARTESIAN_POINT('Ctrl Pts',(221.585876533832,1.40765114992216,4.54140407594682));
#39972=CARTESIAN_POINT('Ctrl Pts',(221.665066104889,-0.930570927433501,
4.66260296168317));
#39973=CARTESIAN_POINT('Ctrl Pts',(221.744255675947,-3.0431354414086,3.65310700279724));
#39974=CARTESIAN_POINT('Ctrl Pts',(221.823445247004,-4.41771141175782,1.75771911177364));
#39975=CARTESIAN_POINT('Ctrl Pts',(221.902634818062,-4.72101826342946,-0.563916692847134));
#39976=CARTESIAN_POINT('Ctrl Pts',(221.98182438912,-3.87937964092229,-2.74880956730796));
#39977=CARTESIAN_POINT('Ctrl Pts',(222.061013960177,-2.09716129213571,-4.26708329290772));
#39978=CARTESIAN_POINT('Ctrl Pts',(222.140203531235,0.193988579230145,-4.75059111312483));
#39979=CARTESIAN_POINT('Ctrl Pts',(222.192996578606,1.68938130567583,-4.30468574388314));
#39980=CARTESIAN_POINT('Ctrl Pts',(222.219393102292,2.33899160943743,-3.91675404524988));
#39981=CARTESIAN_POINT('Ctrl Pts',(209.342,2.5383587572263,-3.55965150255085));
#39982=CARTESIAN_POINT('Ctrl Pts',(209.368396523686,3.12874208667276,-3.13865391518958));
#39983=CARTESIAN_POINT('Ctrl Pts',(209.421189571058,4.09533550545485,-1.99754846162188));
#39984=CARTESIAN_POINT('Ctrl Pts',(209.500379142115,4.55219349719505,0.199542953564506));
#39985=CARTESIAN_POINT('Ctrl Pts',(209.579568713173,3.90500385774559,2.34791981561545));
#39986=CARTESIAN_POINT('Ctrl Pts',(209.65875828423,2.31088729255791,3.92708782806959));
#39987=CARTESIAN_POINT('Ctrl Pts',(209.737947855288,0.156348682839113,4.55384789993644));
#39988=CARTESIAN_POINT('Ctrl Pts',(209.817137426345,-2.03609361756371,4.07632219349179));
#39989=CARTESIAN_POINT('Ctrl Pts',(209.896326997403,-3.73478222633324,2.61025841618883));
#39990=CARTESIAN_POINT('Ctrl Pts',(209.97551656846,-4.52777192009244,0.511206898731814));
#39991=CARTESIAN_POINT('Ctrl Pts',(210.054706139518,-4.22276393917902,-1.71181770547838));
#39992=CARTESIAN_POINT('Ctrl Pts',(210.133895710575,-2.89372191923785,-3.5197193599864));
#39993=CARTESIAN_POINT('Ctrl Pts',(210.213085281633,-0.862943537879242,
-4.47407889498736));
#39994=CARTESIAN_POINT('Ctrl Pts',(210.29227485269,1.37710147802978,-4.3434598905811));
#39995=CARTESIAN_POINT('Ctrl Pts',(210.371464423748,3.2831950149358,-3.15953845045613));
#39996=CARTESIAN_POINT('Ctrl Pts',(210.450653994806,4.39310350826522,-1.20941895478298));
#39997=CARTESIAN_POINT('Ctrl Pts',(210.529843565863,4.43767063245068,1.03398838263629));
#39998=CARTESIAN_POINT('Ctrl Pts',(210.609033136921,3.40608873948736,3.02665031932622));
#39999=CARTESIAN_POINT('Ctrl Pts',(210.688222707978,1.54851965941115,4.28534006751519));
#40000=CARTESIAN_POINT('Ctrl Pts',(210.767412279036,-0.68457028532424,4.50482143573546));
#40001=CARTESIAN_POINT('Ctrl Pts',(210.846601850094,-2.75164979303246,3.63186949857032));
#40002=CARTESIAN_POINT('Ctrl Pts',(210.925791421151,-4.15144560986192,1.87817783712018));
#40003=CARTESIAN_POINT('Ctrl Pts',(211.004980992209,-4.5445028677362,-0.330977831100565));
#40004=CARTESIAN_POINT('Ctrl Pts',(211.084170563266,-3.83550395069923,-2.45987033873152));
#40005=CARTESIAN_POINT('Ctrl Pts',(211.163360134324,-2.19638331619705,-3.99223658715306));
#40006=CARTESIAN_POINT('Ctrl Pts',(211.242549705381,-0.0246328503458637,
-4.55647296294042));
#40007=CARTESIAN_POINT('Ctrl Pts',(211.321739276439,2.1530911588358,-4.01575037833895));
#40008=CARTESIAN_POINT('Ctrl Pts',(211.400928847496,3.80868382039997,-2.501195753153));
#40009=CARTESIAN_POINT('Ctrl Pts',(211.480118418554,4.54065873004066,-0.380093326269416));
#40010=CARTESIAN_POINT('Ctrl Pts',(211.559307989612,4.17150968026545,1.83318292235754));
#40011=CARTESIAN_POINT('Ctrl Pts',(211.638497560669,2.79075647149654,3.60190657238208));
#40012=CARTESIAN_POINT('Ctrl Pts',(211.717687131727,0.733236080175323,4.4971566005755));
#40013=CARTESIAN_POINT('Ctrl Pts',(211.796876702784,-1.50209635644419,4.30183207195806));
#40014=CARTESIAN_POINT('Ctrl Pts',(211.876066273842,-3.37316572337063,3.06329979630588));
#40015=CARTESIAN_POINT('Ctrl Pts',(211.955255844899,-4.42623184056749,1.081907728467));
#40016=CARTESIAN_POINT('Ctrl Pts',(212.034445415957,-4.40592287733015,-1.16185035111622));
#40017=CARTESIAN_POINT('Ctrl Pts',(212.113634987014,-3.31716382083363,-3.1238560826521));
#40018=CARTESIAN_POINT('Ctrl Pts',(212.192824558072,-1.42398215132184,-4.32831693295292));
#40019=CARTESIAN_POINT('Ctrl Pts',(212.272014129129,0.814519648555283,-4.48314737450014));
#40020=CARTESIAN_POINT('Ctrl Pts',(212.351203700187,2.85549788329282,-3.5508005404247));
#40021=CARTESIAN_POINT('Ctrl Pts',(212.430393271244,4.20400894040367,-1.75737345728678));
#40022=CARTESIAN_POINT('Ctrl Pts',(212.509582842302,4.53303466617831,0.462222191803663));
#40023=CARTESIAN_POINT('Ctrl Pts',(212.588772413359,3.76278529189487,2.56972751210507));
#40024=CARTESIAN_POINT('Ctrl Pts',(212.667961984417,2.08004870256613,4.05406586457634));
#40025=CARTESIAN_POINT('Ctrl Pts',(212.747151555475,-0.107106210032759,
4.55528055109042));
#40026=CARTESIAN_POINT('Ctrl Pts',(212.826341126532,-2.2682875313355,3.95182544080049));
#40027=CARTESIAN_POINT('Ctrl Pts',(212.90553069759,-3.87940202399173,2.39004028744685));
#40028=CARTESIAN_POINT('Ctrl Pts',(212.984720268647,-4.5497493789273,0.248662880866296));
#40029=CARTESIAN_POINT('Ctrl Pts',(213.063909839705,-4.11676826362727,-1.95301605291953));
#40030=CARTESIAN_POINT('Ctrl Pts',(213.143099410762,-2.685457954271,-3.68108247872997));
#40031=CARTESIAN_POINT('Ctrl Pts',(213.22228898182,-0.602915682492534,-4.51647487750953));
#40032=CARTESIAN_POINT('Ctrl Pts',(213.301478552877,1.62583553009629,-4.25660797683398));
#40033=CARTESIAN_POINT('Ctrl Pts',(213.380668123935,3.46031653593829,-2.96450031379357));
#40034=CARTESIAN_POINT('Ctrl Pts',(213.459857694992,4.45565994712272,-0.953492042429545));
#40035=CARTESIAN_POINT('Ctrl Pts',(213.53904726605,4.37049186989017,1.28874103472886));
#40036=CARTESIAN_POINT('Ctrl Pts',(213.618236837108,3.22546582964164,3.21845037575295));
#40037=CARTESIAN_POINT('Ctrl Pts',(213.697426408165,1.29825422636,4.36767542327822));
#40038=CARTESIAN_POINT('Ctrl Pts',(213.776615979223,-0.943788091813559,
4.45772550490954));
#40039=CARTESIAN_POINT('Ctrl Pts',(213.85580555028,-2.9569588426014,3.46676319389305));
#40040=CARTESIAN_POINT('Ctrl Pts',(213.934995121338,-4.25305781544302,1.63509995347965));
#40041=CARTESIAN_POINT('Ctrl Pts',(214.014184692395,-4.51777695117311,-0.593080145359114));
#40042=CARTESIAN_POINT('Ctrl Pts',(214.093374263453,-3.68692103050771,-2.6774364519387));
#40043=CARTESIAN_POINT('Ctrl Pts',(214.172563834511,-1.96197521572409,-4.11250603552804));
#40044=CARTESIAN_POINT('Ctrl Pts',(214.251753405568,0.238755732067328,-4.55028002872078));
#40045=CARTESIAN_POINT('Ctrl Pts',(214.330942976626,2.38158766725776,-3.88459686744144));
#40046=CARTESIAN_POINT('Ctrl Pts',(214.410132547683,3.94687713608336,-2.27688680263919));
#40047=CARTESIAN_POINT('Ctrl Pts',(214.489322118741,4.55503654123292,-0.117024558973872));
#40048=CARTESIAN_POINT('Ctrl Pts',(214.568511689798,4.05858532273295,2.07121650666143));
#40049=CARTESIAN_POINT('Ctrl Pts',(214.647701260856,2.57791445552183,3.75718108418821));
#40050=CARTESIAN_POINT('Ctrl Pts',(214.726890831913,0.472091261067617,4.53201748458606));
#40051=CARTESIAN_POINT('Ctrl Pts',(214.806080402971,-1.74821554237347,4.20782545464685));
#40052=CARTESIAN_POINT('Ctrl Pts',(214.885269974028,-3.54457460290309,2.86322257671746));
#40053=CARTESIAN_POINT('Ctrl Pts',(214.964459545086,-4.48136322371341,0.824279258818916));
#40054=CARTESIAN_POINT('Ctrl Pts',(215.043649116144,-4.33140723105327,-1.41455436026672));
#40055=CARTESIAN_POINT('Ctrl Pts',(215.122838687201,-3.13107142267409,-3.31035411783751));
#40056=CARTESIAN_POINT('Ctrl Pts',(215.202028258259,-1.17144099051237,-4.40338263669165));
#40057=CARTESIAN_POINT('Ctrl Pts',(215.281217829316,1.07226754977981,-4.42857707859527));
#40058=CARTESIAN_POINT('Ctrl Pts',(215.360407400374,3.05594785184388,-3.37982771249969));
#40059=CARTESIAN_POINT('Ctrl Pts',(215.439596971431,4.29855123127321,-1.5114595434512));
#40060=CARTESIAN_POINT('Ctrl Pts',(215.518786542489,4.49874247780649,0.723442297456857));
#40061=CARTESIAN_POINT('Ctrl Pts',(215.597976113546,3.60797458733507,2.7829071160415));
#40062=CARTESIAN_POINT('Ctrl Pts',(215.677165684604,1.84226156240618,4.16750824534888));
#40063=CARTESIAN_POINT('Ctrl Pts',(215.756355255662,-0.370205659762209,
4.54147557615916));
#40064=CARTESIAN_POINT('Ctrl Pts',(215.835544826719,-2.49289685027711,3.81412085981142));
#40065=CARTESIAN_POINT('Ctrl Pts',(215.914734397777,-4.01105274902173,2.16182989246041));
#40066=CARTESIAN_POINT('Ctrl Pts',(215.993923968834,-4.5565157970107,-0.0147115927774353));
#40067=CARTESIAN_POINT('Ctrl Pts',(216.073113539892,-3.99700949719232,-2.18768547070287));
#40068=CARTESIAN_POINT('Ctrl Pts',(216.152303110949,-2.46821587915816,-3.83013877206057));
#40069=CARTESIAN_POINT('Ctrl Pts',(216.231492682007,-0.340872182129313,
-4.54377142854046));
#40070=CARTESIAN_POINT('Ctrl Pts',(216.310682253064,1.86913408638018,-4.15552528647124));
#40071=CARTESIAN_POINT('Ctrl Pts',(216.389871824122,3.62586948644518,-2.75955125095293));
#40072=CARTESIAN_POINT('Ctrl Pts',(216.469061395179,4.50332018298729,-0.694377396571518));
#40073=CARTESIAN_POINT('Ctrl Pts',(216.548250966237,4.28870163468497,1.5391851506627));
#40074=CARTESIAN_POINT('Ctrl Pts',(216.627440537294,3.03405951149959,3.39949047947615));
#40075=CARTESIAN_POINT('Ctrl Pts',(216.706630108352,1.04364845674816,4.43540872277824));
#40076=CARTESIAN_POINT('Ctrl Pts',(216.78581967941,-1.19985061656117,4.39572646297605));
#40077=CARTESIAN_POINT('Ctrl Pts',(216.865009250467,-3.15238215846906,3.29006677232181));
#40078=CARTESIAN_POINT('Ctrl Pts',(216.944198821525,-4.3404511564375,1.38655558776074));
#40079=CARTESIAN_POINT('Ctrl Pts',(217.023388392582,-4.47594715846353,-0.853199668314748));
#40080=CARTESIAN_POINT('Ctrl Pts',(217.10257796364,-3.52601195980057,-2.8860513333469));
#40081=CARTESIAN_POINT('Ctrl Pts',(217.181767534697,-1.72100782049271,-4.21902651344751));
#40082=CARTESIAN_POINT('Ctrl Pts',(217.260957105755,0.501346103979698,-4.52887455372684));
#40083=CARTESIAN_POINT('Ctrl Pts',(217.340146676813,2.60212202845841,-3.74045633424341));
#40084=CARTESIAN_POINT('Ctrl Pts',(217.41933624787,4.07187521345992,-2.04496574185997));
#40085=CARTESIAN_POINT('Ctrl Pts',(217.498525818928,4.55418590963663,0.146435445973139));
#40086=CARTESIAN_POINT('Ctrl Pts',(217.577715389985,3.93209226298936,2.3023255796497));
#40087=CARTESIAN_POINT('Ctrl Pts',(217.656904961043,2.35645393068466,3.89989455138609));
#40088=CARTESIAN_POINT('Ctrl Pts',(217.7360945321,0.209368141831046,4.55172688334399));
#40089=CARTESIAN_POINT('Ctrl Pts',(217.815284103158,-1.98849007697495,4.0997511940534));
#40090=CARTESIAN_POINT('Ctrl Pts',(217.894473674215,-3.70413322589841,2.65357300336085));
#40091=CARTESIAN_POINT('Ctrl Pts',(217.973663245273,-4.52151246942783,0.563895050677703));
#40092=CARTESIAN_POINT('Ctrl Pts',(218.05285281633,-4.24241078168862,-1.66252921742216));
#40093=CARTESIAN_POINT('Ctrl Pts',(218.132042387388,-2.93451119586052,-3.48578494470606));
#40094=CARTESIAN_POINT('Ctrl Pts',(218.211231958445,-0.914983456707324,
-4.46372690846136));
#40095=CARTESIAN_POINT('Ctrl Pts',(218.290421529503,1.32643063562732,-4.35920112041638));
#40096=CARTESIAN_POINT('Ctrl Pts',(218.369611100561,3.24618114559881,-3.1975554114556));
#40097=CARTESIAN_POINT('Ctrl Pts',(218.448800671618,4.37872256355528,-1.26049250326289));
#40098=CARTESIAN_POINT('Ctrl Pts',(218.527990242676,4.44941004951064,0.982243783733906));
#40099=CARTESIAN_POINT('Ctrl Pts',(218.607179813733,3.44110166678914,2.98678287764463));
#40100=CARTESIAN_POINT('Ctrl Pts',(218.686369384791,1.59831535534295,4.26701777172829));
#40101=CARTESIAN_POINT('Ctrl Pts',(218.765558955848,-0.632067434303197,
4.51248749559082));
#40102=CARTESIAN_POINT('Ctrl Pts',(218.844748526906,-2.70917189204705,3.66366487259853));
#40103=CARTESIAN_POINT('Ctrl Pts',(218.923938097963,-4.12929368320664,1.92639204659899));
#40104=CARTESIAN_POINT('Ctrl Pts',(219.003127669021,-4.54804882684332,-0.278036882480057));
#40105=CARTESIAN_POINT('Ctrl Pts',(219.082317240079,-3.8638878894494,-2.41504099698875));
#40106=CARTESIAN_POINT('Ctrl Pts',(219.161506811136,-2.24272204053807,-3.96639010792621));
#40107=CARTESIAN_POINT('Ctrl Pts',(219.240696382194,-0.077689074547423,
-4.55587719841812));
#40108=CARTESIAN_POINT('Ctrl Pts',(219.319885953251,2.10618373527536,-4.04054980326089));
#40109=CARTESIAN_POINT('Ctrl Pts',(219.399075524309,3.77930039456389,-2.54537642933601));
#40110=CARTESIAN_POINT('Ctrl Pts',(219.478265095366,4.53592487469901,-0.43294130139881));
#40111=CARTESIAN_POINT('Ctrl Pts',(219.557454666424,4.19257337016016,1.78448344772206));
#40112=CARTESIAN_POINT('Ctrl Pts',(219.636644237481,2.83250969587536,3.569165373325));
#40113=CARTESIAN_POINT('Ctrl Pts',(219.715833808539,0.785553551391572,4.48831352038449));
#40114=CARTESIAN_POINT('Ctrl Pts',(219.795023379596,-1.45190178897309,4.3190315852685));
#40115=CARTESIAN_POINT('Ctrl Pts',(219.874212950654,-3.33726639942199,3.10237096728598));
#40116=CARTESIAN_POINT('Ctrl Pts',(219.953402521712,-4.41333345860431,1.13337567581733));
#40117=CARTESIAN_POINT('Ctrl Pts',(220.032592092769,-4.41915333536473,-1.11046676578087));
#40118=CARTESIAN_POINT('Ctrl Pts',(220.111781663827,-3.35331469136689,-3.08501753966403));
#40119=CARTESIAN_POINT('Ctrl Pts',(220.190971234884,-1.47428673505533,-4.31144190059531));
#40120=CARTESIAN_POINT('Ctrl Pts',(220.270160805942,0.762260370684581,-4.49232810095734));
#40121=CARTESIAN_POINT('Ctrl Pts',(220.349350376999,2.81395694980418,-3.58381067078537));
#40122=CARTESIAN_POINT('Ctrl Pts',(220.428539948057,4.18326015772707,-1.80620793157832));
#40123=CARTESIAN_POINT('Ctrl Pts',(220.507729519115,4.53810967910322,0.409405886501342));
#40124=CARTESIAN_POINT('Ctrl Pts',(220.586919090172,3.79245339384702,2.52573749520784));
#40125=CARTESIAN_POINT('Ctrl Pts',(220.66610866123,2.12711528603252,4.02956985290854));
#40126=CARTESIAN_POINT('Ctrl Pts',(220.745298232287,-0.0540549391371643,
4.55621890420622));
#40127=CARTESIAN_POINT('Ctrl Pts',(220.824487803345,-2.22211667183979,3.97797060507901));
#40128=CARTESIAN_POINT('Ctrl Pts',(220.903677374402,-3.85130815489554,2.43505197879753));
#40129=CARTESIAN_POINT('Ctrl Pts',(220.98286694546,-4.54654534931804,0.30162562296389));
#40130=CARTESIAN_POINT('Ctrl Pts',(221.062056516517,-4.13923106524796,-1.90494589036706));
#40131=CARTESIAN_POINT('Ctrl Pts',(221.141246087575,-2.72814027777575,-3.64956206171641));
#40132=CARTESIAN_POINT('Ctrl Pts',(221.220435658632,-0.655466951210102,
-4.50914800360244));
#40133=CARTESIAN_POINT('Ctrl Pts',(221.29962522969,1.57615920673447,-4.27525144067998));
#40134=CARTESIAN_POINT('Ctrl Pts',(221.378814800747,3.42556172983117,-3.00459300688041));
#40135=CARTESIAN_POINT('Ctrl Pts',(221.458004371805,4.44425500302777,-1.00531138270765));
#40136=CARTESIAN_POINT('Ctrl Pts',(221.537193942863,4.38520210748118,1.23776144530491));
#40137=CARTESIAN_POINT('Ctrl Pts',(221.61638351392,3.26272485129782,3.18067315006488));
#40138=CARTESIAN_POINT('Ctrl Pts',(221.695573084978,1.34902473201658,4.35226186322655));
#40139=CARTESIAN_POINT('Ctrl Pts',(221.774762656035,-0.891814137382579,
4.46841300931145));
#40140=CARTESIAN_POINT('Ctrl Pts',(221.853952227093,-2.91639371982429,3.50096094174254));
#40141=CARTESIAN_POINT('Ctrl Pts',(221.93314179815,-4.23372080057107,1.68451292342707));
#40142=CARTESIAN_POINT('Ctrl Pts',(222.012331369208,-4.52439540721473,-0.540430464955662));
#40143=CARTESIAN_POINT('Ctrl Pts',(222.091520940266,-3.71780968656559,-2.63432604740694));
#40144=CARTESIAN_POINT('Ctrl Pts',(222.170710511323,-2.00981788014407,-4.08936610183967));
#40145=CARTESIAN_POINT('Ctrl Pts',(222.249900082381,0.185909265320968,-4.55273659504203));
#40146=CARTESIAN_POINT('Ctrl Pts',(222.302693129752,1.61902127760079,-4.12540247090247));
#40147=CARTESIAN_POINT('Ctrl Pts',(222.329089653438,2.24157635170112,-3.75362750675853));
#40148=CARTESIAN_POINT('',(222.,2.53382212490982,-4.24300712223271));
#40149=CARTESIAN_POINT('Ctrl Pts',(222.,-4.36842834878726,-0.181075889670495));
#40150=CARTESIAN_POINT('Ctrl Pts',(222.,-4.37098573801141,-0.294564226943176));
#40151=CARTESIAN_POINT('Ctrl Pts',(222.,-4.36909332532532,-0.408000110792678));
#40152=CARTESIAN_POINT('Ctrl Pts',(222.,-4.36272833344689,-0.521122630740717));
#40153=CARTESIAN_POINT('Ctrl Pts',(222.,-4.35524756813103,-0.654075357127793));
#40154=CARTESIAN_POINT('Ctrl Pts',(222.,-4.3415902166335,-0.786595637407321));
#40155=CARTESIAN_POINT('Ctrl Pts',(222.,-4.32194320104597,-0.918301328088664));
#40156=CARTESIAN_POINT('Ctrl Pts',(222.,-4.31073473472777,-0.993438378361748));
#40157=CARTESIAN_POINT('Ctrl Pts',(222.,-4.29757589374814,-1.06831043566032));
#40158=CARTESIAN_POINT('Ctrl Pts',(222.,-4.28249385860505,-1.14284660544086));
#40159=CARTESIAN_POINT('Ctrl Pts',(222.,-4.27226836316086,-1.19338151384594));
#40160=CARTESIAN_POINT('Ctrl Pts',(222.,-4.2611587153347,-1.24376202130847));
#40161=CARTESIAN_POINT('Ctrl Pts',(222.,-4.24917200170829,-1.29396584478053));
#40162=CARTESIAN_POINT('Ctrl Pts',(222.,-4.24463496174222,-1.31296828036392));
#40163=CARTESIAN_POINT('Ctrl Pts',(222.,-4.23997254218613,-1.3319440220672));
#40164=CARTESIAN_POINT('Ctrl Pts',(222.,-4.23518762442552,-1.35088254754639));
#40165=CARTESIAN_POINT('Ctrl Pts',(222.,-4.20189893344145,-1.48263794103715));
#40166=CARTESIAN_POINT('Ctrl Pts',(222.,-4.16265630755129,-1.61271654924556));
#40167=CARTESIAN_POINT('Ctrl Pts',(222.,-4.11765567171295,-1.74072293688837));
#40168=CARTESIAN_POINT('Ctrl Pts',(222.,-4.07248857953235,-1.8692028172869));
#40169=CARTESIAN_POINT('Ctrl Pts',(222.,-4.02152063408476,-1.99559591273624));
#40170=CARTESIAN_POINT('Ctrl Pts',(222.,-3.96489773029065,-2.11949676875068));
#40171=CARTESIAN_POINT('Ctrl Pts',(222.,-3.94205531338401,-2.16947998788162));
#40172=CARTESIAN_POINT('Ctrl Pts',(222.,-3.91829201952593,-2.21905748457378));
#40173=CARTESIAN_POINT('Ctrl Pts',(222.,-3.89361512847883,-2.26820192736284));
#40174=CARTESIAN_POINT('Ctrl Pts',(222.,-3.88019709114222,-2.29492417397697));
#40175=CARTESIAN_POINT('Ctrl Pts',(222.,-3.86650891432765,-2.32151837366928));
#40176=CARTESIAN_POINT('Ctrl Pts',(222.,-3.85255160932784,-2.34798006053391));
#40177=CARTESIAN_POINT('Ctrl Pts',(222.,-3.83952664999993,-2.37267411108051));
#40178=CARTESIAN_POINT('Ctrl Pts',(222.,-3.82626470140156,-2.39725729977753));
#40179=CARTESIAN_POINT('Ctrl Pts',(222.,-3.81278183000108,-2.42169876135494));
#40180=CARTESIAN_POINT('Ctrl Pts',(222.,-3.77582885392445,-2.4886863278844));
#40181=CARTESIAN_POINT('Ctrl Pts',(222.,-3.73719936713687,-2.55464384426184));
#40182=CARTESIAN_POINT('Ctrl Pts',(222.,-3.69692762264733,-2.61950430450256));
#40183=CARTESIAN_POINT('Ctrl Pts',(222.,-3.62547763214162,-2.73457950988876));
#40184=CARTESIAN_POINT('Ctrl Pts',(222.,-3.54886116571452,-2.84620257618153));
#40185=CARTESIAN_POINT('Ctrl Pts',(222.,-3.46744919683223,-2.95414631713669));
#40186=CARTESIAN_POINT('Ctrl Pts',(222.,-3.3848883088047,-3.06361340450265));
#40187=CARTESIAN_POINT('Ctrl Pts',(222.,-3.29739521161876,-3.1692971916575));
#40188=CARTESIAN_POINT('Ctrl Pts',(222.,-3.2053076828989,-3.27093946602781));
#40189=CARTESIAN_POINT('Ctrl Pts',(222.,-3.12292504328557,-3.36186989901187));
#40190=CARTESIAN_POINT('Ctrl Pts',(222.,-3.03686442460084,-3.449565783402));
#40191=CARTESIAN_POINT('Ctrl Pts',(222.,-2.94733923617142,-3.53382207273257));
#40192=CARTESIAN_POINT('Ctrl Pts',(222.,-2.88019534484935,-3.5970142897305));
#40193=CARTESIAN_POINT('Ctrl Pts',(222.,-2.81110205788549,-3.65827137366228));
#40194=CARTESIAN_POINT('Ctrl Pts',(222.,-2.74014107955737,-3.71749798768638));
#40195=CARTESIAN_POINT('Ctrl Pts',(222.,-2.71949941549928,-3.73472627143876));
#40196=CARTESIAN_POINT('Ctrl Pts',(222.,-2.69869477510875,-3.75178651986409));
#40197=CARTESIAN_POINT('Ctrl Pts',(222.,-2.67775618886315,-3.76865475809313));
#40198=CARTESIAN_POINT('Ctrl Pts',(222.,-2.56828725956211,-3.85684351909489));
#40199=CARTESIAN_POINT('Ctrl Pts',(222.,-2.45505249945321,-3.93988052555356));
#40200=CARTESIAN_POINT('Ctrl Pts',(222.,-2.33842175663197,-4.01751530374901));
#40201=CARTESIAN_POINT('Ctrl Pts',(222.,-2.24728794844213,-4.0781781514149));
#40202=CARTESIAN_POINT('Ctrl Pts',(222.,-2.15407959825342,-4.13554221388341));
#40203=CARTESIAN_POINT('Ctrl Pts',(222.,-2.05895545541908,-4.1894747272104));
#40204=CARTESIAN_POINT('Ctrl Pts',(222.,-1.93779588756135,-4.25816853945908));
#40205=CARTESIAN_POINT('Ctrl Pts',(222.,-1.81352904188079,-4.32129707181206));
#40206=CARTESIAN_POINT('Ctrl Pts',(222.,-1.68657664425576,-4.37879834388636));
#40207=CARTESIAN_POINT('Ctrl Pts',(222.,-1.55887908425306,-4.43663712659787));
#40208=CARTESIAN_POINT('Ctrl Pts',(222.,-1.42846364438894,-4.48878270602783));
#40209=CARTESIAN_POINT('Ctrl Pts',(222.,-1.29573422995731,-4.53512593072363));
#40210=CARTESIAN_POINT('Ctrl Pts',(222.,-1.24442289374099,-4.55304157356661));
#40211=CARTESIAN_POINT('Ctrl Pts',(222.,-1.19276552717026,-4.57008955079262));
#40212=CARTESIAN_POINT('Ctrl Pts',(222.,-1.14078481387357,-4.58626157075573));
#40213=CARTESIAN_POINT('Ctrl Pts',(222.,-1.11945747958225,-4.59289684091739));
#40214=CARTESIAN_POINT('Ctrl Pts',(222.,-1.09807373972044,-4.59938514101186));
#40215=CARTESIAN_POINT('Ctrl Pts',(222.,-1.07665683628407,-4.60571966869325));
#40216=CARTESIAN_POINT('Ctrl Pts',(222.,-0.94036242090938,-4.64603178708956));
#40217=CARTESIAN_POINT('Ctrl Pts',(222.,-0.802537508945014,-4.68018040969709));
#40218=CARTESIAN_POINT('Ctrl Pts',(222.,-0.663631693948421,-4.70813488340432));
#40219=CARTESIAN_POINT('Ctrl Pts',(222.,-0.522032220811885,-4.73663144957651));
#40220=CARTESIAN_POINT('Ctrl Pts',(222.,-0.379308809281521,-4.75869170631474));
#40221=CARTESIAN_POINT('Ctrl Pts',(222.,-0.2359104528045,-4.7742353901663));
#40222=CARTESIAN_POINT('Ctrl Pts',(222.,-0.0925120963274796,-4.78977907401787));
#40223=CARTESIAN_POINT('Ctrl Pts',(222.,0.0515620228970814,-4.79880645835128));
#40224=CARTESIAN_POINT('Ctrl Pts',(222.,0.195878260323218,-4.80118506931799));
#40225=CARTESIAN_POINT('Ctrl Pts',(222.,0.29689613471544,-4.80285003944297));
#40226=CARTESIAN_POINT('Ctrl Pts',(222.,0.398032971152377,-4.80125620971581));
#40227=CARTESIAN_POINT('Ctrl Pts',(222.,0.499147154433433,-4.79644184461924));
#40228=CARTESIAN_POINT('Ctrl Pts',(222.,0.543384609618895,-4.79433555988949));
#40229=CARTESIAN_POINT('Ctrl Pts',(222.,0.587617726136605,-4.79161267339));
#40230=CARTESIAN_POINT('Ctrl Pts',(222.,0.631834586924468,-4.78827559687945));
#40231=CARTESIAN_POINT('Ctrl Pts',(222.,0.65953222059132,-4.78618523765763));
#40232=CARTESIAN_POINT('Ctrl Pts',(222.,0.687223474722988,-4.78385387155131));
#40233=CARTESIAN_POINT('Ctrl Pts',(222.,0.714905404701823,-4.78128199606419));
#40234=CARTESIAN_POINT('Ctrl Pts',(222.,0.733390830872528,-4.77956455026205));
#40235=CARTESIAN_POINT('Ctrl Pts',(222.,0.751867033752694,-4.77774029318992));
#40236=CARTESIAN_POINT('Ctrl Pts',(222.,0.770325374548045,-4.77581043336942));
#40237=CARTESIAN_POINT('Ctrl Pts',(222.,0.912376353166609,-4.76095869348995));
#40238=CARTESIAN_POINT('Ctrl Pts',(222.,1.05350857384173,-4.7398439933652));
#40239=CARTESIAN_POINT('Ctrl Pts',(222.,1.19332576755747,-4.71266318948087));
#40240=CARTESIAN_POINT('Ctrl Pts',(222.,1.33571979507934,-4.68498144281214));
#40241=CARTESIAN_POINT('Ctrl Pts',(222.,1.47675060798872,-4.65100794853853));
#40242=CARTESIAN_POINT('Ctrl Pts',(222.,1.61600588548905,-4.61089731421076));
#40243=CARTESIAN_POINT('Ctrl Pts',(222.,1.755439378739,-4.5707353472018));
#40244=CARTESIAN_POINT('Ctrl Pts',(222.,1.89309357002474,-4.52442039296622));
#40245=CARTESIAN_POINT('Ctrl Pts',(222.,2.02854931760949,-4.47205576788645));
#40246=CARTESIAN_POINT('Ctrl Pts',(222.,2.16242889981937,-4.4203004584717));
#40247=CARTESIAN_POINT('Ctrl Pts',(222.,2.29416163637294,-4.36263522966432));
#40248=CARTESIAN_POINT('Ctrl Pts',(222.,2.42332650648257,-4.29911192429263));
#40249=CARTESIAN_POINT('Ctrl Pts',(222.,2.46037320343389,-4.28089235234978));
#40250=CARTESIAN_POINT('Ctrl Pts',(222.,2.49720851529581,-4.26219057786635));
#40251=CARTESIAN_POINT('Ctrl Pts',(222.,2.53382212491006,-4.24300712223256));
#40252=CARTESIAN_POINT('Ctrl Pts',(222.,2.53382212490976,-4.24300712223274));
#40253=CARTESIAN_POINT('Ctrl Pts',(221.973603476314,1.83010136182567,-4.66325228984456));
#40254=CARTESIAN_POINT('Ctrl Pts',(221.947206952628,1.02012428443705,-4.90477621956747));
#40255=CARTESIAN_POINT('Ctrl Pts',(221.920810428943,0.201469858548206,-4.93824110538784));
#40256=CARTESIAN_POINT('Ctrl Pts',(221.894413905257,-0.617184567340706,
-4.97170599120821));
#40257=CARTESIAN_POINT('Ctrl Pts',(221.868017381571,-1.44451634172984,-4.79711183312601));
#40258=CARTESIAN_POINT('Ctrl Pts',(221.841620857885,-2.17996080117718,-4.43569124276262));
#40259=CARTESIAN_POINT('Ctrl Pts',(221.815224334199,-2.91540526062457,-4.07427065239921));
#40260=CARTESIAN_POINT('Ctrl Pts',(221.788827810513,-3.55896240513016,-3.52602362975458));
#40261=CARTESIAN_POINT('Ctrl Pts',(221.762431286827,-4.03269838175349,-2.85741887535226));
#40262=CARTESIAN_POINT('Ctrl Pts',(221.736034763142,-4.50643435837679,-2.18881412094998));
#40263=CARTESIAN_POINT('Ctrl Pts',(221.709638239456,-4.81034916711786,-1.39985163479002));
#40264=CARTESIAN_POINT('Ctrl Pts',(221.68324171577,-4.90754468120046,-0.586200285527234));
#40265=CARTESIAN_POINT('Ctrl Pts',(221.676934628732,-4.9307682152643,-0.391789463134336));
#40266=CARTESIAN_POINT('Ctrl Pts',(221.670627541695,-4.94219003245996,-0.195969140130387));
#40267=CARTESIAN_POINT('Ctrl Pts',(221.664320454657,-4.94199158848527,-0.000125892924181525));
#40268=CARTESIAN_POINT('Origin',(228.,-0.6,-7.5));
#40269=CARTESIAN_POINT('',(226.2,-0.6,7.5));
#40270=CARTESIAN_POINT('Origin',(226.2,0.,0.));
#40271=CARTESIAN_POINT('',(226.2,0.6,-7.5));
#40272=CARTESIAN_POINT('',(226.2,4.163799117101E-16,6.8));
#40273=CARTESIAN_POINT('',(226.2,-1.7,5.1));
#40274=CARTESIAN_POINT('',(226.2,1.575,5.225));
#40275=CARTESIAN_POINT('',(226.2,-1.2491397351303E-15,-6.8));
#40276=CARTESIAN_POINT('',(226.2,1.7,-5.1));
#40277=CARTESIAN_POINT('',(226.2,-1.575,-5.225));
#40278=CARTESIAN_POINT('Origin',(228.,0.6,7.5));
#40279=CARTESIAN_POINT('Origin',(222.5,-1.2491397351303E-15,-6.8));
#40280=CARTESIAN_POINT('',(222.5,-1.2491397351303E-15,-6.8));
#40281=CARTESIAN_POINT('',(222.5,-1.2491397351303E-15,-6.8));
#40282=CARTESIAN_POINT('',(222.5,-1.2491397351303E-15,-6.8));
#40283=CARTESIAN_POINT('Origin',(222.5,6.87448183661356,-1.58319281140051));
#40284=CARTESIAN_POINT('',(227.5,6.56829561876566,-1.75996950669715));
#40285=CARTESIAN_POINT('',(227.5,6.87448183661356,-1.58319281140051));
#40286=CARTESIAN_POINT('',(222.5,6.56829561876566,-1.75996950669715));
#40287=CARTESIAN_POINT('',(222.5,6.56829561876566,-1.75996950669715));
#40288=CARTESIAN_POINT('',(222.5,6.87448183661356,-1.58319281140051));
#40289=CARTESIAN_POINT('Origin',(222.5,6.6890363470518,-1.79232188733496));
#40290=CARTESIAN_POINT('',(222.5,6.56829561876566,-1.75996950669715));
#40291=CARTESIAN_POINT('Origin',(222.5,6.56829561876566,-1.75996950669715));
#40292=CARTESIAN_POINT('',(227.5,6.56829561876566,-1.75996950669715));
#40293=CARTESIAN_POINT('Origin',(227.5,6.6890363470518,-1.79232188733496));
#40294=CARTESIAN_POINT('Origin',(222.5,6.23047909668029,-3.30849364905389));
#40295=CARTESIAN_POINT('',(227.5,5.88897274573418,-3.4));
#40296=CARTESIAN_POINT('',(227.5,6.23047909668029,-3.30849364905389));
#40297=CARTESIAN_POINT('',(222.5,5.88897274573418,-3.4));
#40298=CARTESIAN_POINT('',(222.5,5.88897274573418,-3.4));
#40299=CARTESIAN_POINT('',(222.5,6.23047909668029,-3.30849364905389));
#40300=CARTESIAN_POINT('Origin',(222.5,5.99722592120723,-3.4625));
#40301=CARTESIAN_POINT('',(222.5,5.88897274573418,-3.4));
#40302=CARTESIAN_POINT('Origin',(222.5,5.88897274573418,-3.4));
#40303=CARTESIAN_POINT('',(227.5,5.88897274573418,-3.4));
#40304=CARTESIAN_POINT('Origin',(227.5,5.99722592120723,-3.4625));
#40305=CARTESIAN_POINT('Origin',(222.5,5.1618795026618,-4.80832611206852));
#40306=CARTESIAN_POINT('',(227.5,4.80832611206852,-4.80832611206852));
#40307=CARTESIAN_POINT('',(227.5,5.1618795026618,-4.80832611206852));
#40308=CARTESIAN_POINT('',(222.5,4.80832611206852,-4.80832611206852));
#40309=CARTESIAN_POINT('',(222.5,4.80832611206852,-4.80832611206852));
#40310=CARTESIAN_POINT('',(222.5,5.1618795026618,-4.80832611206852));
#40311=CARTESIAN_POINT('Origin',(222.5,4.89671445971684,-4.89671445971684));
#40312=CARTESIAN_POINT('',(222.5,4.80832611206852,-4.80832611206852));
#40313=CARTESIAN_POINT('Origin',(222.5,4.80832611206852,-4.80832611206852));
#40314=CARTESIAN_POINT('',(227.5,4.80832611206852,-4.80832611206852));
#40315=CARTESIAN_POINT('Origin',(227.5,4.89671445971684,-4.89671445971684));
#40316=CARTESIAN_POINT('Origin',(222.5,3.7415063509461,-5.9804790966803));
#40317=CARTESIAN_POINT('',(227.5,3.39999999999999,-5.88897274573418));
#40318=CARTESIAN_POINT('',(227.5,3.7415063509461,-5.9804790966803));
#40319=CARTESIAN_POINT('',(222.5,3.39999999999999,-5.88897274573418));
#40320=CARTESIAN_POINT('',(222.5,3.39999999999999,-5.88897274573418));
#40321=CARTESIAN_POINT('',(222.5,3.7415063509461,-5.9804790966803));
#40322=CARTESIAN_POINT('Origin',(222.5,3.46249999999999,-5.99722592120724));
#40323=CARTESIAN_POINT('',(222.5,3.39999999999999,-5.88897274573418));
#40324=CARTESIAN_POINT('Origin',(222.5,3.39999999999999,-5.88897274573418));
#40325=CARTESIAN_POINT('',(227.5,3.39999999999999,-5.88897274573418));
#40326=CARTESIAN_POINT('Origin',(227.5,3.46249999999999,-5.99722592120724));
#40327=CARTESIAN_POINT('Origin',(222.5,2.06615572454504,-6.7450723140623));
#40328=CARTESIAN_POINT('',(227.5,1.75996950669714,-6.56829561876567));
#40329=CARTESIAN_POINT('',(227.5,2.06615572454504,-6.7450723140623));
#40330=CARTESIAN_POINT('',(222.5,1.75996950669714,-6.56829561876567));
#40331=CARTESIAN_POINT('',(222.5,1.75996950669714,-6.56829561876567));
#40332=CARTESIAN_POINT('',(222.5,2.06615572454504,-6.7450723140623));
#40333=CARTESIAN_POINT('Origin',(222.5,1.79232188733495,-6.6890363470518));
#40334=CARTESIAN_POINT('',(222.5,1.75996950669714,-6.56829561876567));
#40335=CARTESIAN_POINT('Origin',(222.5,1.75996950669714,-6.56829561876567));
#40336=CARTESIAN_POINT('',(227.5,1.75996950669714,-6.56829561876567));
#40337=CARTESIAN_POINT('Origin',(227.5,1.79232188733495,-6.6890363470518));
#40338=CARTESIAN_POINT('Origin',(222.5,0.249999999999999,-7.05));
#40339=CARTESIAN_POINT('',(222.5,0.249999999999999,-7.05));
#40340=CARTESIAN_POINT('Origin',(222.5,-1.27210186261431E-15,-6.925));
#40341=CARTESIAN_POINT('Origin',(222.5,-1.58319281140051,-6.87448183661356));
#40342=CARTESIAN_POINT('',(227.5,-1.75996950669715,-6.56829561876566));
#40343=CARTESIAN_POINT('',(227.5,-1.58319281140051,-6.87448183661356));
#40344=CARTESIAN_POINT('',(222.5,-1.75996950669715,-6.56829561876566));
#40345=CARTESIAN_POINT('',(222.5,-1.75996950669715,-6.56829561876566));
#40346=CARTESIAN_POINT('',(222.5,-1.58319281140051,-6.87448183661356));
#40347=CARTESIAN_POINT('Origin',(222.5,-1.79232188733496,-6.6890363470518));
#40348=CARTESIAN_POINT('',(222.5,-1.75996950669715,-6.56829561876566));
#40349=CARTESIAN_POINT('Origin',(222.5,-1.75996950669715,-6.56829561876566));
#40350=CARTESIAN_POINT('',(227.5,-1.75996950669715,-6.56829561876566));
#40351=CARTESIAN_POINT('Origin',(227.5,-1.79232188733496,-6.6890363470518));
#40352=CARTESIAN_POINT('Origin',(222.5,-3.30849364905389,-6.23047909668029));
#40353=CARTESIAN_POINT('',(227.5,-3.4,-5.88897274573418));
#40354=CARTESIAN_POINT('',(227.5,-3.30849364905389,-6.23047909668029));
#40355=CARTESIAN_POINT('',(222.5,-3.4,-5.88897274573418));
#40356=CARTESIAN_POINT('',(222.5,-3.4,-5.88897274573418));
#40357=CARTESIAN_POINT('',(222.5,-3.30849364905389,-6.23047909668029));
#40358=CARTESIAN_POINT('Origin',(222.5,-3.4625,-5.99722592120723));
#40359=CARTESIAN_POINT('',(222.5,-3.4,-5.88897274573418));
#40360=CARTESIAN_POINT('Origin',(222.5,-3.4,-5.88897274573418));
#40361=CARTESIAN_POINT('',(227.5,-3.4,-5.88897274573418));
#40362=CARTESIAN_POINT('Origin',(227.5,-3.4625,-5.99722592120723));
#40363=CARTESIAN_POINT('Origin',(222.5,-4.80832611206853,-5.16187950266179));
#40364=CARTESIAN_POINT('',(227.5,-4.80832611206853,-4.80832611206852));
#40365=CARTESIAN_POINT('',(227.5,-4.80832611206853,-5.16187950266179));
#40366=CARTESIAN_POINT('',(222.5,-4.80832611206853,-4.80832611206852));
#40367=CARTESIAN_POINT('',(222.5,-4.80832611206853,-4.80832611206852));
#40368=CARTESIAN_POINT('',(222.5,-4.80832611206853,-5.16187950266179));
#40369=CARTESIAN_POINT('Origin',(222.5,-4.89671445971684,-4.89671445971684));
#40370=CARTESIAN_POINT('',(222.5,-4.80832611206853,-4.80832611206852));
#40371=CARTESIAN_POINT('Origin',(222.5,-4.80832611206853,-4.80832611206852));
#40372=CARTESIAN_POINT('',(227.5,-4.80832611206853,-4.80832611206852));
#40373=CARTESIAN_POINT('Origin',(227.5,-4.89671445971684,-4.89671445971684));
#40374=CARTESIAN_POINT('Origin',(222.5,-5.98047909668029,-3.74150635094611));
#40375=CARTESIAN_POINT('',(227.5,-5.88897274573418,-3.4));
#40376=CARTESIAN_POINT('',(227.5,-5.98047909668029,-3.74150635094611));
#40377=CARTESIAN_POINT('',(222.5,-5.88897274573418,-3.4));
#40378=CARTESIAN_POINT('',(222.5,-5.88897274573418,-3.4));
#40379=CARTESIAN_POINT('',(222.5,-5.98047909668029,-3.74150635094611));
#40380=CARTESIAN_POINT('Origin',(222.5,-5.99722592120724,-3.4625));
#40381=CARTESIAN_POINT('',(222.5,-5.88897274573418,-3.4));
#40382=CARTESIAN_POINT('Origin',(222.5,-5.88897274573418,-3.4));
#40383=CARTESIAN_POINT('',(227.5,-5.88897274573418,-3.4));
#40384=CARTESIAN_POINT('Origin',(227.5,-5.99722592120724,-3.4625));
#40385=CARTESIAN_POINT('Origin',(222.5,-6.7450723140623,-2.06615572454504));
#40386=CARTESIAN_POINT('',(227.5,-6.56829561876567,-1.75996950669714));
#40387=CARTESIAN_POINT('',(227.5,-6.7450723140623,-2.06615572454504));
#40388=CARTESIAN_POINT('',(222.5,-6.56829561876567,-1.75996950669714));
#40389=CARTESIAN_POINT('',(222.5,-6.56829561876567,-1.75996950669714));
#40390=CARTESIAN_POINT('',(222.5,-6.7450723140623,-2.06615572454504));
#40391=CARTESIAN_POINT('Origin',(222.5,-6.6890363470518,-1.79232188733495));
#40392=CARTESIAN_POINT('',(222.5,-6.56829561876567,-1.75996950669714));
#40393=CARTESIAN_POINT('Origin',(222.5,-6.56829561876567,-1.75996950669714));
#40394=CARTESIAN_POINT('',(227.5,-6.56829561876567,-1.75996950669714));
#40395=CARTESIAN_POINT('Origin',(227.5,-6.6890363470518,-1.79232188733495));
#40396=CARTESIAN_POINT('Origin',(222.5,-7.05,-0.249999999999999));
#40397=CARTESIAN_POINT('',(227.5,-6.8,8.327598234202E-16));
#40398=CARTESIAN_POINT('',(227.5,-7.05,-0.249999999999999));
#40399=CARTESIAN_POINT('',(222.5,-6.8,8.327598234202E-16));
#40400=CARTESIAN_POINT('',(222.5,-6.8,8.327598234202E-16));
#40401=CARTESIAN_POINT('',(222.5,-7.05,-0.249999999999999));
#40402=CARTESIAN_POINT('Origin',(222.5,-6.925,8.48067908409542E-16));
#40403=CARTESIAN_POINT('',(222.5,-6.8,8.327598234202E-16));
#40404=CARTESIAN_POINT('Origin',(222.5,-6.8,8.327598234202E-16));
#40405=CARTESIAN_POINT('',(227.5,-6.8,8.327598234202E-16));
#40406=CARTESIAN_POINT('Origin',(227.5,-6.925,8.48067908409542E-16));
#40407=CARTESIAN_POINT('Origin',(222.5,-6.87448183661356,1.58319281140051));
#40408=CARTESIAN_POINT('',(227.5,-6.56829561876566,1.75996950669714));
#40409=CARTESIAN_POINT('',(227.5,-6.87448183661356,1.58319281140051));
#40410=CARTESIAN_POINT('',(222.5,-6.56829561876566,1.75996950669714));
#40411=CARTESIAN_POINT('',(222.5,-6.56829561876566,1.75996950669714));
#40412=CARTESIAN_POINT('',(222.5,-6.87448183661356,1.58319281140051));
#40413=CARTESIAN_POINT('Origin',(222.5,-6.6890363470518,1.79232188733496));
#40414=CARTESIAN_POINT('',(222.5,-6.56829561876566,1.75996950669714));
#40415=CARTESIAN_POINT('Origin',(222.5,-6.56829561876566,1.75996950669714));
#40416=CARTESIAN_POINT('',(227.5,-6.56829561876566,1.75996950669714));
#40417=CARTESIAN_POINT('Origin',(227.5,-6.6890363470518,1.79232188733496));
#40418=CARTESIAN_POINT('Origin',(222.5,-6.23047909668029,3.30849364905389));
#40419=CARTESIAN_POINT('',(227.5,-5.88897274573418,3.4));
#40420=CARTESIAN_POINT('',(227.5,-6.23047909668029,3.30849364905389));
#40421=CARTESIAN_POINT('',(222.5,-5.88897274573418,3.4));
#40422=CARTESIAN_POINT('',(222.5,-5.88897274573418,3.4));
#40423=CARTESIAN_POINT('',(222.5,-6.23047909668029,3.30849364905389));
#40424=CARTESIAN_POINT('Origin',(222.5,-5.99722592120724,3.4625));
#40425=CARTESIAN_POINT('',(222.5,-5.88897274573418,3.4));
#40426=CARTESIAN_POINT('Origin',(222.5,-5.88897274573418,3.4));
#40427=CARTESIAN_POINT('',(227.5,-5.88897274573418,3.4));
#40428=CARTESIAN_POINT('Origin',(227.5,-5.99722592120724,3.4625));
#40429=CARTESIAN_POINT('Origin',(222.5,-5.1618795026618,4.80832611206852));
#40430=CARTESIAN_POINT('',(227.5,-4.80832611206852,4.80832611206852));
#40431=CARTESIAN_POINT('',(227.5,-5.1618795026618,4.80832611206852));
#40432=CARTESIAN_POINT('',(222.5,-4.80832611206852,4.80832611206852));
#40433=CARTESIAN_POINT('',(222.5,-4.80832611206852,4.80832611206852));
#40434=CARTESIAN_POINT('',(222.5,-5.1618795026618,4.80832611206852));
#40435=CARTESIAN_POINT('Origin',(222.5,-4.89671445971684,4.89671445971684));
#40436=CARTESIAN_POINT('',(222.5,-4.80832611206852,4.80832611206852));
#40437=CARTESIAN_POINT('Origin',(222.5,-4.80832611206852,4.80832611206852));
#40438=CARTESIAN_POINT('',(227.5,-4.80832611206852,4.80832611206852));
#40439=CARTESIAN_POINT('Origin',(227.5,-4.89671445971684,4.89671445971684));
#40440=CARTESIAN_POINT('Origin',(222.5,-3.74150635094611,5.98047909668029));
#40441=CARTESIAN_POINT('',(227.5,-3.4,5.88897274573418));
#40442=CARTESIAN_POINT('',(227.5,-3.74150635094611,5.98047909668029));
#40443=CARTESIAN_POINT('',(222.5,-3.4,5.88897274573418));
#40444=CARTESIAN_POINT('',(222.5,-3.4,5.88897274573418));
#40445=CARTESIAN_POINT('',(222.5,-3.74150635094611,5.98047909668029));
#40446=CARTESIAN_POINT('Origin',(222.5,-3.4625,5.99722592120724));
#40447=CARTESIAN_POINT('',(222.5,-3.4,5.88897274573418));
#40448=CARTESIAN_POINT('Origin',(222.5,-3.4,5.88897274573418));
#40449=CARTESIAN_POINT('',(227.5,-3.4,5.88897274573418));
#40450=CARTESIAN_POINT('Origin',(227.5,-3.4625,5.99722592120724));
#40451=CARTESIAN_POINT('Origin',(222.5,-2.06615572454504,6.7450723140623));
#40452=CARTESIAN_POINT('',(227.5,-1.75996950669714,6.56829561876566));
#40453=CARTESIAN_POINT('',(227.5,-2.06615572454504,6.7450723140623));
#40454=CARTESIAN_POINT('',(222.5,-1.75996950669714,6.56829561876566));
#40455=CARTESIAN_POINT('',(222.5,-1.75996950669714,6.56829561876566));
#40456=CARTESIAN_POINT('',(222.5,-2.06615572454504,6.7450723140623));
#40457=CARTESIAN_POINT('Origin',(222.5,-1.79232188733496,6.6890363470518));
#40458=CARTESIAN_POINT('',(222.5,-1.75996950669714,6.56829561876566));
#40459=CARTESIAN_POINT('Origin',(222.5,-1.75996950669714,6.56829561876566));
#40460=CARTESIAN_POINT('',(227.5,-1.75996950669714,6.56829561876566));
#40461=CARTESIAN_POINT('Origin',(227.5,-1.79232188733496,6.6890363470518));
#40462=CARTESIAN_POINT('Origin',(222.5,-0.25,7.05));
#40463=CARTESIAN_POINT('',(222.5,4.163799117101E-16,6.8));
#40464=CARTESIAN_POINT('',(222.5,4.163799117101E-16,6.8));
#40465=CARTESIAN_POINT('',(222.5,-0.25,7.05));
#40466=CARTESIAN_POINT('Origin',(222.5,4.24033954204771E-16,6.925));
#40467=CARTESIAN_POINT('',(222.5,4.163799117101E-16,6.8));
#40468=CARTESIAN_POINT('Origin',(222.5,4.163799117101E-16,6.8));
#40469=CARTESIAN_POINT('Origin',(222.5,1.58319281140051,6.87448183661356));
#40470=CARTESIAN_POINT('',(227.5,1.75996950669714,6.56829561876566));
#40471=CARTESIAN_POINT('',(227.5,1.58319281140051,6.87448183661356));
#40472=CARTESIAN_POINT('',(222.5,1.75996950669714,6.56829561876566));
#40473=CARTESIAN_POINT('',(222.5,1.75996950669714,6.56829561876566));
#40474=CARTESIAN_POINT('',(222.5,1.58319281140051,6.87448183661356));
#40475=CARTESIAN_POINT('Origin',(222.5,1.79232188733496,6.6890363470518));
#40476=CARTESIAN_POINT('',(222.5,1.75996950669714,6.56829561876566));
#40477=CARTESIAN_POINT('Origin',(222.5,1.75996950669714,6.56829561876566));
#40478=CARTESIAN_POINT('',(227.5,1.75996950669714,6.56829561876566));
#40479=CARTESIAN_POINT('Origin',(227.5,1.79232188733496,6.6890363470518));
#40480=CARTESIAN_POINT('Origin',(222.5,3.30849364905389,6.23047909668029));
#40481=CARTESIAN_POINT('',(227.5,3.4,5.88897274573418));
#40482=CARTESIAN_POINT('',(227.5,3.30849364905389,6.23047909668029));
#40483=CARTESIAN_POINT('',(222.5,3.4,5.88897274573418));
#40484=CARTESIAN_POINT('',(222.5,3.4,5.88897274573418));
#40485=CARTESIAN_POINT('',(222.5,3.30849364905389,6.23047909668029));
#40486=CARTESIAN_POINT('Origin',(222.5,3.4625,5.99722592120724));
#40487=CARTESIAN_POINT('',(222.5,3.4,5.88897274573418));
#40488=CARTESIAN_POINT('Origin',(222.5,3.4,5.88897274573418));
#40489=CARTESIAN_POINT('',(227.5,3.4,5.88897274573418));
#40490=CARTESIAN_POINT('Origin',(227.5,3.4625,5.99722592120724));
#40491=CARTESIAN_POINT('Origin',(222.5,4.80832611206852,5.1618795026618));
#40492=CARTESIAN_POINT('',(227.5,4.80832611206852,4.80832611206852));
#40493=CARTESIAN_POINT('',(227.5,4.80832611206852,5.1618795026618));
#40494=CARTESIAN_POINT('',(222.5,4.80832611206852,4.80832611206852));
#40495=CARTESIAN_POINT('',(222.5,4.80832611206852,4.80832611206852));
#40496=CARTESIAN_POINT('',(222.5,4.80832611206852,5.1618795026618));
#40497=CARTESIAN_POINT('Origin',(222.5,4.89671445971684,4.89671445971684));
#40498=CARTESIAN_POINT('',(222.5,4.80832611206852,4.80832611206852));
#40499=CARTESIAN_POINT('Origin',(222.5,4.80832611206852,4.80832611206852));
#40500=CARTESIAN_POINT('',(227.5,4.80832611206852,4.80832611206852));
#40501=CARTESIAN_POINT('Origin',(227.5,4.89671445971684,4.89671445971684));
#40502=CARTESIAN_POINT('Origin',(222.5,5.98047909668029,3.74150635094611));
#40503=CARTESIAN_POINT('',(227.5,5.88897274573418,3.4));
#40504=CARTESIAN_POINT('',(227.5,5.98047909668029,3.74150635094611));
#40505=CARTESIAN_POINT('',(222.5,5.88897274573418,3.4));
#40506=CARTESIAN_POINT('',(222.5,5.88897274573418,3.4));
#40507=CARTESIAN_POINT('',(222.5,5.98047909668029,3.74150635094611));
#40508=CARTESIAN_POINT('Origin',(222.5,5.99722592120724,3.4625));
#40509=CARTESIAN_POINT('',(222.5,5.88897274573418,3.4));
#40510=CARTESIAN_POINT('Origin',(222.5,5.88897274573418,3.4));
#40511=CARTESIAN_POINT('',(227.5,5.88897274573418,3.4));
#40512=CARTESIAN_POINT('Origin',(227.5,5.99722592120724,3.4625));
#40513=CARTESIAN_POINT('Origin',(222.5,6.7450723140623,2.06615572454504));
#40514=CARTESIAN_POINT('',(227.5,6.56829561876566,1.75996950669714));
#40515=CARTESIAN_POINT('',(227.5,6.7450723140623,2.06615572454504));
#40516=CARTESIAN_POINT('',(222.5,6.56829561876566,1.75996950669714));
#40517=CARTESIAN_POINT('',(222.5,6.56829561876566,1.75996950669714));
#40518=CARTESIAN_POINT('',(222.5,6.7450723140623,2.06615572454504));
#40519=CARTESIAN_POINT('Origin',(222.5,6.6890363470518,1.79232188733496));
#40520=CARTESIAN_POINT('',(222.5,6.56829561876566,1.75996950669714));
#40521=CARTESIAN_POINT('Origin',(222.5,6.56829561876566,1.75996950669714));
#40522=CARTESIAN_POINT('',(227.5,6.56829561876566,1.75996950669714));
#40523=CARTESIAN_POINT('Origin',(227.5,6.6890363470518,1.79232188733496));
#40524=CARTESIAN_POINT('Origin',(222.5,7.05,0.25));
#40525=CARTESIAN_POINT('',(227.5,6.8,0.));
#40526=CARTESIAN_POINT('',(227.5,7.05,0.25));
#40527=CARTESIAN_POINT('',(222.5,6.8,0.));
#40528=CARTESIAN_POINT('',(222.5,6.8,0.));
#40529=CARTESIAN_POINT('',(222.5,7.05,0.25));
#40530=CARTESIAN_POINT('Origin',(222.5,6.925,0.));
#40531=CARTESIAN_POINT('',(222.5,6.8,0.));
#40532=CARTESIAN_POINT('Origin',(222.5,6.8,0.));
#40533=CARTESIAN_POINT('',(227.5,6.8,0.));
#40534=CARTESIAN_POINT('Origin',(227.5,6.925,0.));
#40535=CARTESIAN_POINT('Origin',(209.,4.6,0.));
#40536=CARTESIAN_POINT('',(209.,-4.59999999999999,-5.63337527607781E-16));
#40537=CARTESIAN_POINT('Origin',(209.,0.,0.));
#40538=CARTESIAN_POINT('Origin',(209.2,0.,0.));
#40539=CARTESIAN_POINT('',(209.2,-4.8,-5.87830463590729E-16));
#40540=CARTESIAN_POINT('Origin',(215.7,0.,0.));
#40541=CARTESIAN_POINT('Origin',(222.,0.,0.));
#40542=CARTESIAN_POINT('Origin',(222.,6.6,0.));
#40543=CARTESIAN_POINT('',(222.,-6.60000000000001,-8.08266887437254E-16));
#40544=CARTESIAN_POINT('Origin',(222.,0.,0.));
#40545=CARTESIAN_POINT('Origin',(222.2,0.,0.));
#40546=CARTESIAN_POINT('',(222.2,-6.8,-8.327598234202E-16));
#40547=CARTESIAN_POINT('Origin',(227.8,0.,0.));
#40548=CARTESIAN_POINT('',(0.,0.,0.));
#40549=CARTESIAN_POINT('Origin',(224.25,0.,0.));
#40550=CARTESIAN_POINT('',(224.,10.,-1.22464679914735E-15));
#40551=CARTESIAN_POINT('Origin',(224.,0.,0.));
#40552=CARTESIAN_POINT('',(224.5,9.5,1.16341445918999E-15));
#40553=CARTESIAN_POINT('',(224.25,9.75,-1.19403062916867E-15));
#40554=CARTESIAN_POINT('',(224.5,-9.5,-1.16341445918999E-15));
#40555=CARTESIAN_POINT('Origin',(224.5,0.,0.));
#40556=CARTESIAN_POINT('Origin',(224.5,0.,0.));
#40557=CARTESIAN_POINT('Origin',(259.,0.,0.));
#40558=CARTESIAN_POINT('',(294.,-9.5,-1.16341445918999E-15));
#40559=CARTESIAN_POINT('Origin',(294.,0.,0.));
#40560=CARTESIAN_POINT('',(259.,-9.5,-1.16341445918999E-15));
#40561=CARTESIAN_POINT('Origin',(224.,12.05,0.));
#40562=CARTESIAN_POINT('',(224.,-12.05,-1.47569939297256E-15));
#40563=CARTESIAN_POINT('Origin',(224.,0.,0.));
#40564=CARTESIAN_POINT('Origin',(215.,0.,0.));
#40565=CARTESIAN_POINT('',(206.,-12.05,-1.47569939297256E-15));
#40566=CARTESIAN_POINT('',(215.,-12.05,-1.47569939297256E-15));
#40567=CARTESIAN_POINT('Origin',(206.,0.,0.));
#40568=CARTESIAN_POINT('Origin',(206.,12.6,0.));
#40569=CARTESIAN_POINT('',(206.,-12.6,-1.54305496692566E-15));
#40570=CARTESIAN_POINT('Origin',(206.,0.,0.));
#40571=CARTESIAN_POINT('Origin',(206.2,0.,0.));
#40572=CARTESIAN_POINT('',(206.4,-13.,-1.59204083889156E-15));
#40573=CARTESIAN_POINT('Origin',(206.4,0.,0.));
#40574=CARTESIAN_POINT('',(206.2,-12.8,-1.56754790290861E-15));
#40575=CARTESIAN_POINT('Origin',(251.7,0.,0.));
#40576=CARTESIAN_POINT('',(297.,-13.,-1.59204083889156E-15));
#40577=CARTESIAN_POINT('Origin',(297.,0.,0.));
#40578=CARTESIAN_POINT('',(251.7,-13.,-1.59204083889156E-15));
#40579=CARTESIAN_POINT('Origin',(298.5,0.,0.));
#40580=CARTESIAN_POINT('',(300.,-10.,-1.22464679914735E-15));
#40581=CARTESIAN_POINT('Origin',(300.,0.,0.));
#40582=CARTESIAN_POINT('',(298.5,-11.5,-1.40834381901946E-15));
#40583=CARTESIAN_POINT('Origin',(300.,0.,0.));
#40584=CARTESIAN_POINT('Origin',(294.,9.5,0.));
#40585=CARTESIAN_POINT('',(0.,0.,0.));
#40586=CARTESIAN_POINT('Origin',(304.920943058496,0.,-2.59451884383998E-16));
#40587=CARTESIAN_POINT('',(305.,7.50000000000002,-9.18485099360518E-16));
#40588=CARTESIAN_POINT('Origin',(305.,0.,0.));
#40589=CARTESIAN_POINT('',(304.841886116992,8.47434164902529,1.03780753753599E-15));
#40590=CARTESIAN_POINT('',(304.920943058496,7.98717082451265,9.78146318448255E-16));
#40591=CARTESIAN_POINT('',(304.841886116992,-8.47434164902529,-1.03780753753599E-15));
#40592=CARTESIAN_POINT('Origin',(304.841886116992,0.,-5.18903768767996E-16));
#40593=CARTESIAN_POINT('Origin',(304.841886116992,0.,-5.18903768767996E-16));
#40594=CARTESIAN_POINT('Origin',(304.25,0.,0.));
#40595=CARTESIAN_POINT('',(303.658113883008,-12.0256583509747,-1.47271840071608E-15));
#40596=CARTESIAN_POINT('',(304.25,-10.25,-1.25526296912604E-15));
#40597=CARTESIAN_POINT('',(303.658113883008,12.0256583509747,-1.47271840071608E-15));
#40598=CARTESIAN_POINT('Origin',(303.658113883008,0.,-7.36359200358042E-16));
#40599=CARTESIAN_POINT('Origin',(303.658113883008,0.,-7.36359200358042E-16));
#40600=CARTESIAN_POINT('Origin',(305.,0.,0.));
#40601=CARTESIAN_POINT('Origin',(303.375623573703,0.,-7.59779368581073E-16));
#40602=CARTESIAN_POINT('',(303.093133264397,12.7906190968596,1.56639907360821E-15));
#40603=CARTESIAN_POINT('',(303.375623573703,12.4081387239171,1.51955873716215E-15));
#40604=CARTESIAN_POINT('',(303.093133264397,-12.7906190968596,-1.56639907360821E-15));
#40605=CARTESIAN_POINT('Origin',(303.093133264397,0.,-7.83199536804103E-16));
#40606=CARTESIAN_POINT('Origin',(303.093133264397,0.,-7.83199536804103E-16));
#40607=CARTESIAN_POINT('Origin',(301.75,0.,0.));
#40608=CARTESIAN_POINT('',(300.406866735603,-14.7093809031404,-1.80137962404702E-15));
#40609=CARTESIAN_POINT('',(301.75,-13.75,-1.68388934882761E-15));
#40610=CARTESIAN_POINT('',(300.406866735603,14.7093809031404,-1.80137962404702E-15));
#40611=CARTESIAN_POINT('Origin',(300.406866735603,0.,-9.00689812023508E-16));
#40612=CARTESIAN_POINT('Origin',(300.406866735603,0.,-9.00689812023508E-16));
#40613=CARTESIAN_POINT('Origin',(299.953433367802,0.,-4.50344906011754E-16));
#40614=CARTESIAN_POINT('',(299.5,15.,1.83697019872103E-15));
#40615=CARTESIAN_POINT('',(299.953433367802,14.8546904515702,1.81917491138402E-15));
#40616=CARTESIAN_POINT('',(299.5,-15.,-1.83697019872103E-15));
#40617=CARTESIAN_POINT('Origin',(299.5,0.,0.));
#40618=CARTESIAN_POINT('Origin',(299.5,0.,0.));
#40619=CARTESIAN_POINT('Origin',(254.35,0.,0.));
#40620=CARTESIAN_POINT('',(208.7,-15.,-1.83697019872103E-15));
#40621=CARTESIAN_POINT('',(254.35,-15.,-1.83697019872103E-15));
#40622=CARTESIAN_POINT('Origin',(208.7,0.,0.));
#40623=CARTESIAN_POINT('Origin',(252.5,0.,0.));
#40624=CARTESIAN_POINT('',(297.,-13.,-1.59204083889156E-15));
#40625=CARTESIAN_POINT('Origin',(297.,0.,0.));
#40626=CARTESIAN_POINT('',(208.,-13.,-1.59204083889156E-15));
#40627=CARTESIAN_POINT('',(252.5,-13.,-1.59204083889156E-15));
#40628=CARTESIAN_POINT('Origin',(208.,0.,0.));
#40629=CARTESIAN_POINT('Origin',(208.,14.3,0.));
#40630=CARTESIAN_POINT('',(208.,-14.3,-1.75124492278071E-15));
#40631=CARTESIAN_POINT('Origin',(208.,0.,0.));
#40632=CARTESIAN_POINT('Origin',(208.35,0.,0.));
#40633=CARTESIAN_POINT('',(208.35,-14.65,-1.79410756075087E-15));
#40634=CARTESIAN_POINT('Origin',(300.,10.,0.));
#40635=CARTESIAN_POINT('',(300.,-10.,-1.22464679914735E-15));
#40636=CARTESIAN_POINT('Origin',(300.,0.,0.));
#40637=CARTESIAN_POINT('Origin',(298.5,0.,0.));
#40638=CARTESIAN_POINT('',(298.5,-11.5,-1.40834381901946E-15));
#40639=CARTESIAN_POINT('',(0.,0.,0.));
#40640=CARTESIAN_POINT('Origin',(8.75,0.,0.));
#40641=CARTESIAN_POINT('',(2.76432045465689,-4.94788959559308,0.00239028935128519));
#40642=CARTESIAN_POINT('',(2.6196795453431,-4.94443125321576,0.00146311145371448));
#40643=CARTESIAN_POINT('',(8.75,-4.942,-6.05220448138622E-16));
#40644=CARTESIAN_POINT('',(2.442,2.17246025283987,4.44279282409917));
#40645=CARTESIAN_POINT('Ctrl Pts',(2.76432045465689,-4.94788959559308,0.00239028935128519));
#40646=CARTESIAN_POINT('Ctrl Pts',(2.75931691497812,-4.94892132323628,0.157204467377098));
#40647=CARTESIAN_POINT('Ctrl Pts',(2.75431337529936,-4.94231374587349,0.311936106973573));
#40648=CARTESIAN_POINT('Ctrl Pts',(2.74930983562059,-4.9277840870703,0.465924016286531));
#40649=CARTESIAN_POINT('Ctrl Pts',(2.6962765448657,-4.7737819866876,2.09806567831472));
#40650=CARTESIAN_POINT('Ctrl Pts',(2.6432432541108,-3.72979678823222,3.64665513416632));
#40651=CARTESIAN_POINT('Ctrl Pts',(2.59020996335591,-2.27271757376403,4.39850416463932));
#40652=CARTESIAN_POINT('Ctrl Pts',(2.54080664223727,-0.915371059847599,
5.09889138475105));
#40653=CARTESIAN_POINT('Ctrl Pts',(2.49140332111864,0.80045472016787,5.10787444045995));
#40654=CARTESIAN_POINT('Ctrl Pts',(2.442,2.17574915139364,4.44508346536535));
#40655=CARTESIAN_POINT('',(2.442,-2.16917135428613,4.44050218283298));
#40656=CARTESIAN_POINT('Origin',(2.442,0.,0.));
#40657=CARTESIAN_POINT('Ctrl Pts',(2.442,-2.16917135428612,4.44050218283299));
#40658=CARTESIAN_POINT('Ctrl Pts',(2.46851664537745,-2.9089989675068,4.07909871997413));
#40659=CARTESIAN_POINT('Ctrl Pts',(2.49503329075489,-3.55111543888009,3.52928885898635));
#40660=CARTESIAN_POINT('Ctrl Pts',(2.52154993613233,-4.02901758456164,2.85775650263327));
#40661=CARTESIAN_POINT('Ctrl Pts',(2.54806658150978,-4.5069197302432,2.18622414628017));
#40662=CARTESIAN_POINT('Ctrl Pts',(2.57458322688722,-4.82060755023301,1.39296929456177));
#40663=CARTESIAN_POINT('Ctrl Pts',(2.60109987226467,-4.91429750933697,0.576285982800623));
#40664=CARTESIAN_POINT('Ctrl Pts',(2.60729309662415,-4.93617972440233,0.385541531216247));
#40665=CARTESIAN_POINT('Ctrl Pts',(2.61348632098362,-4.94606100888929,0.193519052102877));
#40666=CARTESIAN_POINT('Ctrl Pts',(2.6196795453431,-4.94443125321576,0.00146311145371448));
#40667=CARTESIAN_POINT('Origin',(8.75,0.,0.));
#40668=CARTESIAN_POINT('',(3.76432045465689,-4.93571920292385,0.00301700625176843));
#40669=CARTESIAN_POINT('',(3.6196795453431,-4.93504902497496,0.00248727919068638));
#40670=CARTESIAN_POINT('',(8.75,-4.942,-6.05220448138622E-16));
#40671=CARTESIAN_POINT('Ctrl Pts',(3.76432045465689,-4.93571920292385,0.00301700625176843));
#40672=CARTESIAN_POINT('Ctrl Pts',(3.74418332617413,-4.9392039814057,0.630130822225083));
#40673=CARTESIAN_POINT('Ctrl Pts',(3.72404619769136,-4.82845404842863,1.25605983210146));
#40674=CARTESIAN_POINT('Ctrl Pts',(3.70390906920859,-4.59783645110691,1.83417191416958));
#40675=CARTESIAN_POINT('Ctrl Pts',(3.6508757784537,-3.99048023830714,3.3566921763544));
#40676=CARTESIAN_POINT('Ctrl Pts',(3.59784248769881,-2.55173533303798,4.54755958365334));
#40677=CARTESIAN_POINT('Ctrl Pts',(3.54480919694392,-0.942516547825695,
4.85964727579633));
#40678=CARTESIAN_POINT('Ctrl Pts',(3.49177590618903,0.666702237386595,5.17173496793932));
#40679=CARTESIAN_POINT('Ctrl Pts',(3.43874261543414,2.44639490254201,4.60504294492635));
#40680=CARTESIAN_POINT('Ctrl Pts',(3.38570932467925,3.5788553706631,3.41997949552812));
#40681=CARTESIAN_POINT('Ctrl Pts',(3.33267603392436,4.71131583878419,2.23491604612988));
#40682=CARTESIAN_POINT('Ctrl Pts',(3.27964274316948,5.19654410987096,0.431481170346373));
#40683=CARTESIAN_POINT('Ctrl Pts',(3.22660945241459,4.8118217284371,-1.16194233954266));
#40684=CARTESIAN_POINT('Ctrl Pts',(3.1735761616597,4.42709934700323,-2.7553658494317));
#40685=CARTESIAN_POINT('Ctrl Pts',(3.12054287090481,3.17242631304874,-4.13877799342627));
#40686=CARTESIAN_POINT('Ctrl Pts',(3.06750958014992,1.62382688421027,-4.67638660621195));
#40687=CARTESIAN_POINT('Ctrl Pts',(3.01447628939503,0.0752274553718063,
-5.21399521899763));
#40688=CARTESIAN_POINT('Ctrl Pts',(2.96144299864014,-1.76729836835063,-4.90580030057443));
#40689=CARTESIAN_POINT('Ctrl Pts',(2.90840970788525,-3.05655177905683,-3.89385590726044));
#40690=CARTESIAN_POINT('Ctrl Pts',(2.86037995680913,-4.22416780870228,-2.97738558037873));
#40691=CARTESIAN_POINT('Ctrl Pts',(2.81235020573301,-4.93798588240953,-1.48369494450495));
#40692=CARTESIAN_POINT('Ctrl Pts',(2.76432045465689,-4.94788959559308,0.00239028935128519));
#40693=CARTESIAN_POINT('Ctrl Pts',(2.6196795453431,-4.94443125321576,0.00146311145371448));
#40694=CARTESIAN_POINT('Ctrl Pts',(2.66651961173851,-4.93210522407074,-1.45107800275172));
#40695=CARTESIAN_POINT('Ctrl Pts',(2.71335967813392,-4.26133958869745,-2.90553314037676));
#40696=CARTESIAN_POINT('Ctrl Pts',(2.76019974452934,-3.14406853058354,-3.82348377368421));
#40697=CARTESIAN_POINT('Ctrl Pts',(2.81323303528422,-1.87907115895764,-4.86280644295348));
#40698=CARTESIAN_POINT('Ctrl Pts',(2.86626632603911,-0.0416879410413212,
-5.21437131779874));
#40699=CARTESIAN_POINT('Ctrl Pts',(2.919299616794,1.51912370630509,-4.71214944827796));
#40700=CARTESIAN_POINT('Ctrl Pts',(2.97233290754889,3.0799353536515,-4.20992757875717));
#40701=CARTESIAN_POINT('Ctrl Pts',(3.02536619830378,4.364175430428,-2.85391896487034));
#40702=CARTESIAN_POINT('Ctrl Pts',(3.07839948905867,4.78425699578354,-1.26926289529364));
#40703=CARTESIAN_POINT('Ctrl Pts',(3.13143277981356,5.20433856113907,0.315393174283052));
#40704=CARTESIAN_POINT('Ctrl Pts',(3.18446607056845,4.76026161507364,2.12869669954961));
#40705=CARTESIAN_POINT('Ctrl Pts',(3.23749936132334,3.6548001293483,3.33872180443716));
#40706=CARTESIAN_POINT('Ctrl Pts',(3.29053265207823,2.54933864362295,4.54874690932471));
#40707=CARTESIAN_POINT('Ctrl Pts',(3.34356594283312,0.782492618237691,5.15549359383325));
#40708=CARTESIAN_POINT('Ctrl Pts',(3.39659923358801,-0.833393310877007,
4.87963769585482));
#40709=CARTESIAN_POINT('Ctrl Pts',(3.4496325243429,-2.44927923999171,4.60378179787639));
#40710=CARTESIAN_POINT('Ctrl Pts',(3.50266581509778,-3.91420507283584,3.44532331741098));
#40711=CARTESIAN_POINT('Ctrl Pts',(3.55569910585267,-4.55550993645389,1.93676831562686));
#40712=CARTESIAN_POINT('Ctrl Pts',(3.57702591901615,-4.81340434226065,1.33011784736587));
#40713=CARTESIAN_POINT('Ctrl Pts',(3.59835273217962,-4.93810551184841,0.666850937312143));
#40714=CARTESIAN_POINT('Ctrl Pts',(3.6196795453431,-4.93504902497496,0.00248727919068638));
#40715=CARTESIAN_POINT('Origin',(8.75,0.,0.));
#40716=CARTESIAN_POINT('',(4.76432045465689,-4.93730273339884,-0.00383068200619119));
#40717=CARTESIAN_POINT('',(4.61967954534309,-4.93822978717952,-0.00413487577884502));
#40718=CARTESIAN_POINT('',(8.75,-4.942,-6.05220448138622E-16));
#40719=CARTESIAN_POINT('Ctrl Pts',(4.76432045465689,-4.93730273339884,-0.00383068200619119));
#40720=CARTESIAN_POINT('Ctrl Pts',(4.72904973737013,-4.92940489017672,1.09369834277235));
#40721=CARTESIAN_POINT('Ctrl Pts',(4.69377902008336,-4.56844519037125,2.1959421476368));
#40722=CARTESIAN_POINT('Ctrl Pts',(4.6585083027966,-3.89588421868249,3.05392627541324));
#40723=CARTESIAN_POINT('Ctrl Pts',(4.60547501204171,-2.88461696057815,4.34399705399991));
#40724=CARTESIAN_POINT('Ctrl Pts',(4.55244172128681,-1.16887112604092,5.08183738578865));
#40725=CARTESIAN_POINT('Ctrl Pts',(4.49940843053193,0.463129480941426,4.92847788550683));
#40726=CARTESIAN_POINT('Ctrl Pts',(4.44637513977704,2.09513008792377,4.77511838522502));
#40727=CARTESIAN_POINT('Ctrl Pts',(4.39334184902215,3.64338546735125,3.73055905287266));
#40728=CARTESIAN_POINT('Ctrl Pts',(4.34030855826726,4.39661485369635,2.27467863331172));
#40729=CARTESIAN_POINT('Ctrl Pts',(4.28727526751237,5.14984424004146,0.818798213750785));
#40730=CARTESIAN_POINT('Ctrl Pts',(4.23424197675748,5.10804763330419,-1.04840329301873));
#40731=CARTESIAN_POINT('Ctrl Pts',(4.18120868600259,4.29043066949209,-2.46912382375875));
#40732=CARTESIAN_POINT('Ctrl Pts',(4.1281753952477,3.47281370567999,-3.88984435449878));
#40733=CARTESIAN_POINT('Ctrl Pts',(4.07514210449281,1.87937638479307,-4.8640839092093));
#40734=CARTESIAN_POINT('Ctrl Pts',(4.02210881373792,0.242146596270669,-4.94426553960403));
#40735=CARTESIAN_POINT('Ctrl Pts',(3.96907552298303,-1.39508319225173,-5.02444716999875));
#40736=CARTESIAN_POINT('Ctrl Pts',(3.91604223222815,-3.07610544840959,-4.21057087607769));
#40737=CARTESIAN_POINT('Ctrl Pts',(3.86300894147326,-4.02863281632334,-2.87654617058181));
#40738=CARTESIAN_POINT('Ctrl Pts',(3.83011277920114,-4.61947857410121,-2.04906040527569));
#40739=CARTESIAN_POINT('Ctrl Pts',(3.79721661692902,-4.93002644297949,-1.02144076939389));
#40740=CARTESIAN_POINT('Ctrl Pts',(3.76432045465689,-4.93571920292385,0.00301700625176843));
#40741=CARTESIAN_POINT('Ctrl Pts',(3.6196795453431,-4.93504902497496,0.00248727919068638));
#40742=CARTESIAN_POINT('Ctrl Pts',(3.65138602293451,-4.93050495963249,-0.985219195157505));
#40743=CARTESIAN_POINT('Ctrl Pts',(3.68309250052593,-4.6435828004328,-1.97534977180522));
#40744=CARTESIAN_POINT('Ctrl Pts',(3.71479897811734,-4.09214380238604,-2.78546735077523));
#40745=CARTESIAN_POINT('Ctrl Pts',(3.76783226887223,-3.16978891030818,-4.14049649229039));
#40746=CARTESIAN_POINT('Ctrl Pts',(3.82086555962712,-1.50739523176048,-4.99190325221787));
#40747=CARTESIAN_POINT('Ctrl Pts',(3.87389885038201,0.131231392969287,-4.9484634883131));
#40748=CARTESIAN_POINT('Ctrl Pts',(3.9269321411369,1.76985801769906,-4.90502372440833));
#40749=CARTESIAN_POINT('Ctrl Pts',(3.97996543189179,3.38471758861089,-3.96673743667131));
#40750=CARTESIAN_POINT('Ctrl Pts',(4.03299872264668,4.2339806263878,-2.56470241627798));
#40751=CARTESIAN_POINT('Ctrl Pts',(4.08603201340157,5.0832436641647,-1.16266739588466));
#40752=CARTESIAN_POINT('Ctrl Pts',(4.13906530415646,5.16691016880668,0.703116357164973));
#40753=CARTESIAN_POINT('Ctrl Pts',(4.19209859491135,4.44651837456859,2.17551792657388));
#40754=CARTESIAN_POINT('Ctrl Pts',(4.24513188566624,3.7261265803305,3.64791949598279));
#40755=CARTESIAN_POINT('Ctrl Pts',(4.29816517642112,2.20167648721235,4.72693888175098));
#40756=CARTESIAN_POINT('Ctrl Pts',(4.35119846717601,0.573523415343645,4.91685582765776));
#40757=CARTESIAN_POINT('Ctrl Pts',(4.4042317579309,-1.05462965652506,5.10677277356454));
#40758=CARTESIAN_POINT('Ctrl Pts',(4.45726504868579,-2.78648570714431,4.40758727960991));
#40759=CARTESIAN_POINT('Ctrl Pts',(4.51029833944068,-3.82642545649684,3.14051583547344));
#40760=CARTESIAN_POINT('Ctrl Pts',(4.54675874140815,-4.54138431995091,2.26940386943988));
#40761=CARTESIAN_POINT('Ctrl Pts',(4.58321914337562,-4.92930435769488,1.12987684519085));
#40762=CARTESIAN_POINT('Ctrl Pts',(4.61967954534309,-4.93822978717952,-0.00413487577884502));
#40763=CARTESIAN_POINT('Origin',(8.75,0.,0.));
#40764=CARTESIAN_POINT('',(5.76432045465689,-4.94964305481555,-0.00149822017877888));
#40765=CARTESIAN_POINT('',(5.6196795453431,-4.95001972789837,-0.000833046281679996));
#40766=CARTESIAN_POINT('',(8.75,-4.942,-6.05220448138622E-16));
#40767=CARTESIAN_POINT('Ctrl Pts',(5.76432045465689,-4.94964305481555,-0.00149822017877888));
#40768=CARTESIAN_POINT('Ctrl Pts',(5.71391614856612,-4.94344322054585,1.55689473528395));
#40769=CARTESIAN_POINT('Ctrl Pts',(5.66351184247536,-4.14637927320866,3.12074849239652));
#40770=CARTESIAN_POINT('Ctrl Pts',(5.6131075363846,-2.87904405190479,4.02684576166472));
#40771=CARTESIAN_POINT('Ctrl Pts',(5.56007424562971,-1.54560723890131,4.98020319598355));
#40772=CARTESIAN_POINT('Ctrl Pts',(5.50704095487483,0.308436957536128,5.20540030448662));
#40773=CARTESIAN_POINT('Ctrl Pts',(5.45400766411994,1.83132849201121,4.59898004409288));
#40774=CARTESIAN_POINT('Ctrl Pts',(5.40097437336505,3.35422002648629,3.99255978369913));
#40775=CARTESIAN_POINT('Ctrl Pts',(5.34794108261015,4.54595889899902,2.55452215440856));
#40776=CARTESIAN_POINT('Ctrl Pts',(5.29490779185527,4.8590524110568,0.945511104271855));
#40777=CARTESIAN_POINT('Ctrl Pts',(5.24187450110038,5.17214592311458,-0.663499945864848));
#40778=CARTESIAN_POINT('Ctrl Pts',(5.18884121034549,4.60659407471741,-2.44348441684768));
#40779=CARTESIAN_POINT('Ctrl Pts',(5.1358079195906,3.42221517592476,-3.57670581664182));
#40780=CARTESIAN_POINT('Ctrl Pts',(5.08277462883571,2.23783627713212,-4.70992721643594));
#40781=CARTESIAN_POINT('Ctrl Pts',(5.02974133808082,0.434630327943992,-5.19638554504138));
#40782=CARTESIAN_POINT('Ctrl Pts',(4.97670804732593,-1.15899818313101,-4.81259855606007));
#40783=CARTESIAN_POINT('Ctrl Pts',(4.92367475657104,-2.75262669420602,-4.42881156707877));
#40784=CARTESIAN_POINT('Ctrl Pts',(4.87064146581615,-4.1366777671679,-3.17477926051071));
#40785=CARTESIAN_POINT('Ctrl Pts',(4.81760817506126,-4.67530896281311,-1.62661249453437));
#40786=CARTESIAN_POINT('Ctrl Pts',(4.79984560159314,-4.85571406399927,-1.10808110547425));
#40787=CARTESIAN_POINT('Ctrl Pts',(4.78208302812502,-4.94128014104076,-0.556553774579704));
#40788=CARTESIAN_POINT('Ctrl Pts',(4.76432045465689,-4.93730273339884,-0.00383068200619119));
#40789=CARTESIAN_POINT('Ctrl Pts',(4.61967954534309,-4.93822978717952,-0.00413487577884502));
#40790=CARTESIAN_POINT('Ctrl Pts',(4.63625243413051,-4.94228679539246,-0.519594089641197));
#40791=CARTESIAN_POINT('Ctrl Pts',(4.65282532291793,-4.86803933279054,-1.03391378094767));
#40792=CARTESIAN_POINT('Ctrl Pts',(4.66939821170535,-4.71060802454418,-1.5213680565377));
#40793=CARTESIAN_POINT('Ctrl Pts',(4.72243150246023,-4.20682739515321,-3.08122311009404));
#40794=CARTESIAN_POINT('Ctrl Pts',(4.77546479321513,-2.8512426882855,-4.36597582288839));
#40795=CARTESIAN_POINT('Ctrl Pts',(4.82849808397002,-1.26662024780191,-4.78540071462561));
#40796=CARTESIAN_POINT('Ctrl Pts',(4.88153137472491,0.318002192681684,-5.20482560636284));
#40797=CARTESIAN_POINT('Ctrl Pts',(4.9345646654798,2.13166236678116,-4.7589226770429));
#40798=CARTESIAN_POINT('Ctrl Pts',(4.98759795623469,3.34115384955769,-3.65254352104788));
#40799=CARTESIAN_POINT('Ctrl Pts',(5.04063124698957,4.55064533233423,-2.54616436505285));
#40800=CARTESIAN_POINT('Ctrl Pts',(5.09366453774446,5.15596812378785,-0.77930898238273));
#40801=CARTESIAN_POINT('Ctrl Pts',(5.14669782849935,4.87903246291005,0.83631812290041));
#40802=CARTESIAN_POINT('Ctrl Pts',(5.19973111925424,4.60209680203225,2.45194522818355));
#40803=CARTESIAN_POINT('Ctrl Pts',(5.25276441000913,3.44290268882303,3.91634405607971));
#40804=CARTESIAN_POINT('Ctrl Pts',(5.30579770076402,1.93399176423248,4.55675994305442));
#40805=CARTESIAN_POINT('Ctrl Pts',(5.35883099151891,0.425080839641918,5.19717583002913));
#40806=CARTESIAN_POINT('Ctrl Pts',(5.4118642822738,-1.43354689632998,5.01360877608239));
#40807=CARTESIAN_POINT('Ctrl Pts',(5.46489757302869,-2.78802580404174,4.09039081253591));
#40808=CARTESIAN_POINT('Ctrl Pts',(5.51649156380016,-4.10574475509872,3.19222857494401));
#40809=CARTESIAN_POINT('Ctrl Pts',(5.56808555457163,-4.94630829537066,1.5940182288886));
#40810=CARTESIAN_POINT('Ctrl Pts',(5.6196795453431,-4.95001972789837,-0.000833046281679996));
#40811=CARTESIAN_POINT('Origin',(8.75,0.,0.));
#40812=CARTESIAN_POINT('',(6.76432045465689,-4.94186257797741,0.00456669625063827));
#40813=CARTESIAN_POINT('',(6.6196795453431,-4.9407490012001,0.0045438707638676));
#40814=CARTESIAN_POINT('',(8.75,-4.942,-6.05220448138622E-16));
#40815=CARTESIAN_POINT('Ctrl Pts',(6.76432045465689,-4.94186257797741,0.00456669625063827));
#40816=CARTESIAN_POINT('Ctrl Pts',(6.75181585051702,-4.9454453112525,0.392766622957461));
#40817=CARTESIAN_POINT('Ctrl Pts',(6.73931124637715,-4.903575088203,0.780202475095632));
#40818=CARTESIAN_POINT('Ctrl Pts',(6.72680664223727,-4.81331559170814,1.15601664885576));
#40819=CARTESIAN_POINT('Ctrl Pts',(6.67377335148238,-4.4305159390795,2.74988256607248));
#40820=CARTESIAN_POINT('Ctrl Pts',(6.6207400607275,-3.17734138642797,4.13471006555375));
#40821=CARTESIAN_POINT('Ctrl Pts',(6.56770676997261,-1.62950854494116,4.67430030900523));
#40822=CARTESIAN_POINT('Ctrl Pts',(6.51467347921772,-0.0816757034543591,
5.2138905524567));
#40823=CARTESIAN_POINT('Ctrl Pts',(6.46164018846282,1.76081542686771,4.90824353987838));
#40824=CARTESIAN_POINT('Ctrl Pts',(6.40860689770793,3.05151233350821,3.89777551376765));
#40825=CARTESIAN_POINT('Ctrl Pts',(6.35557360695305,4.34220924014869,2.88730748765693));
#40826=CARTESIAN_POINT('Ctrl Pts',(6.30254031619816,5.08111192310762,1.17201844801381));
#40827=CARTESIAN_POINT('Ctrl Pts',(6.24950702544328,4.9287636414054,-0.460076566630388));
#40828=CARTESIAN_POINT('Ctrl Pts',(6.19647373468839,4.77641535970318,-2.0921715812746));
#40829=CARTESIAN_POINT('Ctrl Pts',(6.14344044393349,3.73281611333981,-3.64107257091991));
#40830=CARTESIAN_POINT('Ctrl Pts',(6.0904071531786,2.2774022442656,-4.39520426037522));
#40831=CARTESIAN_POINT('Ctrl Pts',(6.03737386242371,0.821988375191376,-5.14933594983054));
#40832=CARTESIAN_POINT('Ctrl Pts',(5.98434057166883,-1.04524011659369,-5.10869833909587));
#40833=CARTESIAN_POINT('Ctrl Pts',(5.93130728091394,-2.46646621509766,-4.29196061115554));
#40834=CARTESIAN_POINT('Ctrl Pts',(5.87827399015905,-3.8876923136016,-3.47522288321523));
#40835=CARTESIAN_POINT('Ctrl Pts',(5.82524069940415,-4.86291601882446,-1.88238503806929));
#40836=CARTESIAN_POINT('Ctrl Pts',(5.77220740864926,-4.94411315665113,-0.245207235429026));
#40837=CARTESIAN_POINT('Ctrl Pts',(5.76957842398514,-4.94813828930043,-0.164048490151806));
#40838=CARTESIAN_POINT('Ctrl Pts',(5.76694943932101,-4.94996642538603,-0.0827807830855278));
#40839=CARTESIAN_POINT('Ctrl Pts',(5.76432045465689,-4.94964305481555,-0.00149822017877888));
#40840=CARTESIAN_POINT('Ctrl Pts',(5.6196795453431,-4.95001972789837,-0.000833046281679996));
#40841=CARTESIAN_POINT('Ctrl Pts',(5.62111884532652,-4.95012326446717,-0.0453240689683047));
#40842=CARTESIAN_POINT('Ctrl Pts',(5.62255814530994,-4.94957554297509,-0.0898124775466891));
#40843=CARTESIAN_POINT('Ctrl Pts',(5.62399744529335,-4.94836875446486,-0.134283001160447));
#40844=CARTESIAN_POINT('Ctrl Pts',(5.67703073604824,-4.90390271772459,-1.77286997816412));
#40845=CARTESIAN_POINT('Ctrl Pts',(5.73006402680313,-3.96464056479241,-3.38717505902524));
#40846=CARTESIAN_POINT('Ctrl Pts',(5.78309731755802,-2.5620855277057,-4.23557586562432));
#40847=CARTESIAN_POINT('Ctrl Pts',(5.83613060831291,-1.15953049061901,-5.08397667222339));
#40848=CARTESIAN_POINT('Ctrl Pts',(5.8891638990678,0.706317430622214,-5.16647320456044));
#40849=CARTESIAN_POINT('Ctrl Pts',(5.94219718982269,2.17827547934186,-4.44516603182682));
#40850=CARTESIAN_POINT('Ctrl Pts',(5.99523048057758,3.65023352806152,-3.7238588590932));
#40851=CARTESIAN_POINT('Ctrl Pts',(6.04826377133247,4.72830170425962,-2.19874798128889));
#40852=CARTESIAN_POINT('Ctrl Pts',(6.10129706208736,4.91720840506355,-0.570479332131516));
#40853=CARTESIAN_POINT('Ctrl Pts',(6.15433035284225,5.10611510586748,1.05778931702586));
#40854=CARTESIAN_POINT('Ctrl Pts',(6.20736364359714,4.40586033127725,2.78921573753631));
#40855=CARTESIAN_POINT('Ctrl Pts',(6.26039693435203,3.1381457240098,3.82837126804708));
#40856=CARTESIAN_POINT('Ctrl Pts',(6.31343022510691,1.87043111674235,4.86752679855783));
#40857=CARTESIAN_POINT('Ctrl Pts',(6.3664635158618,0.0352566767976717,5.21441143906891));
#40858=CARTESIAN_POINT('Ctrl Pts',(6.41949680661669,-1.52428642115839,4.70966411245116));
#40859=CARTESIAN_POINT('Ctrl Pts',(6.47253009737158,-3.08382951911445,4.2049167858334));
#40860=CARTESIAN_POINT('Ctrl Pts',(6.52556338812647,-4.3677412750819,2.84853749208683));
#40861=CARTESIAN_POINT('Ctrl Pts',(6.57859667888136,-4.78618420382354,1.26365577601926));
#40862=CARTESIAN_POINT('Ctrl Pts',(6.59229096770194,-4.89423479317131,0.854406648587289));
#40863=CARTESIAN_POINT('Ctrl Pts',(6.60598525652252,-4.94457775183742,0.429921462983896));
#40864=CARTESIAN_POINT('Ctrl Pts',(6.6196795453431,-4.9407490012001,0.0045438707638676));
#40865=CARTESIAN_POINT('Origin',(8.75,0.,0.));
#40866=CARTESIAN_POINT('',(7.76432045465689,-4.93388715137377,-0.000577480970858357));
#40867=CARTESIAN_POINT('',(7.6196795453431,-4.93408355834929,-0.0011800419470579));
#40868=CARTESIAN_POINT('',(8.75,-4.942,-6.05220448138622E-16));
#40869=CARTESIAN_POINT('Ctrl Pts',(7.76432045465689,-4.93388715137377,-0.000577480970858357));
#40870=CARTESIAN_POINT('Ctrl Pts',(7.73668226171302,-4.93299226451753,0.860940067097838));
#40871=CARTESIAN_POINT('Ctrl Pts',(7.70904406876916,-4.71867004547136,1.72287425155414));
#40872=CARTESIAN_POINT('Ctrl Pts',(7.68140587582529,-4.29348773831838,2.46380691579945));
#40873=CARTESIAN_POINT('Ctrl Pts',(7.6283725850704,-3.4776306030537,3.88553870168424));
#40874=CARTESIAN_POINT('Ctrl Pts',(7.57533929431551,-1.88539720710199,4.86174896359399));
#40875=CARTESIAN_POINT('Ctrl Pts',(7.52230600356062,-0.248270018437432,
4.94396030276934));
#40876=CARTESIAN_POINT('Ctrl Pts',(7.46927271280573,1.38885717022713,5.02617164194469));
#40877=CARTESIAN_POINT('Ctrl Pts',(7.41623942205083,3.07087815160453,4.21438405838564));
#40878=CARTESIAN_POINT('Ctrl Pts',(7.36320613129594,4.02506145193688,2.88153809371726));
#40879=CARTESIAN_POINT('Ctrl Pts',(7.31017284054106,4.97924475226923,1.54869212904887));
#40880=CARTESIAN_POINT('Ctrl Pts',(7.25713954978617,5.20559037155652,-0.305212216728855));
#40881=CARTESIAN_POINT('Ctrl Pts',(7.20410625903128,4.60011364733754,-1.8284791245895));
#40882=CARTESIAN_POINT('Ctrl Pts',(7.15107296827639,3.99463692311855,-3.35174603245014));
#40883=CARTESIAN_POINT('Ctrl Pts',(7.0980396775215,2.55733785539328,-4.5443755023937));
#40884=CARTESIAN_POINT('Ctrl Pts',(7.04500638676661,0.948521065327934,-4.85846573168681));
#40885=CARTESIAN_POINT('Ctrl Pts',(6.99197309601172,-0.6602957247374,-5.17255596097992));
#40886=CARTESIAN_POINT('Ctrl Pts',(6.93893980525684,-2.44063023714281,-4.60810694962259));
#40887=CARTESIAN_POINT('Ctrl Pts',(6.88590651450195,-3.57458511704265,-3.42443027646787));
#40888=CARTESIAN_POINT('Ctrl Pts',(6.84537782788693,-4.44116724515231,-2.5198501484589));
#40889=CARTESIAN_POINT('Ctrl Pts',(6.80484914127191,-4.930250577109,-1.25362852508438));
#40890=CARTESIAN_POINT('Ctrl Pts',(6.76432045465689,-4.94186257797741,0.00456669625063827));
#40891=CARTESIAN_POINT('Ctrl Pts',(6.6196795453431,-4.9407490012001,0.0045438707638676));
#40892=CARTESIAN_POINT('Ctrl Pts',(6.65901854727741,-4.92975031184129,-1.21742027373473));
#40893=CARTESIAN_POINT('Ctrl Pts',(6.69835754921173,-4.47171793942916,-2.44674870157877));
#40894=CARTESIAN_POINT('Ctrl Pts',(6.73769655114603,-3.65047313959733,-3.34341606856897));
#40895=CARTESIAN_POINT('Ctrl Pts',(6.79072984190092,-2.54334504511365,-4.55222205870107));
#40896=CARTESIAN_POINT('Ctrl Pts',(6.8437631326558,-0.776114754630469,-5.15644990057672));
#40897=CARTESIAN_POINT('Ctrl Pts',(6.89679642341069,0.839340542852879,-4.87851335994245));
#40898=CARTESIAN_POINT('Ctrl Pts',(6.94982971416558,2.45479584033622,-4.60057681930817));
#40899=CARTESIAN_POINT('Ctrl Pts',(7.00286300492048,3.91847614481972,-3.44047589616397));
#40900=CARTESIAN_POINT('Ctrl Pts',(7.05589629567537,4.5579571217266,-1.93116856527833));
#40901=CARTESIAN_POINT('Ctrl Pts',(7.10892958643026,5.19743809863347,-0.421861234392705));
#40902=CARTESIAN_POINT('Ctrl Pts',(7.16196287718514,5.01271974796372,1.43665250423437));
#40903=CARTESIAN_POINT('Ctrl Pts',(7.21499616794003,4.08866289196774,2.79055924617738));
#40904=CARTESIAN_POINT('Ctrl Pts',(7.26802945869492,3.16460603597175,4.1444659881204));
#40905=CARTESIAN_POINT('Ctrl Pts',(7.32106274944981,1.50121067464953,4.99376573337936));
#40906=CARTESIAN_POINT('Ctrl Pts',(7.3740960402047,-0.137348450334091,4.94828460718909));
#40907=CARTESIAN_POINT('Ctrl Pts',(7.42712933095959,-1.77590757531773,4.90280348099881));
#40908=CARTESIAN_POINT('Ctrl Pts',(7.48016262171448,-3.38963046396277,3.96254148335925));
#40909=CARTESIAN_POINT('Ctrl Pts',(7.53319591246937,-4.23716223434557,2.5594611445621));
#40910=CARTESIAN_POINT('Ctrl Pts',(7.56202379009394,-4.69786421628478,1.79677363774235));
#40911=CARTESIAN_POINT('Ctrl Pts',(7.59085166771852,-4.93217199616782,0.89733253701383));
#40912=CARTESIAN_POINT('Ctrl Pts',(7.6196795453431,-4.93408355834929,-0.0011800419470579));
#40913=CARTESIAN_POINT('Origin',(8.75,0.,0.));
#40914=CARTESIAN_POINT('',(8.76432045465689,-4.94398902458143,-0.00436563055240979));
#40915=CARTESIAN_POINT('',(8.6196795453431,-4.94509229898035,-0.00412964409767292));
#40916=CARTESIAN_POINT('',(8.75,-4.942,-6.05220448138622E-16));
#40917=CARTESIAN_POINT('Ctrl Pts',(8.76432045465689,-4.94398902458143,-0.00436563055240979));
#40918=CARTESIAN_POINT('Ctrl Pts',(8.72154867290902,-4.93175999696903,1.32200133659815));
#40919=CARTESIAN_POINT('Ctrl Pts',(8.67877689116116,-4.38072220103998,2.65732794935703));
#40920=CARTESIAN_POINT('Ctrl Pts',(8.63600510941329,-3.42664403930687,3.5724630306423));
#40921=CARTESIAN_POINT('Ctrl Pts',(8.5829718186584,-2.24367006706628,4.70715096886972));
#40922=CARTESIAN_POINT('Ctrl Pts',(8.52993852790351,-0.441068126124786,
5.1958430039501));
#40923=CARTESIAN_POINT('Ctrl Pts',(8.47690523714862,1.15303462585385,4.81403080889657));
#40924=CARTESIAN_POINT('Ctrl Pts',(8.42387194639373,2.74713737783251,4.43221861384304));
#40925=CARTESIAN_POINT('Ctrl Pts',(8.37083865563885,4.13274094084831,3.17990218865558));
#40926=CARTESIAN_POINT('Ctrl Pts',(8.31780536488396,4.67328994778057,1.63240391490459));
#40927=CARTESIAN_POINT('Ctrl Pts',(8.26477207412907,5.21383895471282,0.0849056411536261));
#40928=CARTESIAN_POINT('Ctrl Pts',(8.21173878337417,4.90933340556155,-1.75777448116088));
#40929=CARTESIAN_POINT('Ctrl Pts',(8.15870549261928,3.89966514731939,-3.04909711491891));
#40930=CARTESIAN_POINT('Ctrl Pts',(8.10567220186439,2.88999688907721,-4.34041974867696));
#40931=CARTESIAN_POINT('Ctrl Pts',(8.05263891110951,1.17516592174414,-5.0803848938785));
#40932=CARTESIAN_POINT('Ctrl Pts',(7.99960562035462,-0.457023158113981,
-4.92904770826675));
#40933=CARTESIAN_POINT('Ctrl Pts',(7.94657232959973,-2.08921223797207,-4.77771052265501));
#40934=CARTESIAN_POINT('Ctrl Pts',(7.89353903884484,-3.6387594303552,-3.73507100623));
#40935=CARTESIAN_POINT('Ctrl Pts',(7.84050574808995,-4.39379258925795,-2.28012459308761));
#40936=CARTESIAN_POINT('Ctrl Pts',(7.81511065027893,-4.75534173410583,-1.58342058046442));
#40937=CARTESIAN_POINT('Ctrl Pts',(7.78971555246791,-4.93470940987996,-0.792174907168253));
#40938=CARTESIAN_POINT('Ctrl Pts',(7.76432045465689,-4.93388715137377,-0.000577480970858357));
#40939=CARTESIAN_POINT('Ctrl Pts',(7.6196795453431,-4.93408355834929,-0.0011800419470579));
#40940=CARTESIAN_POINT('Ctrl Pts',(7.64388495847341,-4.93568860721656,-0.755618799449938));
#40941=CARTESIAN_POINT('Ctrl Pts',(7.66809037160372,-4.77345034543105,-1.50940293321614));
#40942=CARTESIAN_POINT('Ctrl Pts',(7.69229578473404,-4.44381576150152,-2.18102880046318));
#40943=CARTESIAN_POINT('Ctrl Pts',(7.74532907548893,-3.72159686615413,-3.6525397267366));
#40944=CARTESIAN_POINT('Ctrl Pts',(7.79836236624381,-2.19581842333879,-4.72966289932871));
#40945=CARTESIAN_POINT('Ctrl Pts',(7.8513956569987,-0.567433059567756,-4.91756086627617));
#40946=CARTESIAN_POINT('Ctrl Pts',(7.90442894775359,1.06095230420328,-5.10545883322364));
#40947=CARTESIAN_POINT('Ctrl Pts',(7.95746223850848,2.79194458893001,-4.40413159452647));
#40948=CARTESIAN_POINT('Ctrl Pts',(8.01049552926337,3.83031458280598,-3.13577348470557));
#40949=CARTESIAN_POINT('Ctrl Pts',(8.06352882001826,4.86868457668194,-1.86741537488468));
#40950=CARTESIAN_POINT('Ctrl Pts',(8.11656211077315,5.21443227970714,-0.0320263939400439));
#40951=CARTESIAN_POINT('Ctrl Pts',(8.16959540152804,4.7087189288313,1.52720371918551));
#40952=CARTESIAN_POINT('Ctrl Pts',(8.22262869228293,4.20300557795547,3.08643383231107));
#40953=CARTESIAN_POINT('Ctrl Pts',(8.27566198303782,2.84583117317862,4.36950507761757));
#40954=CARTESIAN_POINT('Ctrl Pts',(8.32869527379271,1.26069053981566,4.78696610740548));
#40955=CARTESIAN_POINT('Ctrl Pts',(8.3817285645476,-0.324450093547317,5.20442713719338));
#40956=CARTESIAN_POINT('Ctrl Pts',(8.43476185530248,-2.1375569554964,4.75627795146268));
#40957=CARTESIAN_POINT('Ctrl Pts',(8.48779514605737,-3.34567685873883,3.6484012262265));
#40958=CARTESIAN_POINT('Ctrl Pts',(8.53175661248595,-4.34713691924224,2.73003684094686));
#40959=CARTESIAN_POINT('Ctrl Pts',(8.57571807891452,-4.93288436617281,1.35834522977113));
#40960=CARTESIAN_POINT('Ctrl Pts',(8.6196795453431,-4.94509229898035,-0.00412964409767292));
#40961=CARTESIAN_POINT('Origin',(8.75,0.,0.));
#40962=CARTESIAN_POINT('',(9.76432045465689,-4.94845593707282,0.00263657310841547));
#40963=CARTESIAN_POINT('',(9.6196795453431,-4.94762324771633,0.00315517675713146));
#40964=CARTESIAN_POINT('',(8.75,-4.942,-6.05220448138622E-16));
#40965=CARTESIAN_POINT('Ctrl Pts',(9.76432045465689,-4.94845593707282,0.00263657310841547));
#40966=CARTESIAN_POINT('Ctrl Pts',(9.75944837485992,-4.94942745139196,0.153366619893802));
#40967=CARTESIAN_POINT('Ctrl Pts',(9.75457629506294,-4.94314008508034,0.304014507117773));
#40968=CARTESIAN_POINT('Ctrl Pts',(9.74970421526596,-4.92932988376321,0.453969574366955));
#40969=CARTESIAN_POINT('Ctrl Pts',(9.69667092451108,-4.77900385209818,2.08625209291875));
#40970=CARTESIAN_POINT('Ctrl Pts',(9.64363763375619,-3.73732446482242,3.63644489277922));
#40971=CARTESIAN_POINT('Ctrl Pts',(9.5906043430013,-2.28284606639771,4.39237923164047));
#40972=CARTESIAN_POINT('Ctrl Pts',(9.53757105224641,-0.828367667972992,
5.14831357050172));
#40973=CARTESIAN_POINT('Ctrl Pts',(9.48453776149151,1.03890974160068,5.10998944836375));
#40974=CARTESIAN_POINT('Ctrl Pts',(9.43150447073663,2.46114667006327,4.29501321835778));
#40975=CARTESIAN_POINT('Ctrl Pts',(9.37847117998174,3.88338359852585,3.4800369883518));
#40976=CARTESIAN_POINT('Ctrl Pts',(9.32543788922685,4.86058004587734,1.88840865047781));
#40977=CARTESIAN_POINT('Ctrl Pts',(9.27240459847196,4.9438055532949,0.251332705057519));
#40978=CARTESIAN_POINT('Ctrl Pts',(9.21937130771707,5.02703106071247,-1.38574324036278));
#40979=CARTESIAN_POINT('Ctrl Pts',(9.16633801696218,4.2162856281961,-3.06826679332938));
#40980=CARTESIAN_POINT('Ctrl Pts',(9.11330472620729,2.88403102634981,-4.02327559539163));
#40981=CARTESIAN_POINT('Ctrl Pts',(9.0602714354524,1.55177642450353,-4.97828439745387));
#40982=CARTESIAN_POINT('Ctrl Pts',(9.00723814469752,-0.301987346672683,
-5.20577844861174));
#40983=CARTESIAN_POINT('Ctrl Pts',(8.95420485394263,-1.82562904905711,-4.60124548928475));
#40984=CARTESIAN_POINT('Ctrl Pts',(8.90117156318774,-3.34927075144153,-3.99671252995776));
#40985=CARTESIAN_POINT('Ctrl Pts',(8.84813827243285,-4.54279038503418,-2.56015256014591));
#40986=CARTESIAN_POINT('Ctrl Pts',(8.79510498167796,-4.85787720006066,-0.951530654552757));
#40987=CARTESIAN_POINT('Ctrl Pts',(8.78484347267093,-4.91884392764563,-0.640275442247928));
#40988=CARTESIAN_POINT('Ctrl Pts',(8.77458196366391,-4.94692292800709,-0.322578387277471));
#40989=CARTESIAN_POINT('Ctrl Pts',(8.76432045465689,-4.94398902458143,-0.00436563055240979));
#40990=CARTESIAN_POINT('Ctrl Pts',(8.6196795453431,-4.94509229898035,-0.00412964409767292));
#40991=CARTESIAN_POINT('Ctrl Pts',(8.62875136966941,-4.94761151025364,-0.285287979087153));
#40992=CARTESIAN_POINT('Ctrl Pts',(8.63782319399572,-4.92570720098754,-0.566053829919258));
#40993=CARTESIAN_POINT('Ctrl Pts',(8.64689501832204,-4.87799246076471,-0.842362572383541));
#40994=CARTESIAN_POINT('Ctrl Pts',(8.69992830907693,-4.59905521501237,-2.45764538101576));
#40995=CARTESIAN_POINT('Ctrl Pts',(8.75296159983182,-3.43804777897189,-3.92060673353855));
#40996=CARTESIAN_POINT('Ctrl Pts',(8.80599489058671,-1.9283445855655,-4.55915258682474));
#40997=CARTESIAN_POINT('Ctrl Pts',(8.8590281813416,-0.418641392159106,-5.19769844011094));
#40998=CARTESIAN_POINT('Ctrl Pts',(8.91206147209648,1.4397575586132,-5.01182879416055));
#40999=CARTESIAN_POINT('Ctrl Pts',(8.96509476285137,2.79309159671432,-4.08693338372359));
#41000=CARTESIAN_POINT('Ctrl Pts',(9.01812805360626,4.14642563481545,-3.16203797328663));
#41001=CARTESIAN_POINT('Ctrl Pts',(9.07116134436116,4.9946947602454,-1.4981167983631));
#41002=CARTESIAN_POINT('Ctrl Pts',(9.12419463511605,4.94819857170044,0.140413837109267));
#41003=CARTESIAN_POINT('Ctrl Pts',(9.17722792587094,4.90170238315548,1.77894447258163));
#41004=CARTESIAN_POINT('Ctrl Pts',(9.23026121662582,3.96044088063561,3.39208456860284));
#41005=CARTESIAN_POINT('Ctrl Pts',(9.28329450738071,2.55683577355735,4.23874698203242));
#41006=CARTESIAN_POINT('Ctrl Pts',(9.3363277981356,1.15323066647911,5.085409395462));
#41007=CARTESIAN_POINT('Ctrl Pts',(9.38936108889049,-0.712718045157501,
5.16559412629996));
#41008=CARTESIAN_POINT('Ctrl Pts',(9.44239437964538,-2.18378128164371,4.44246378314692));
#41009=CARTESIAN_POINT('Ctrl Pts',(9.49542767040027,-3.65484451812992,3.71933343999387));
#41010=CARTESIAN_POINT('Ctrl Pts',(9.54846096115516,-4.73102227946572,2.19288802284981));
#41011=CARTESIAN_POINT('Ctrl Pts',(9.60149425191005,-4.91791144181518,0.564386570615904));
#41012=CARTESIAN_POINT('Ctrl Pts',(9.60755601638773,-4.93927308220122,0.378247032327898));
#41013=CARTESIAN_POINT('Ctrl Pts',(9.61361778086541,-4.94901639309396,0.190774157883547));
#41014=CARTESIAN_POINT('Ctrl Pts',(9.6196795453431,-4.94762324771633,0.00315517675713146));
#41015=CARTESIAN_POINT('Origin',(8.75,0.,0.));
#41016=CARTESIAN_POINT('',(10.7643204546569,-4.93580407701378,0.00307338633379534));
#41017=CARTESIAN_POINT('',(10.6196795453431,-4.93516283533062,0.00258890295936728));
#41018=CARTESIAN_POINT('',(8.75,-4.942,-6.05220448138622E-16));
#41019=CARTESIAN_POINT('Ctrl Pts',(10.7643204546569,-4.93580407701378,0.00307338633379534));
#41020=CARTESIAN_POINT('Ctrl Pts',(10.7443147860559,-4.93932984348302,0.626070349929172));
#41021=CARTESIAN_POINT('Ctrl Pts',(10.7243091174549,-4.83006652292542,1.24787603993653));
#41022=CARTESIAN_POINT('Ctrl Pts',(10.704303448854,-4.60237556535654,1.82277827304598));
#41023=CARTESIAN_POINT('Ctrl Pts',(10.6512701580991,-3.99878660285512,3.34679418534805));
#41024=CARTESIAN_POINT('Ctrl Pts',(10.5982368673442,-2.56296628237974,4.54120352427818));
#41025=CARTESIAN_POINT('Ctrl Pts',(10.5452035765893,-0.954539878637368,
4.85728680405981));
#41026=CARTESIAN_POINT('Ctrl Pts',(10.4921702858344,0.653886525104984,5.17337008384144));
#41027=CARTESIAN_POINT('Ctrl Pts',(10.4391369950795,2.43491901211431,4.61112730447459));
#41028=CARTESIAN_POINT('Ctrl Pts',(10.3861037043246,3.57033957324573,3.42885648715834));
#41029=CARTESIAN_POINT('Ctrl Pts',(10.3330704135697,4.70576013437717,2.24658566984208));
#41030=CARTESIAN_POINT('Ctrl Pts',(10.2800371228148,5.19556876963067,0.444286814576416));
#41031=CARTESIAN_POINT('Ctrl Pts',(10.22700383206,4.81474417863934,-1.15005216039585));
#41032=CARTESIAN_POINT('Ctrl Pts',(10.1739705413051,4.43391958764801,-2.74439113536811));
#41033=CARTESIAN_POINT('Ctrl Pts',(10.1209372505502,3.18246177041184,-4.130770230047));
#41034=CARTESIAN_POINT('Ctrl Pts',(10.0679039597953,1.63529865834168,-4.67227779304397));
#41035=CARTESIAN_POINT('Ctrl Pts',(10.0148706690404,0.0881355462715097,
-5.21378535604094));
#41036=CARTESIAN_POINT('Ctrl Pts',(9.96183737828552,-1.75473286063265,-4.910421387356));
#41037=CARTESIAN_POINT('Ctrl Pts',(9.90880408753063,-3.04668072605759,-3.90155328439197));
#41038=CARTESIAN_POINT('Ctrl Pts',(9.86064287657272,-4.21993950007811,-2.98536820811364));
#41039=CARTESIAN_POINT('Ctrl Pts',(9.8124816656148,-4.93885237801332,-1.48735166259974));
#41040=CARTESIAN_POINT('Ctrl Pts',(9.76432045465689,-4.94845593707282,0.00263657310841547));
#41041=CARTESIAN_POINT('Ctrl Pts',(9.6196795453431,-4.94762324771633,0.00315517675713146));
#41042=CARTESIAN_POINT('Ctrl Pts',(9.6666510716203,-4.93682801392686,-1.45067067453174));
#41043=CARTESIAN_POINT('Ctrl Pts',(9.7136225978975,-4.25735291877213,-2.91326938798931));
#41044=CARTESIAN_POINT('Ctrl Pts',(9.76059412417471,-3.13340004119507,-3.83225642833011));
#41045=CARTESIAN_POINT('Ctrl Pts',(9.8136274149296,-1.86439891486239,-4.86984048771844));
#41046=CARTESIAN_POINT('Ctrl Pts',(9.8666607056845,-0.0287960988339278,
-5.21445111917136));
#41047=CARTESIAN_POINT('Ctrl Pts',(9.91969399643938,1.53012043070582,-4.70777193778096));
#41048=CARTESIAN_POINT('Ctrl Pts',(9.97272728719427,3.08903696024558,-4.20109275639056));
#41049=CARTESIAN_POINT('Ctrl Pts',(10.0257605779492,4.37126720329662,-2.84312376215679));
#41050=CARTESIAN_POINT('Ctrl Pts',(10.078793868704,4.78774617411819,-1.25772481999673));
#41051=CARTESIAN_POINT('Ctrl Pts',(10.1318271594589,5.20422514493976,0.32767412216334));
#41052=CARTESIAN_POINT('Ctrl Pts',(10.1848604502138,4.75495284353188,2.14050301224973));
#41053=CARTESIAN_POINT('Ctrl Pts',(10.2378937409687,3.64632791260652,3.34793636505146));
#41054=CARTESIAN_POINT('Ctrl Pts',(10.2909270317236,2.53770298168117,4.55536971785319));
#41055=CARTESIAN_POINT('Ctrl Pts',(10.3439603224785,0.769725421238379,5.15740753337025));
#41056=CARTESIAN_POINT('Ctrl Pts',(10.3969936132334,-0.845384278590161,
4.87746968950768));
#41057=CARTESIAN_POINT('Ctrl Pts',(10.4500269039883,-2.4604939784187,4.59753184564511));
#41058=CARTESIAN_POINT('Ctrl Pts',(10.5030601947432,-3.92273581763298,3.43561834240286));
#41059=CARTESIAN_POINT('Ctrl Pts',(10.5560934854981,-4.56034630228406,1.92551986586069));
#41060=CARTESIAN_POINT('Ctrl Pts',(10.5772888387797,-4.81517452972229,1.32199196395519));
#41061=CARTESIAN_POINT('Ctrl Pts',(10.5984841920614,-4.93828509595529,0.662848773962371));
#41062=CARTESIAN_POINT('Ctrl Pts',(10.6196795453431,-4.93516283533062,0.00258890295936728));
#41063=CARTESIAN_POINT('Origin',(8.75,0.,0.));
#41064=CARTESIAN_POINT('',(11.7643204546569,-4.93720552711113,-0.00379265621960889));
#41065=CARTESIAN_POINT('',(11.6196795453431,-4.9381236876051,-0.00410472656473214));
#41066=CARTESIAN_POINT('',(8.75,-4.942,-6.05220448138622E-16));
#41067=CARTESIAN_POINT('Ctrl Pts',(11.7643204546569,-4.93720552711113,-0.00379265621960889));
#41068=CARTESIAN_POINT('Ctrl Pts',(11.7291811972519,-4.92942537133172,1.08969997146474));
#41069=CARTESIAN_POINT('Ctrl Pts',(11.694041939847,-4.57137406349285,2.18781921440517));
#41070=CARTESIAN_POINT('Ctrl Pts',(11.658902682442,-3.90343992071078,3.04426317473012));
#41071=CARTESIAN_POINT('Ctrl Pts',(11.6058693916871,-2.89537235710122,4.33683578204868));
#41072=CARTESIAN_POINT('Ctrl Pts',(11.5528361009322,-1.1814595146183,5.07892498719433));
#41073=CARTESIAN_POINT('Ctrl Pts',(11.4998028101773,0.450915814594913,4.92961016401842));
#41074=CARTESIAN_POINT('Ctrl Pts',(11.4467695194224,2.08329114380809,4.78029534084251));
#41075=CARTESIAN_POINT('Ctrl Pts',(11.3937362286675,3.63412895975154,3.73957648934505));
#41076=CARTESIAN_POINT('Ctrl Pts',(11.3407029379126,4.39096418931034,2.28556666546216));
#41077=CARTESIAN_POINT('Ctrl Pts',(11.2876696471578,5.14779941886913,0.83155684157926));
#41078=CARTESIAN_POINT('Ctrl Pts',(11.2346363564029,5.11063206204329,-1.03574395468909));
#41079=CARTESIAN_POINT('Ctrl Pts',(11.181603065648,4.29653704961789,-2.45848548077665));
#41080=CARTESIAN_POINT('Ctrl Pts',(11.1285697748931,3.4824420371925,-3.88122700686422));
#41081=CARTESIAN_POINT('Ctrl Pts',(11.0755364841382,1.89141936916755,-4.85940926277102));
#41082=CARTESIAN_POINT('Ctrl Pts',(11.0225031933833,0.254395295479178,-4.94364890604547));
#41083=CARTESIAN_POINT('Ctrl Pts',(10.9694699026284,-1.38262877820921,-5.02788854931992));
#41084=CARTESIAN_POINT('Ctrl Pts',(10.9164366118735,-3.06565425756101,-4.21818557996203));
#41085=CARTESIAN_POINT('Ctrl Pts',(10.8634033211186,-4.0214881949732,-2.88652285244607));
#41086=CARTESIAN_POINT('Ctrl Pts',(10.8303756989647,-4.6167543320991,-2.05720125510973));
#41087=CARTESIAN_POINT('Ctrl Pts',(10.7973480768108,-4.92998334264735,-1.0254405177534));
#41088=CARTESIAN_POINT('Ctrl Pts',(10.7643204546569,-4.93580407701378,0.00307338633379534));
#41089=CARTESIAN_POINT('Ctrl Pts',(10.6196795453431,-4.93516283533062,0.00258890295936728));
#41090=CARTESIAN_POINT('Ctrl Pts',(10.6515174828163,-4.93047282911924,-0.989199825904508));
#41091=CARTESIAN_POINT('Ctrl Pts',(10.6833554202895,-4.64095603026269,-1.98350818994138));
#41092=CARTESIAN_POINT('Ctrl Pts',(10.7151933577627,-4.08520230705393,-2.7956228753998));
#41093=CARTESIAN_POINT('Ctrl Pts',(10.7682266485176,-3.15946869708483,-4.14838369027595));
#41094=CARTESIAN_POINT('Ctrl Pts',(10.8212599392725,-1.49502234705878,-4.99562187018618));
#41095=CARTESIAN_POINT('Ctrl Pts',(10.8742932300274,0.143479170036918,-4.94811063718052));
#41096=CARTESIAN_POINT('Ctrl Pts',(10.9273265207823,1.78198068713267,-4.90059940417486));
#41097=CARTESIAN_POINT('Ctrl Pts',(10.9803598115372,3.39453737129806,-3.95833875825322));
#41098=CARTESIAN_POINT('Ctrl Pts',(11.0333931022921,4.24033010293758,-2.55420942144691));
#41099=CARTESIAN_POINT('Ctrl Pts',(11.0864263930469,5.08612283457709,-1.1500800846406));
#41100=CARTESIAN_POINT('Ctrl Pts',(11.1394596838018,5.16515161369075,0.715917943050361));
#41101=CARTESIAN_POINT('Ctrl Pts',(11.1924929745567,4.44111010008868,2.18653292499499));
#41102=CARTESIAN_POINT('Ctrl Pts',(11.2455262653116,3.71706858648663,3.6571479069396));
#41103=CARTESIAN_POINT('Ctrl Pts',(11.2985595560665,2.18995678016881,4.73237984313789));
#41104=CARTESIAN_POINT('Ctrl Pts',(11.3515928468214,0.561339864738128,4.91826012956756));
#41105=CARTESIAN_POINT('Ctrl Pts',(11.4046261375763,-1.06727705069257,5.10414041599724));
#41106=CARTESIAN_POINT('Ctrl Pts',(11.4576594283312,-2.79739907523614,4.40066905265832));
#41107=CARTESIAN_POINT('Ctrl Pts',(11.5106927190861,-3.83419680251794,3.13102539604688));
#41108=CARTESIAN_POINT('Ctrl Pts',(11.5470216611717,-4.54442549194757,2.26129224892483));
#41109=CARTESIAN_POINT('Ctrl Pts',(11.5833506032574,-4.92930870695169,1.12588026422444));
#41110=CARTESIAN_POINT('Ctrl Pts',(11.6196795453431,-4.9381236876051,-0.00410472656473213));
#41111=CARTESIAN_POINT('Origin',(8.75,0.,0.));
#41112=CARTESIAN_POINT('',(12.7643204546569,-4.949590084061,-0.00157034721157134));
#41113=CARTESIAN_POINT('',(12.6196795453431,-4.94998806776073,-0.000908059682992989));
#41114=CARTESIAN_POINT('',(8.75,-4.942,-6.05220448138622E-16));
#41115=CARTESIAN_POINT('Ctrl Pts',(12.7643204546569,-4.949590084061,-0.00157034721157134));
#41116=CARTESIAN_POINT('Ctrl Pts',(12.7140476084479,-4.94314587879761,1.55280243246766));
#41117=CARTESIAN_POINT('Ctrl Pts',(12.663774762239,-4.15080012520513,3.11283579625446));
#41118=CARTESIAN_POINT('Ctrl Pts',(12.61350191603,-2.8890133989013,4.01969958641386));
#41119=CARTESIAN_POINT('Ctrl Pts',(12.5604686252751,-1.55794290313953,4.9763585919273));
#41120=CARTESIAN_POINT('Ctrl Pts',(12.5074353345202,0.295537250634443,5.20614859064765));
#41121=CARTESIAN_POINT('Ctrl Pts',(12.4544020437653,1.8199267078499,4.60350370034535));
#41122=CARTESIAN_POINT('Ctrl Pts',(12.4013687530104,3.34431616506535,4.00085881004305));
#41123=CARTESIAN_POINT('Ctrl Pts',(12.3483354622555,4.53961492572229,2.56577903071809));
#41124=CARTESIAN_POINT('Ctrl Pts',(12.2953021715007,4.8566945907577,0.957548827601382));
#41125=CARTESIAN_POINT('Ctrl Pts',(12.2422688807458,5.17377425579312,-0.650681375515335));
#41126=CARTESIAN_POINT('Ctrl Pts',(12.1892355899909,4.61263482520701,-2.43206200242381));
#41127=CARTESIAN_POINT('Ctrl Pts',(12.136202299236,3.43106759472794,-3.56821479324049));
#41128=CARTESIAN_POINT('Ctrl Pts',(12.0831690084811,2.24950036424889,-4.70436758405716));
#41129=CARTESIAN_POINT('Ctrl Pts',(12.0301357177262,0.447505333876852,-5.19529253878204));
#41130=CARTESIAN_POINT('Ctrl Pts',(11.9771024269713,-1.14706924085875,-4.81545567582185));
#41131=CARTESIAN_POINT('Ctrl Pts',(11.9240691362164,-2.74164381559436,-4.43561881286166));
#41132=CARTESIAN_POINT('Ctrl Pts',(11.8710358454615,-4.12879793469354,-3.1850201322164));
#41133=CARTESIAN_POINT('Ctrl Pts',(11.8180025547066,-4.67126385187503,-1.63819278714807));
#41134=CARTESIAN_POINT('Ctrl Pts',(11.8001085213567,-4.85429800033287,-1.11627571005884));
#41135=CARTESIAN_POINT('Ctrl Pts',(11.7822144880068,-4.94116743118268,-0.560634063599559));
#41136=CARTESIAN_POINT('Ctrl Pts',(11.7643204546569,-4.93720552711113,-0.00379265621960889));
#41137=CARTESIAN_POINT('Ctrl Pts',(11.6196795453431,-4.9381236876051,-0.00410472656473213));
#41138=CARTESIAN_POINT('Ctrl Pts',(11.6363838940123,-4.94217688876905,-0.523681190767773));
#41139=CARTESIAN_POINT('Ctrl Pts',(11.6530882426815,-4.86672036673493,-1.04211026004547));
#41140=CARTESIAN_POINT('Ctrl Pts',(11.6697925913507,-4.70682314126475,-1.53303655666506));
#41141=CARTESIAN_POINT('Ctrl Pts',(11.7228258821056,-4.19917832270976,-3.09163890288159));
#41142=CARTESIAN_POINT('Ctrl Pts',(11.7758591728605,-2.84041525557975,-4.3730276454307));
#41143=CARTESIAN_POINT('Ctrl Pts',(11.8288924636154,-1.2547586151515,-4.78852440028367));
#41144=CARTESIAN_POINT('Ctrl Pts',(11.8819257543703,0.330898025276773,-5.20402115513665));
#41145=CARTESIAN_POINT('Ctrl Pts',(11.9349590451252,2.14344823900332,-4.75362592229347));
#41146=CARTESIAN_POINT('Ctrl Pts',(11.9879923358801,3.35019458202354,-3.64425320570872));
#41147=CARTESIAN_POINT('Ctrl Pts',(12.041025626635,4.55694092504374,-2.53488048912399));
#41148=CARTESIAN_POINT('Ctrl Pts',(12.0940589173898,5.15788339735766,-0.76653028879776));
#41149=CARTESIAN_POINT('Ctrl Pts',(12.1470922081447,4.87694505508189,0.848405671997188));
#41150=CARTESIAN_POINT('Ctrl Pts',(12.2001254988996,4.59600671280612,2.46334163279215));
#41151=CARTESIAN_POINT('Ctrl Pts',(12.2531587896545,3.43318755594063,3.9248633540558));
#41152=CARTESIAN_POINT('Ctrl Pts',(12.3061920804094,1.92269439062044,4.56153824532443));
#41153=CARTESIAN_POINT('Ctrl Pts',(12.3592253711643,0.412201225300242,5.19821313659306));
#41154=CARTESIAN_POINT('Ctrl Pts',(12.4122586619192,-1.44596594847468,5.01004119786668));
#41155=CARTESIAN_POINT('Ctrl Pts',(12.4652919526741,-2.79815304941714,4.08346970538315));
#41156=CARTESIAN_POINT('Ctrl Pts',(12.5167544835637,-4.11029056644383,3.18434175434171));
#41157=CARTESIAN_POINT('Ctrl Pts',(12.5682170144534,-4.94597675512516,1.58990687892319));
#41158=CARTESIAN_POINT('Ctrl Pts',(12.6196795453431,-4.94998806776073,-0.000908059682992989));
#41159=CARTESIAN_POINT('Origin',(8.75,0.,0.));
#41160=CARTESIAN_POINT('',(13.7643204546569,-4.94198723275246,0.00456325735460533));
#41161=CARTESIAN_POINT('',(13.6196795453431,-4.94087041225341,0.00455116726388009));
#41162=CARTESIAN_POINT('',(8.75,-4.942,-6.05220448138622E-16));
#41163=CARTESIAN_POINT('Ctrl Pts',(13.7643204546569,-4.94198723275246,0.00456325735460533));
#41164=CARTESIAN_POINT('Ctrl Pts',(13.7519473103988,-4.94554485058906,0.388644192184096));
#41165=CARTESIAN_POINT('Ctrl Pts',(13.7395741661407,-4.90456715137494,0.7719772057555));
#41166=CARTESIAN_POINT('Ctrl Pts',(13.7272010218827,-4.8161816818024,1.14405398553911));
#41167=CARTESIAN_POINT('Ctrl Pts',(13.6741677311278,-4.43734731209181,2.73883503987936));
#41168=CARTESIAN_POINT('Ctrl Pts',(13.6211344403729,-3.18757636531753,4.12682582225269));
#41169=CARTESIAN_POINT('Ctrl Pts',(13.568101149618,-1.64107775501197,4.67026475588749));
#41170=CARTESIAN_POINT('Ctrl Pts',(13.5150678588631,-0.0945791447063754,
5.2137036895223));
#41171=CARTESIAN_POINT('Ctrl Pts',(13.4620345681082,1.74864712913051,4.91259077441855));
#41172=CARTESIAN_POINT('Ctrl Pts',(13.4090012773533,3.04184000442437,3.90531638018477));
#41173=CARTESIAN_POINT('Ctrl Pts',(13.3559679865984,4.33503287971822,2.89804198595098));
#41174=CARTESIAN_POINT('Ctrl Pts',(13.3029346958435,5.07819235646905,1.18460611258716));
#41175=CARTESIAN_POINT('Ctrl Pts',(13.2499014050887,4.92989087406059,-0.447857354634542));
#41176=CARTESIAN_POINT('Ctrl Pts',(13.1968681143338,4.78158939165213,-2.08032082185625));
#41177=CARTESIAN_POINT('Ctrl Pts',(13.1438348235789,3.74182695008439,-3.63181188293583));
#41178=CARTESIAN_POINT('Ctrl Pts',(13.090801532824,2.28828517637576,-4.38954982336234));
#41179=CARTESIAN_POINT('Ctrl Pts',(13.0377682420691,0.83474340266712,-5.14728776378884));
#41180=CARTESIAN_POINT('Ctrl Pts',(12.9847349513142,-1.03257770318241,-5.11127258356227));
#41181=CARTESIAN_POINT('Ctrl Pts',(12.9317016605593,-2.45582271629555,-4.29805800017847));
#41182=CARTESIAN_POINT('Ctrl Pts',(12.8786683698044,-3.8790677294087,-3.48484341679467));
#41183=CARTESIAN_POINT('Ctrl Pts',(12.8256350790495,-4.85823664978545,-1.89442943025364));
#41184=CARTESIAN_POINT('Ctrl Pts',(12.7726017882947,-4.94349069109905,-0.257458430829869));
#41185=CARTESIAN_POINT('Ctrl Pts',(12.7698413437487,-4.94792826323556,-0.17225218390715));
#41186=CARTESIAN_POINT('Ctrl Pts',(12.7670808992028,-4.94994393057285,-0.0869197989643819));
#41187=CARTESIAN_POINT('Ctrl Pts',(12.7643204546569,-4.949590084061,-0.00157034721157134));
#41188=CARTESIAN_POINT('Ctrl Pts',(12.6196795453431,-4.94998806776073,-0.000908059682992989));
#41189=CARTESIAN_POINT('Ctrl Pts',(12.6212503052083,-4.95011050264269,-0.0494635468567493));
#41190=CARTESIAN_POINT('Ctrl Pts',(12.6228210650735,-4.94945813523979,-0.0980156616365649));
#41191=CARTESIAN_POINT('Ctrl Pts',(12.6243918249387,-4.94802086470688,-0.146544529912058));
#41192=CARTESIAN_POINT('Ctrl Pts',(12.6774251156936,-4.89949455094414,-1.78501622648295));
#41193=CARTESIAN_POINT('Ctrl Pts',(12.7304584064485,-3.95623489530868,-3.3969885733841));
#41194=CARTESIAN_POINT('Ctrl Pts',(12.7834916972034,-2.55158197219604,-4.24191143928385));
#41195=CARTESIAN_POINT('Ctrl Pts',(12.8365249879583,-1.14692904908337,-5.08683430518362));
#41196=CARTESIAN_POINT('Ctrl Pts',(12.8895582787132,0.719117141506524,-5.16470769008199));
#41197=CARTESIAN_POINT('Ctrl Pts',(12.9425915694681,2.18928350503452,-4.43975501421699));
#41198=CARTESIAN_POINT('Ctrl Pts',(12.995624860223,3.65944986856251,-3.71480233835198));
#41199=CARTESIAN_POINT('Ctrl Pts',(13.0486581509778,4.73373640502861,-2.18702360172358));
#41200=CARTESIAN_POINT('Ctrl Pts',(13.1016914417327,4.91860735974007,-0.558292365221102));
#41201=CARTESIAN_POINT('Ctrl Pts',(13.1547247324876,5.10347831445153,1.07043887128138));
#41202=CARTESIAN_POINT('Ctrl Pts',(13.2077580232425,4.39893368740835,2.80012260765795));
#41203=CARTESIAN_POINT('Ctrl Pts',(13.2607913139974,3.12864872498507,3.83613459652236));
#41204=CARTESIAN_POINT('Ctrl Pts',(13.3138246047523,1.85836376256179,4.87214658538676));
#41205=CARTESIAN_POINT('Ctrl Pts',(13.3668578955072,0.0223384647584107,
5.21448682673899));
#41206=CARTESIAN_POINT('Ctrl Pts',(13.4198911862621,-1.53595051362779,4.70587466445995));
#41207=CARTESIAN_POINT('Ctrl Pts',(13.472924477017,-3.09423949201398,4.19726250218091));
#41208=CARTESIAN_POINT('Ctrl Pts',(13.5259577677719,-4.37479215098299,2.8376979362706));
#41209=CARTESIAN_POINT('Ctrl Pts',(13.5789910585267,-4.78930381973335,1.2517878520372));
#41210=CARTESIAN_POINT('Ctrl Pts',(13.5925538874655,-4.89531177768519,0.846204361392297));
#41211=CARTESIAN_POINT('Ctrl Pts',(13.6061167164043,-4.94467730729444,0.42581699893638));
#41212=CARTESIAN_POINT('Ctrl Pts',(13.6196795453431,-4.94087041225341,0.00455116726388009));
#41213=CARTESIAN_POINT('Origin',(8.75,0.,0.));
#41214=CARTESIAN_POINT('',(14.7643204546569,-4.93250450453637,0.00244705770993248));
#41215=CARTESIAN_POINT('',(14.6196795453431,-4.93380912478971,-0.000781869070653209));
#41216=CARTESIAN_POINT('',(8.75,-4.942,-6.05220448138622E-16));
#41217=CARTESIAN_POINT('Ctrl Pts',(14.7643204546569,-4.93235156762733,0.00248647065513752));
#41218=CARTESIAN_POINT('Ctrl Pts',(14.7368137215948,-4.93231616464049,0.858797103940552));
#41219=CARTESIAN_POINT('Ctrl Pts',(14.7093069885327,-4.72122797606844,1.71429698878651));
#41220=CARTESIAN_POINT('Ctrl Pts',(14.6818002554707,-4.30032841604571,2.45180850600084));
#41221=CARTESIAN_POINT('Ctrl Pts',(14.6287669647158,-3.48882932980696,3.87373900713432));
#41222=CARTESIAN_POINT('Ctrl Pts',(14.5757336739609,-1.89741367011298,4.85707991822524));
#41223=CARTESIAN_POINT('Ctrl Pts',(14.522700383206,-0.260105224363101,4.94413079607572));
#41224=CARTESIAN_POINT('Ctrl Pts',(14.4696670924511,1.37720322138678,5.03118167392621));
#41225=CARTESIAN_POINT('Ctrl Pts',(14.4166338016962,3.06040445319256,4.22194251853627));
#41226=CARTESIAN_POINT('Ctrl Pts',(14.3636005109413,4.01768931210048,2.89107485014993));
#41227=CARTESIAN_POINT('Ctrl Pts',(14.3105672201864,4.9749741710084,1.56020718176359));
#41228=CARTESIAN_POINT('Ctrl Pts',(14.2575339294315,5.20634265701846,-0.292288999619142));
#41229=CARTESIAN_POINT('Ctrl Pts',(14.2045006386767,4.60474522293428,-1.81685003135272));
#41230=CARTESIAN_POINT('Ctrl Pts',(14.1514673479218,4.0031477888501,-3.34141106308629));
#41231=CARTESIAN_POINT('Ctrl Pts',(14.0984340571669,2.56858443467169,-4.5380369451707));
#41232=CARTESIAN_POINT('Ctrl Pts',(14.045400766412,0.960497304699148,-4.85621770190632));
#41233=CARTESIAN_POINT('Ctrl Pts',(13.9923674756571,-0.64758982527339,-5.17439845864193));
#41234=CARTESIAN_POINT('Ctrl Pts',(13.9393341849022,-2.42920073104005,-4.61413409002874));
#41235=CARTESIAN_POINT('Ctrl Pts',(13.8863008941473,-3.56605728759995,-3.43321624256855));
#41236=CARTESIAN_POINT('Ctrl Pts',(13.8456407476505,-4.43767497297469,-2.5278171621994));
#41237=CARTESIAN_POINT('Ctrl Pts',(13.8049806011537,-4.93029632707818,-1.25758860566906));
#41238=CARTESIAN_POINT('Ctrl Pts',(13.7643204546569,-4.94198723275246,0.00456325735460533));
#41239=CARTESIAN_POINT('Ctrl Pts',(13.6196795453431,-4.94087041225341,0.00455116726388009));
#41240=CARTESIAN_POINT('Ctrl Pts',(13.6591500071592,-4.92979160959116,-1.22141407925688));
#41241=CARTESIAN_POINT('Ctrl Pts',(13.6986204689753,-4.46838339598338,-2.45481928224828));
#41242=CARTESIAN_POINT('Ctrl Pts',(13.7380909307914,-3.6421712883116,-3.3524436960653));
#41243=CARTESIAN_POINT('Ctrl Pts',(13.7911242215463,-2.53205640960778,-4.5585095573779));
#41244=CARTESIAN_POINT('Ctrl Pts',(13.8441575123012,-0.763355973668449,
-5.15838567744665));
#41245=CARTESIAN_POINT('Ctrl Pts',(13.8971908030561,0.85141559526732,-4.87643353874572));
#41246=CARTESIAN_POINT('Ctrl Pts',(13.950224093811,2.46618716420311,-4.59448140004478));
#41247=CARTESIAN_POINT('Ctrl Pts',(14.0032573845658,3.92702986613531,-3.43070100257412));
#41248=CARTESIAN_POINT('Ctrl Pts',(14.0562906753207,4.56274980759158,-1.9198394346831));
#41249=CARTESIAN_POINT('Ctrl Pts',(14.1093239660756,5.19846974904784,-0.408977866792093));
#41250=CARTESIAN_POINT('Ctrl Pts',(14.1623572568305,5.00906693002818,1.44896487151931));
#41251=CARTESIAN_POINT('Ctrl Pts',(14.2153905475854,4.08169456080327,2.80062703726421));
#41252=CARTESIAN_POINT('Ctrl Pts',(14.2684238383403,3.15432219157834,4.15228920300912));
#41253=CARTESIAN_POINT('Ctrl Pts',(14.3214571290952,1.48898027214817,4.99767079618755));
#41254=CARTESIAN_POINT('Ctrl Pts',(14.3744904198501,-0.149531273418242,
4.94803484746135));
#41255=CARTESIAN_POINT('Ctrl Pts',(14.427523710605,-1.78804281898468,4.89839889873514));
#41256=CARTESIAN_POINT('Ctrl Pts',(14.4805570013599,-3.39972399068732,3.95374540810427));
#41257=CARTESIAN_POINT('Ctrl Pts',(14.5335902921148,-4.243641679441,2.54875117840475));
#41258=CARTESIAN_POINT('Ctrl Pts',(14.5622867098575,-4.70028719761052,1.78850604242019));
#41259=CARTESIAN_POINT('Ctrl Pts',(14.5909831276003,-4.93213822096086,0.893477127079331));
#41260=CARTESIAN_POINT('Ctrl Pts',(14.6196795453431,-4.93380912478971,-0.000781869070653209));
#41261=CARTESIAN_POINT('Origin',(0.59341010809499,0.,0.));
#41262=CARTESIAN_POINT('',(14.093410108095,-4.37198870530024,0.00403694074333234));
#41263=CARTESIAN_POINT('',(14.290589891905,-4.36475384329838,-0.000691689918779215));
#41264=CARTESIAN_POINT('',(0.59341010809499,-4.372,-3.0022354348761E-13));
#41265=CARTESIAN_POINT('',(15.,-3.64743349744463,2.4217429795102));
#41266=CARTESIAN_POINT('Ctrl Pts',(14.093410108095,-4.37198870530024,0.00403694074333216));
#41267=CARTESIAN_POINT('Ctrl Pts',(14.1340702545918,-4.36164620436778,-1.11254095183847));
#41268=CARTESIAN_POINT('Ctrl Pts',(14.2277636918435,-3.35742155165682,-3.70194317815195));
#41269=CARTESIAN_POINT('Ctrl Pts',(14.3744904198501,1.00322544797992,-5.07323874560084));
#41270=CARTESIAN_POINT('Ctrl Pts',(14.5335902921147,4.810536850935,-1.89741011965601));
#41271=CARTESIAN_POINT('Ctrl Pts',(14.6926901643794,4.19648807260473,3.01908925610601));
#41272=CARTESIAN_POINT('Ctrl Pts',(14.8481600670078,-0.168782852515597,
5.11779741395519));
#41273=CARTESIAN_POINT('Ctrl Pts',(14.9505966788814,-2.89351652081187,3.54232264574166));
#41274=CARTESIAN_POINT('Ctrl Pts',(15.,-3.64743349744463,2.4217429795102));
#41275=CARTESIAN_POINT('',(15.,1.10295997362678,4.23058663740352));
#41276=CARTESIAN_POINT('Origin',(15.,0.,0.));
#41277=CARTESIAN_POINT('Ctrl Pts',(14.290589891905,-4.36475384329838,-0.000691689918779284));
#41278=CARTESIAN_POINT('Ctrl Pts',(14.3149267649171,-4.36600746342641,-0.671622630368523));
#41279=CARTESIAN_POINT('Ctrl Pts',(14.3922969286841,-3.90437662282341,-2.80304411594494));
#41280=CARTESIAN_POINT('Ctrl Pts',(14.522700383206,-0.581919347715841,-5.1410577240212));
#41281=CARTESIAN_POINT('Ctrl Pts',(14.6818002554707,4.01308660375755,-3.2607181841902));
#41282=CARTESIAN_POINT('Ctrl Pts',(14.8143834823579,4.75806562994111,0.786704444467226));
#41283=CARTESIAN_POINT('Ctrl Pts',(14.9204500638677,3.11408383257965,3.31830903713004));
#41284=CARTESIAN_POINT('Ctrl Pts',(14.9734833546226,1.80781376844615,4.04682358287313));
#41285=CARTESIAN_POINT('Ctrl Pts',(15.,1.10295997362678,4.23058663740352));
#41286=CARTESIAN_POINT('Origin',(0.59341010809499,0.,0.));
#41287=CARTESIAN_POINT('',(13.093410108095,-4.37871465955376,-0.00138922663093295));
#41288=CARTESIAN_POINT('',(13.290589891905,-4.37100069655441,0.0040262450982749));
#41289=CARTESIAN_POINT('',(0.59341010809499,-4.372,-3.0022354348761E-13));
#41290=CARTESIAN_POINT('Ctrl Pts',(13.093410108095,-4.37871465955376,-0.00138922663093346));
#41291=CARTESIAN_POINT('Ctrl Pts',(13.0961705526409,-4.37902769414498,-0.0768946501564255));
#41292=CARTESIAN_POINT('Ctrl Pts',(13.1519642879417,-4.34298620877237,-1.60269498775243));
#41293=CARTESIAN_POINT('Ctrl Pts',(13.2607913139974,-2.56543051256322,-4.48988777162764));
#41294=CARTESIAN_POINT('Ctrl Pts',(13.4198911862621,2.39041400874848,-4.58547156439403));
#41295=CARTESIAN_POINT('Ctrl Pts',(13.5789910585267,5.14992922194199,-0.467835636203029));
#41296=CARTESIAN_POINT('Ctrl Pts',(13.7380909307914,3.17759419623094,4.07959959549261));
#41297=CARTESIAN_POINT('Ctrl Pts',(13.8971908030561,-1.71430297245472,4.87874912898118));
#41298=CARTESIAN_POINT('Ctrl Pts',(14.0156305288239,-4.18350516313649,2.13646272095719));
#41299=CARTESIAN_POINT('Ctrl Pts',(14.0810369638369,-4.37513599489588,0.343818779487714));
#41300=CARTESIAN_POINT('Ctrl Pts',(14.093410108095,-4.37198870530024,0.00403694074333216));
#41301=CARTESIAN_POINT('Ctrl Pts',(13.290589891905,-4.37100069655441,0.00402624509827507));
#41302=CARTESIAN_POINT('Ctrl Pts',(13.3300603537211,-4.36119969994578,-1.08053872005514));
#41303=CARTESIAN_POINT('Ctrl Pts',(13.4225641062921,-3.40455674710145,-3.63777190456466));
#41304=CARTESIAN_POINT('Ctrl Pts',(13.568101149618,0.889390123239341,-5.09411585972022));
#41305=CARTESIAN_POINT('Ctrl Pts',(13.7272010218827,4.7664465535393,-2.00545869799919));
#41306=CARTESIAN_POINT('Ctrl Pts',(13.8863008941473,4.26377407797028,2.92549576490892));
#41307=CARTESIAN_POINT('Ctrl Pts',(14.045400766412,-0.156020461739612,5.16912688108217));
#41308=CARTESIAN_POINT('Ctrl Pts',(14.1801637656646,-3.77910640678081,3.04553020145906));
#41309=CARTESIAN_POINT('Ctrl Pts',(14.2618934741622,-4.36327565804152,0.790425333789909));
#41310=CARTESIAN_POINT('Ctrl Pts',(14.290589891905,-4.36475384329838,-0.000691689918779284));
#41311=CARTESIAN_POINT('Origin',(0.59341010809499,0.,0.));
#41312=CARTESIAN_POINT('',(12.093410108095,-4.367758511641,-0.00335521914055352));
#41313=CARTESIAN_POINT('',(12.290589891905,-4.37906674064143,-0.000803325968382063));
#41314=CARTESIAN_POINT('',(0.59341010809499,-4.372,-3.0022354348761E-13));
#41315=CARTESIAN_POINT('Ctrl Pts',(12.093410108095,-4.367758511641,-0.00335521914055378));
#41316=CARTESIAN_POINT('Ctrl Pts',(12.1113041414449,-4.37126345793821,-0.495971696895518));
#41317=CARTESIAN_POINT('Ctrl Pts',(12.1822314655497,-4.06664955489653,-2.44436906711752));
#41318=CARTESIAN_POINT('Ctrl Pts',(12.3061920804094,-1.19826567241535,-5.0303809958746));
#41319=CARTESIAN_POINT('Ctrl Pts',(12.4652919526741,3.58420434344045,-3.72747292097139));
#41320=CARTESIAN_POINT('Ctrl Pts',(12.6243918249387,5.07346067115539,1.00028675173837));
#41321=CARTESIAN_POINT('Ctrl Pts',(12.7834916972034,1.90115420721842,4.80896873992654));
#41322=CARTESIAN_POINT('Ctrl Pts',(12.9398311249222,-2.93260813533299,4.20969054412402));
#41323=CARTESIAN_POINT('Ctrl Pts',(13.043137261886,-4.37301371552075,1.37370542993683));
#41324=CARTESIAN_POINT('Ctrl Pts',(13.093410108095,-4.37871465955376,-0.00138922663093346));
#41325=CARTESIAN_POINT('Ctrl Pts',(12.290589891905,-4.37906674064143,-0.000803325968382323));
#41326=CARTESIAN_POINT('Ctrl Pts',(12.2921606517702,-4.37917505413878,-0.0437585242530951));
#41327=CARTESIAN_POINT('Ctrl Pts',(12.3467647023903,-4.35911256894886,-1.53689886108888));
#41328=CARTESIAN_POINT('Ctrl Pts',(12.4544020437653,-2.66546494290799,-4.43123778702695));
#41329=CARTESIAN_POINT('Ctrl Pts',(12.61350191603,2.28699597084696,-4.63791267903968));
#41330=CARTESIAN_POINT('Ctrl Pts',(12.7726017882947,5.13813765686258,-0.583208933669766));
#41331=CARTESIAN_POINT('Ctrl Pts',(12.9317016605593,3.2682859109503,4.00734790289743));
#41332=CARTESIAN_POINT('Ctrl Pts',(13.090801532824,-1.60449996642509,4.91591419297749));
#41333=CARTESIAN_POINT('Ctrl Pts',(13.2104309432726,-4.15993144754704,2.20280898171477));
#41334=CARTESIAN_POINT('Ctrl Pts',(13.2770270629662,-4.37436851224028,0.376704152033278));
#41335=CARTESIAN_POINT('Ctrl Pts',(13.290589891905,-4.37100069655441,0.00402624509827507));
#41336=CARTESIAN_POINT('Origin',(0.59341010809499,0.,0.));
#41337=CARTESIAN_POINT('',(11.093410108095,-4.36651870188269,0.00271890834687631));
#41338=CARTESIAN_POINT('',(11.290589891905,-4.3685707734135,-0.00363129594146361));
#41339=CARTESIAN_POINT('',(0.59341010809499,-4.372,-3.0022354348761E-13));
#41340=CARTESIAN_POINT('Ctrl Pts',(11.093410108095,-4.36651870188269,0.00271890834687608));
#41341=CARTESIAN_POINT('Ctrl Pts',(11.1264377302489,-4.36136931891016,-0.907168341484959));
#41342=CARTESIAN_POINT('Ctrl Pts',(11.2124986431577,-3.63931805594909,-3.28556918685279));
#41343=CARTESIAN_POINT('Ctrl Pts',(11.3515928468214,0.265749570496903,-5.16429585585985));
#41344=CARTESIAN_POINT('Ctrl Pts',(11.5106927190861,4.4883018395813,-2.56821360809099));
#41345=CARTESIAN_POINT('Ctrl Pts',(11.6697925913507,4.58694349318866,2.38757701187169));
#41346=CARTESIAN_POINT('Ctrl Pts',(11.8288924636154,0.471041268600573,5.14963052385883));
#41347=CARTESIAN_POINT('Ctrl Pts',(11.9700983025302,-3.56606539792994,3.4016459105259));
#41348=CARTESIAN_POINT('Ctrl Pts',(12.05827085069,-4.36087570284549,0.964016243473005));
#41349=CARTESIAN_POINT('Ctrl Pts',(12.093410108095,-4.367758511641,-0.00335521914055378));
#41350=CARTESIAN_POINT('Ctrl Pts',(11.290589891905,-4.3685707734135,-0.00363129594146409));
#41351=CARTESIAN_POINT('Ctrl Pts',(11.3072942405742,-4.37215648678634,-0.463280891549555));
#41352=CARTESIAN_POINT('Ctrl Pts',(11.3770318799983,-4.09347257870959,-2.3779972764569));
#41353=CARTESIAN_POINT('Ctrl Pts',(11.4998028101773,-1.31076150706236,-5.00224776370858));
#41354=CARTESIAN_POINT('Ctrl Pts',(11.658902682442,3.49972182018105,-3.80690501300621));
#41355=CARTESIAN_POINT('Ctrl Pts',(11.8180025547066,5.09461487296727,0.886272086847998));
#41356=CARTESIAN_POINT('Ctrl Pts',(11.9771024269713,2.00850883058607,4.76513062511062));
#41357=CARTESIAN_POINT('Ctrl Pts',(12.1346315393708,-2.87435311497258,4.27065541760681));
#41358=CARTESIAN_POINT('Ctrl Pts',(12.2391273610153,-4.37551808446131,1.40653032672016));
#41359=CARTESIAN_POINT('Ctrl Pts',(12.290589891905,-4.37906674064143,-0.000803325968382323));
#41360=CARTESIAN_POINT('Origin',(0.59341010809499,0.,0.));
#41361=CARTESIAN_POINT('',(10.093410108095,-4.37771132272003,0.00233247625034503));
#41362=CARTESIAN_POINT('',(10.290589891905,-4.3659514196814,0.00229030427700283));
#41363=CARTESIAN_POINT('',(0.59341010809499,-4.372,-3.0022354348761E-13));
#41364=CARTESIAN_POINT('Ctrl Pts',(10.093410108095,-4.37771132272003,0.00233247625034497));
#41365=CARTESIAN_POINT('Ctrl Pts',(10.1415713190529,-4.36921541818575,-1.31580361571968));
#41366=CARTESIAN_POINT('Ctrl Pts',(10.2427658207657,-3.03288703287329,-4.10034412525587));
#41367=CARTESIAN_POINT('Ctrl Pts',(10.3969936132334,1.70828597395473,-4.88081279799705));
#41368=CARTESIAN_POINT('Ctrl Pts',(10.556093485498,5.02963780132612,-1.20138175675703));
#41369=CARTESIAN_POINT('Ctrl Pts',(10.7151933577627,3.72969242293982,3.58189460618598));
#41370=CARTESIAN_POINT('Ctrl Pts',(10.8742932300274,-0.997143291267936,
5.07407920638337));
#41371=CARTESIAN_POINT('Ctrl Pts',(11.0003654801381,-4.01673646885604,2.56218392279602));
#41372=CARTESIAN_POINT('Ctrl Pts',(11.073404439494,-4.36963781378144,0.553860698075588));
#41373=CARTESIAN_POINT('Ctrl Pts',(11.093410108095,-4.36651870188269,0.00271890834687608));
#41374=CARTESIAN_POINT('Ctrl Pts',(10.290589891905,-4.3659514196814,0.00229030427700276));
#41375=CARTESIAN_POINT('Ctrl Pts',(10.3224278293782,-4.36180234903057,-0.875107575648617));
#41376=CARTESIAN_POINT('Ctrl Pts',(10.4072990576063,-3.67904443619338,-3.21995217888924));
#41377=CARTESIAN_POINT('Ctrl Pts',(10.5452035765893,0.149882990889038,-5.1689567258239));
#41378=CARTESIAN_POINT('Ctrl Pts',(10.704303448854,4.42958624251035,-2.66820993668828));
#41379=CARTESIAN_POINT('Ctrl Pts',(10.8634033211187,4.63932753487269,2.28412315339565));
#41380=CARTESIAN_POINT('Ctrl Pts',(11.0225031933833,0.586393813370393,5.13777391729214));
#41381=CARTESIAN_POINT('Ctrl Pts',(11.1648987169788,-3.52322847002093,3.46679259372449));
#41382=CARTESIAN_POINT('Ctrl Pts',(11.2542609498193,-4.36077249429243,0.996023576525303));
#41383=CARTESIAN_POINT('Ctrl Pts',(11.290589891905,-4.3685707734135,-0.00363129594146409));
#41384=CARTESIAN_POINT('Origin',(0.59341010809499,0.,0.));
#41385=CARTESIAN_POINT('',(9.09341010809498,-4.37375961462363,-0.00386210780576171));
#41386=CARTESIAN_POINT('',(9.29058989190502,-4.37697467402181,0.00279126523279556));
#41387=CARTESIAN_POINT('',(0.59341010809499,-4.372,-3.0022354348761E-13));
#41388=CARTESIAN_POINT('Ctrl Pts',(9.09341010809498,-4.37375961462363,-0.00386210780576188));
#41389=CARTESIAN_POINT('Ctrl Pts',(9.103671617102,-4.37635512773107,-0.285372867093846));
#41390=CARTESIAN_POINT('Ctrl Pts',(9.16696641686391,-4.22313498793317,-2.01896688929275));
#41391=CARTESIAN_POINT('Ctrl Pts',(9.28329450738073,-1.90711126815764,-4.80661015155663));
#41392=CARTESIAN_POINT('Ctrl Pts',(9.44239437964536,3.01275227347471,-4.20284407001334));
#41393=CARTESIAN_POINT('Ctrl Pts',(9.60149425191006,5.16445949583093,0.26255028868963));
#41394=CARTESIAN_POINT('Ctrl Pts',(9.76059412417471,2.5709935704035,4.48670999721959));
#41395=CARTESIAN_POINT('Ctrl Pts',(9.91969399643938,-2.38473498159332,4.58842169004869));
#41396=CARTESIAN_POINT('Ctrl Pts',(10.0306326577461,-4.3124633006313,1.7196401851414));
#41397=CARTESIAN_POINT('Ctrl Pts',(10.088538028298,-4.37857078459848,0.135677632977564));
#41398=CARTESIAN_POINT('Ctrl Pts',(10.093410108095,-4.37771132272003,0.00233247625034497));
#41399=CARTESIAN_POINT('Ctrl Pts',(9.29058989190502,-4.37697467402181,0.00279126523279523));
#41400=CARTESIAN_POINT('Ctrl Pts',(9.33756141818222,-4.36742454004203,-1.28335333651436));
#41401=CARTESIAN_POINT('Ctrl Pts',(9.43756623521432,-3.08763898870623,-4.03814554925744));
#41402=CARTESIAN_POINT('Ctrl Pts',(9.59060434300129,1.59841338882536,-4.91789113187562));
#41403=CARTESIAN_POINT('Ctrl Pts',(9.74970421526597,5.00143481089275,-1.31386010630501));
#41404=CARTESIAN_POINT('Ctrl Pts',(9.90880408753063,3.80907230476851,3.49736282416303));
#41405=CARTESIAN_POINT('Ctrl Pts',(10.0679039597953,-0.883115813962409,
5.09516290273885));
#41406=CARTESIAN_POINT('Ctrl Pts',(10.1951658945868,-3.98729343645151,2.62854910513976));
#41407=CARTESIAN_POINT('Ctrl Pts',(10.2693945386233,-4.36871356526036,0.586397175184639));
#41408=CARTESIAN_POINT('Ctrl Pts',(10.290589891905,-4.3659514196814,0.00229030427700276));
#41409=CARTESIAN_POINT('Origin',(0.59341010809499,0.,0.));
#41410=CARTESIAN_POINT('',(8.09341010809498,-4.36482287045854,-0.000510875517043062));
#41411=CARTESIAN_POINT('',(8.29058989190502,-4.37473563964834,-0.00365333953792402));
#41412=CARTESIAN_POINT('',(0.59341010809499,-4.372,-3.0022354348761E-13));
#41413=CARTESIAN_POINT('Ctrl Pts',(8.09341010809498,-4.36482287045854,-0.000510875517042778));
#41414=CARTESIAN_POINT('Ctrl Pts',(8.118805205906,-4.36555029137901,-0.70080710120195));
#41415=CARTESIAN_POINT('Ctrl Pts',(8.1972335944719,-3.87549509935531,-2.86259042526824));
#41416=CARTESIAN_POINT('Ctrl Pts',(8.32869527379272,-0.477421201803847,
-5.14904297265438));
#41417=CARTESIAN_POINT('Ctrl Pts',(8.48779514605736,4.07371659009023,-3.18518565892236));
#41418=CARTESIAN_POINT('Ctrl Pts',(8.64689501832206,4.8818701276596,1.70526203113781));
#41419=CARTESIAN_POINT('Ctrl Pts',(8.8059948905867,1.20449733678236,5.02889259219775));
#41420=CARTESIAN_POINT('Ctrl Pts',(8.95483325384436,-3.27102321588964,3.81556246242598));
#41421=CARTESIAN_POINT('Ctrl Pts',(9.05063832634711,-4.36294105761814,1.16952445236876));
#41422=CARTESIAN_POINT('Ctrl Pts',(9.09341010809498,-4.37375961462363,-0.00386210780576188));
#41423=CARTESIAN_POINT('Ctrl Pts',(8.29058989190502,-4.37473563964834,-0.00365333953792416));
#41424=CARTESIAN_POINT('Ctrl Pts',(8.29966171623133,-4.37696429033364,-0.252383457015382));
#41425=CARTESIAN_POINT('Ctrl Pts',(8.36176683131253,-4.24430437552142,-1.95279653103946));
#41426=CARTESIAN_POINT('Ctrl Pts',(8.47690523714862,-2.01441124631645,-4.76263854153384));
#41427=CARTESIAN_POINT('Ctrl Pts',(8.63600510941329,2.91775399818566,-4.26934305867557));
#41428=CARTESIAN_POINT('Ctrl Pts',(8.79510498167796,5.16904858522312,0.146680844662566));
#41429=CARTESIAN_POINT('Ctrl Pts',(8.95420485394263,2.67095350892793,4.42793246332181));
#41430=CARTESIAN_POINT('Ctrl Pts',(9.1133047262073,-2.28124869702632,4.64074163565498));
#41431=CARTESIAN_POINT('Ctrl Pts',(9.22543307219475,-4.29417680922933,1.78561397709894));
#41432=CARTESIAN_POINT('Ctrl Pts',(9.28452812742733,-4.37820713690952,0.168770663347971));
#41433=CARTESIAN_POINT('Ctrl Pts',(9.29058989190502,-4.37697467402181,0.00279126523279523));
#41434=CARTESIAN_POINT('Origin',(0.59341010809499,0.,0.));
#41435=CARTESIAN_POINT('',(7.09341010809498,-4.37187842794764,0.00403998300431283));
#41436=CARTESIAN_POINT('',(7.29058989190502,-4.36499662426206,-0.00104393836387107));
#41437=CARTESIAN_POINT('',(0.59341010809499,-4.372,-3.0022354348761E-13));
#41438=CARTESIAN_POINT('Ctrl Pts',(7.09341010809498,-4.37187842794764,0.00403998300431242));
#41439=CARTESIAN_POINT('Ctrl Pts',(7.13393879471,-4.3616057311049,-1.1090376187109));
#41440=CARTESIAN_POINT('Ctrl Pts',(7.22750077207991,-3.36276294787998,-3.69501069902628));
#41441=CARTESIAN_POINT('Ctrl Pts',(7.3740960402047,0.990855843724147,-5.07531075254117));
#41442=CARTESIAN_POINT('Ctrl Pts',(7.53319591246937,4.80542779279021,-1.91008854942909));
#41443=CARTESIAN_POINT('Ctrl Pts',(7.69229578473403,4.20470963362949,3.01014807526144));
#41444=CARTESIAN_POINT('Ctrl Pts',(7.8513956569987,-0.25935090699094,5.16462115214535));
#41445=CARTESIAN_POINT('Ctrl Pts',(7.98510043145236,-3.81061099465694,2.98731690196163));
#41446=CARTESIAN_POINT('Ctrl Pts',(8.06577191515111,-4.36403119799085,0.76164103062551));
#41447=CARTESIAN_POINT('Ctrl Pts',(8.09341010809498,-4.36482287045854,-0.000510875517042778));
#41448=CARTESIAN_POINT('Ctrl Pts',(7.29058989190502,-4.36499662426206,-0.00104393836387148));
#41449=CARTESIAN_POINT('Ctrl Pts',(7.31479530503533,-4.36641655013163,-0.668467298906582));
#41450=CARTESIAN_POINT('Ctrl Pts',(7.39203400892053,-3.90842952464144,-2.79634607106463));
#41451=CARTESIAN_POINT('Ctrl Pts',(7.52230600356061,-0.59275896293977,-5.13704344525249));
#41452=CARTESIAN_POINT('Ctrl Pts',(7.68140587582529,4.00127074294363,-3.27573060374049));
#41453=CARTESIAN_POINT('Ctrl Pts',(7.84050574808995,4.91888038941839,1.59536649744721));
#41454=CARTESIAN_POINT('Ctrl Pts',(7.99960562035462,1.31695819333312,5.00061992792881));
#41455=CARTESIAN_POINT('Ctrl Pts',(8.14963366829297,-3.2206259976218,3.87905632732833));
#41456=CARTESIAN_POINT('Ctrl Pts',(8.24662842547644,-4.36393574441683,1.20167651650311));
#41457=CARTESIAN_POINT('Ctrl Pts',(8.29058989190502,-4.37473563964834,-0.00365333953792416));
#41458=CARTESIAN_POINT('Origin',(0.59341010809499,0.,0.));
#41459=CARTESIAN_POINT('',(6.09341010809498,-4.37876152077167,-0.00132541857997806));
#41460=CARTESIAN_POINT('',(6.29058989190502,-4.37089328879944,0.00401979016151965));
#41461=CARTESIAN_POINT('',(0.59341010809499,-4.372,-3.0022354348761E-13));
#41462=CARTESIAN_POINT('Ctrl Pts',(6.09341010809498,-4.37876152077167,-0.00132541857997809));
#41463=CARTESIAN_POINT('Ctrl Pts',(6.09603909275911,-4.3790475944532,-0.0732330197592887));
#41464=CARTESIAN_POINT('Ctrl Pts',(6.15170136817812,-4.34480561702315,-1.5954211178316));
#41465=CARTESIAN_POINT('Ctrl Pts',(6.26039693435203,-2.57655053740016,-4.48352114617468));
#41466=CARTESIAN_POINT('Ctrl Pts',(6.41949680661669,2.37904818745876,-4.59137280590671));
#41467=CARTESIAN_POINT('Ctrl Pts',(6.57859667888136,5.14874622778692,-0.48061089166393));
#41468=CARTESIAN_POINT('Ctrl Pts',(6.73769655114603,3.18770867422774,4.07174261783812));
#41469=CARTESIAN_POINT('Ctrl Pts',(6.8967964234107,-1.70223743368489,4.8829255836368));
#41470=CARTESIAN_POINT('Ctrl Pts',(7.01536760906034,-4.18091231648288,2.14385213795481));
#41471=CARTESIAN_POINT('Ctrl Pts',(7.08090550395511,-4.37504793621934,0.347465737670911));
#41472=CARTESIAN_POINT('Ctrl Pts',(7.09341010809498,-4.37187842794764,0.00403998300431242));
#41473=CARTESIAN_POINT('Ctrl Pts',(6.29058989190502,-4.37089328879944,0.00401979016151986));
#41474=CARTESIAN_POINT('Ctrl Pts',(6.32992889383933,-4.36116316539251,-1.0770055517542));
#41475=CARTESIAN_POINT('Ctrl Pts',(6.42230118652852,-3.40970001782311,-3.63066936637308));
#41476=CARTESIAN_POINT('Ctrl Pts',(6.56770676997262,0.876802331596175,-5.09625315459363));
#41477=CARTESIAN_POINT('Ctrl Pts',(6.72680664223727,4.76138972002301,-2.0173612671069));
#41478=CARTESIAN_POINT('Ctrl Pts',(6.88590651450195,4.27114975899821,2.91510862278235));
#41479=CARTESIAN_POINT('Ctrl Pts',(7.04500638676661,-0.143478642277096,
5.16913846066508));
#41480=CARTESIAN_POINT('Ctrl Pts',(7.17990084590097,-3.77469316016274,3.0533520140145));
#41481=CARTESIAN_POINT('Ctrl Pts',(7.26176201428044,-4.36330553768636,0.793836068762296));
#41482=CARTESIAN_POINT('Ctrl Pts',(7.29058989190502,-4.36499662426206,-0.00104393836387148));
#41483=CARTESIAN_POINT('Origin',(0.59341010809499,0.,0.));
#41484=CARTESIAN_POINT('',(5.09341010809498,-4.36784450635769,-0.00338885911202358));
#41485=CARTESIAN_POINT('',(5.29058989190502,-4.37909474916464,-0.000736964456646283));
#41486=CARTESIAN_POINT('',(0.59341010809499,-4.372,-3.0022354348761E-13));
#41487=CARTESIAN_POINT('Ctrl Pts',(5.09341010809498,-4.3678445063577,-0.0033888591120243));
#41488=CARTESIAN_POINT('Ctrl Pts',(5.11117268156311,-4.37136316807571,-0.492362019923694));
#41489=CARTESIAN_POINT('Ctrl Pts',(5.18196854578612,-4.06965919180842,-2.43703442403858));
#41490=CARTESIAN_POINT('Ctrl Pts',(5.30579770076401,-1.21072695590433,-5.0273964823116));
#41491=CARTESIAN_POINT('Ctrl Pts',(5.46489757302869,3.57495682182765,-3.73634277167034));
#41492=CARTESIAN_POINT('Ctrl Pts',(5.62399744529335,5.07592364569998,0.98771152242332));
#41493=CARTESIAN_POINT('Ctrl Pts',(5.78309731755802,1.91306507591506,4.80424360372137));
#41494=CARTESIAN_POINT('Ctrl Pts',(5.93956820515856,-2.92623401914661,4.21644954493704));
#41495=CARTESIAN_POINT('Ctrl Pts',(6.04300580200421,-4.37327676249022,1.37732573505887));
#41496=CARTESIAN_POINT('Ctrl Pts',(6.09341010809498,-4.37876152077167,-0.00132541857997809));
#41497=CARTESIAN_POINT('Ctrl Pts',(5.29058989190502,-4.37909474916464,-0.000736964456646279));
#41498=CARTESIAN_POINT('Ctrl Pts',(5.29202919188843,-4.37918634404097,-0.0400964851336176));
#41499=CARTESIAN_POINT('Ctrl Pts',(5.34650178262674,-4.36084783999699,-1.52963244896985));
#41500=CARTESIAN_POINT('Ctrl Pts',(5.45400766411994,-2.67643755901513,-4.42461982427826));
#41501=CARTESIAN_POINT('Ctrl Pts',(5.6131075363846,2.27549715061658,-4.64356448598052));
#41502=CARTESIAN_POINT('Ctrl Pts',(5.77220740864928,5.13667525644702,-0.595941201221052));
#41503=CARTESIAN_POINT('Ctrl Pts',(5.93130728091394,3.27820871991814,3.9992406950588));
#41504=CARTESIAN_POINT('Ctrl Pts',(6.0904071531786,-1.5923189924077,4.91986775797726));
#41505=CARTESIAN_POINT('Ctrl Pts',(6.21016802350897,-4.15726929526591,2.21014455144395));
#41506=CARTESIAN_POINT('Ctrl Pts',(6.27689560308444,-4.37428043930257,0.380335215735453));
#41507=CARTESIAN_POINT('Ctrl Pts',(6.29058989190502,-4.37089328879944,0.00401979016151986));
#41508=CARTESIAN_POINT('Origin',(0.59341010809499,0.,0.));
#41509=CARTESIAN_POINT('',(4.09341010809498,-4.36644361699374,0.00266903102634173));
#41510=CARTESIAN_POINT('',(4.29058989190502,-4.36866463568371,-0.00365796780793459));
#41511=CARTESIAN_POINT('',(0.59341010809499,-4.372,-3.0022354348761E-13));
#41512=CARTESIAN_POINT('Ctrl Pts',(4.09341010809498,-4.36644361699374,0.0026690310263415));
#41513=CARTESIAN_POINT('Ctrl Pts',(4.1263062703671,-4.36140744813966,-0.903629915781166));
#41514=CARTESIAN_POINT('Ctrl Pts',(4.21223572339411,-3.6437738264693,-3.27831824856905));
#41515=CARTESIAN_POINT('Ctrl Pts',(4.35119846717601,0.252959447065525,-5.16494338006019));
#41516=CARTESIAN_POINT('Ctrl Pts',(4.51029833944068,4.48192017162094,-2.5793250070162));
#41517=CARTESIAN_POINT('Ctrl Pts',(4.66939821170534,4.59284779079654,2.37620209998279));
#41518=CARTESIAN_POINT('Ctrl Pts',(4.82849808397002,0.483799317188488,5.14844819531533));
#41519=CARTESIAN_POINT('Ctrl Pts',(4.96983538276656,-3.56138743320807,3.40885374374836));
#41520=CARTESIAN_POINT('Ctrl Pts',(5.05813939080822,-4.36085758394431,0.96755345095109));
#41521=CARTESIAN_POINT('Ctrl Pts',(5.09341010809498,-4.3678445063577,-0.0033888591120243));
#41522=CARTESIAN_POINT('Ctrl Pts',(4.29058989190502,-4.36866463568371,-0.00365796780793456));
#41523=CARTESIAN_POINT('Ctrl Pts',(4.30716278069244,-4.37225371700844,-0.459665188165218));
#41524=CARTESIAN_POINT('Ctrl Pts',(4.37676896023474,-4.09638109039665,-2.37066280594993));
#41525=CARTESIAN_POINT('Ctrl Pts',(4.49940843053193,-1.32315190100328,-4.99898526062427));
#41526=CARTESIAN_POINT('Ctrl Pts',(4.6585083027966,3.49027724579729,-3.81556502166019));
#41527=CARTESIAN_POINT('Ctrl Pts',(4.81760817506126,5.09679560530872,0.873644852702682));
#41528=CARTESIAN_POINT('Ctrl Pts',(4.97670804732593,2.02031037891206,4.76013919238013));
#41529=CARTESIAN_POINT('Ctrl Pts',(5.13436861960719,-2.86783763983711,4.27736208016393));
#41530=CARTESIAN_POINT('Ctrl Pts',(5.23899590113355,-4.37581138554451,1.41016748213276));
#41531=CARTESIAN_POINT('Ctrl Pts',(5.29058989190502,-4.37909474916464,-0.000736964456646279));
#41532=CARTESIAN_POINT('Origin',(0.59341010809499,0.,0.));
#41533=CARTESIAN_POINT('',(3.09341010809498,-4.3772103018885,0.00211459834950888));
#41534=CARTESIAN_POINT('',(3.29058989190502,-4.36585073597542,0.00220040158241119));
#41535=CARTESIAN_POINT('',(0.59341010809499,-4.372,-3.0022354348761E-13));
#41536=CARTESIAN_POINT('Ctrl Pts',(3.09341010809498,-4.3772103018885,0.00211459834950896));
#41537=CARTESIAN_POINT('Ctrl Pts',(3.1414398591711,-4.3684488623825,-1.31256865588346));
#41538=CARTESIAN_POINT('Ctrl Pts',(3.24250290100212,-3.03968752820866,-4.09305073566412));
#41539=CARTESIAN_POINT('Ctrl Pts',(3.396599233588,1.69656360505873,-4.88527221384132));
#41540=CARTESIAN_POINT('Ctrl Pts',(3.55569910585268,5.02644857336042,-1.21371541889335));
#41541=CARTESIAN_POINT('Ctrl Pts',(3.71479897811734,3.73865941844861,3.57257592687282));
#41542=CARTESIAN_POINT('Ctrl Pts',(3.87389885038201,-0.984620426994229,
5.07656875848712));
#41543=CARTESIAN_POINT('Ctrl Pts',(4.00010256037456,-4.01351918209848,2.56951083998331));
#41544=CARTESIAN_POINT('Ctrl Pts',(4.07327297961222,-4.3695264683743,0.55745284394327));
#41545=CARTESIAN_POINT('Ctrl Pts',(4.09341010809498,-4.36644361699374,0.0026690310263415));
#41546=CARTESIAN_POINT('Ctrl Pts',(3.29058989190502,-4.36585073597542,0.00220040158241119));
#41547=CARTESIAN_POINT('Ctrl Pts',(3.32229636949643,-4.36183077367725,-0.871586062571754));
#41548=CARTESIAN_POINT('Ctrl Pts',(3.40703613784273,-3.68343867970127,-3.21262781785179));
#41549=CARTESIAN_POINT('Ctrl Pts',(3.54480919694392,0.137121248351661,-5.16935479018605));
#41550=CARTESIAN_POINT('Ctrl Pts',(3.70390906920859,4.42293632971135,-2.67915589298676));
#41551=CARTESIAN_POINT('Ctrl Pts',(3.86300894147325,4.6449860818125,2.2726085151474));
#41552=CARTESIAN_POINT('Ctrl Pts',(4.02210881373793,0.599116510517935,5.13631111808859));
#41553=CARTESIAN_POINT('Ctrl Pts',(4.16463579721518,-3.51842248411001,3.4739769218908));
#41554=CARTESIAN_POINT('Ctrl Pts',(4.25412948993755,-4.36076864666985,0.999559200156457));
#41555=CARTESIAN_POINT('Ctrl Pts',(4.29058989190502,-4.36866463568371,-0.00365796780793456));
#41556=CARTESIAN_POINT('Ctrl Pts',(2.11291034656191,-1.91898364244009,3.92834389788462));
#41557=CARTESIAN_POINT('Ctrl Pts',(2.13942699193936,-2.57348107768915,3.6086239586659));
#41558=CARTESIAN_POINT('Ctrl Pts',(2.19246028269425,-3.70959326419019,2.63583208807155));
#41559=CARTESIAN_POINT('Ctrl Pts',(2.29852686420402,-4.81962414156407,-0.171217860704528));
#41560=CARTESIAN_POINT('Ctrl Pts',(2.43111009109125,-3.28780625975168,-3.99092434960932));
#41561=CARTESIAN_POINT('Ctrl Pts',(2.59020996335592,1.58858351891899,-4.92397269005252));
#41562=CARTESIAN_POINT('Ctrl Pts',(2.74930983562058,4.99693901203929,-1.32514448694853));
#41563=CARTESIAN_POINT('Ctrl Pts',(2.90840970788525,3.81836490750785,3.48733811875686));
#41564=CARTESIAN_POINT('Ctrl Pts',(3.06750958014992,-0.870820132749773,
5.09763547084385));
#41565=CARTESIAN_POINT('Ctrl Pts',(3.22660945241459,-4.75871313630775,2.02310260362725));
#41566=CARTESIAN_POINT('Ctrl Pts',(3.38570932467925,-4.27484870062277,-2.9097329643648));
#41567=CARTESIAN_POINT('Ctrl Pts',(3.54480919694392,0.137121248351661,-5.16935479018605));
#41568=CARTESIAN_POINT('Ctrl Pts',(3.70390906920859,4.42293632971135,-2.67915589298676));
#41569=CARTESIAN_POINT('Ctrl Pts',(3.86300894147325,4.6449860818125,2.2726085151474));
#41570=CARTESIAN_POINT('Ctrl Pts',(4.02210881373793,0.599116510517935,5.13631111808859));
#41571=CARTESIAN_POINT('Ctrl Pts',(4.18120868600259,-3.99720561815913,3.28068243765374));
#41572=CARTESIAN_POINT('Ctrl Pts',(4.34030855826727,-4.92085506071136,-1.58926923856624));
#41573=CARTESIAN_POINT('Ctrl Pts',(4.49940843053193,-1.32315190100328,-4.99898526062427));
#41574=CARTESIAN_POINT('Ctrl Pts',(4.6585083027966,3.49027724579729,-3.81556502166019));
#41575=CARTESIAN_POINT('Ctrl Pts',(4.81760817506126,5.09679560530872,0.873644852702682));
#41576=CARTESIAN_POINT('Ctrl Pts',(4.97670804732593,2.02031037891206,4.76013919238013));
#41577=CARTESIAN_POINT('Ctrl Pts',(5.1358079195906,-2.91246205836179,4.27295475701679));
#41578=CARTESIAN_POINT('Ctrl Pts',(5.29490779185526,-5.16922638901484,-0.140276351883654));
#41579=CARTESIAN_POINT('Ctrl Pts',(5.45400766411994,-2.67643755901513,-4.42461982427826));
#41580=CARTESIAN_POINT('Ctrl Pts',(5.6131075363846,2.27549715061658,-4.64356448598052));
#41581=CARTESIAN_POINT('Ctrl Pts',(5.77220740864928,5.13667525644702,-0.595941201221052));
#41582=CARTESIAN_POINT('Ctrl Pts',(5.93130728091394,3.27820871991814,3.9992406950588));
#41583=CARTESIAN_POINT('Ctrl Pts',(6.0904071531786,-1.5923189924077,4.91986775797726));
#41584=CARTESIAN_POINT('Ctrl Pts',(6.24950702544328,-4.99980312661834,1.32005577562594));
#41585=CARTESIAN_POINT('Ctrl Pts',(6.40860689770794,-3.81340254294399,-3.49264077619605));
#41586=CARTESIAN_POINT('Ctrl Pts',(6.56770676997262,0.876802331596175,-5.09625315459363));
#41587=CARTESIAN_POINT('Ctrl Pts',(6.72680664223727,4.76138972002301,-2.0173612671069));
#41588=CARTESIAN_POINT('Ctrl Pts',(6.88590651450195,4.27114975899821,2.91510862278235));
#41589=CARTESIAN_POINT('Ctrl Pts',(7.04500638676661,-0.143478642277096,
5.16913846066508));
#41590=CARTESIAN_POINT('Ctrl Pts',(7.20410625903128,-4.42627698454096,2.67369605656947));
#41591=CARTESIAN_POINT('Ctrl Pts',(7.36320613129595,-4.6421539560531,-2.27837336598945));
#41592=CARTESIAN_POINT('Ctrl Pts',(7.52230600356061,-0.59275896293977,-5.13704344525249));
#41593=CARTESIAN_POINT('Ctrl Pts',(7.68140587582529,4.00127074294363,-3.27573060374049));
#41594=CARTESIAN_POINT('Ctrl Pts',(7.84050574808995,4.91888038941839,1.59536649744721));
#41595=CARTESIAN_POINT('Ctrl Pts',(7.99960562035462,1.31695819333312,5.00061992792881));
#41596=CARTESIAN_POINT('Ctrl Pts',(8.15870549261929,-3.49500247063371,3.81123815535816));
#41597=CARTESIAN_POINT('Ctrl Pts',(8.31780536488395,-5.09570900655666,-0.879959241718225));
#41598=CARTESIAN_POINT('Ctrl Pts',(8.47690523714862,-2.01441124631645,-4.76263854153384));
#41599=CARTESIAN_POINT('Ctrl Pts',(8.63600510941329,2.91775399818566,-4.26934305867557));
#41600=CARTESIAN_POINT('Ctrl Pts',(8.79510498167796,5.16904858522312,0.146680844662566));
#41601=CARTESIAN_POINT('Ctrl Pts',(8.95420485394263,2.67095350892793,4.42793246332181));
#41602=CARTESIAN_POINT('Ctrl Pts',(9.1133047262073,-2.28124869702632,4.64074163565498));
#41603=CARTESIAN_POINT('Ctrl Pts',(9.27240459847195,-5.13740966782362,0.589576501850538));
#41604=CARTESIAN_POINT('Ctrl Pts',(9.43150447073664,-3.27325122773264,-4.00329925770802));
#41605=CARTESIAN_POINT('Ctrl Pts',(9.59060434300129,1.59841338882536,-4.91789113187562));
#41606=CARTESIAN_POINT('Ctrl Pts',(9.74970421526597,5.00143481089275,-1.31386010630501));
#41607=CARTESIAN_POINT('Ctrl Pts',(9.90880408753063,3.80907230476851,3.49736282416303));
#41608=CARTESIAN_POINT('Ctrl Pts',(10.0679039597953,-0.883115813962409,
5.09516290273885));
#41609=CARTESIAN_POINT('Ctrl Pts',(10.22700383206,-4.76388553535737,2.01146045261232));
#41610=CARTESIAN_POINT('Ctrl Pts',(10.3861037043246,-4.26753471994517,-2.92039825401031));
#41611=CARTESIAN_POINT('Ctrl Pts',(10.5452035765893,0.149882990889038,-5.1689567258239));
#41612=CARTESIAN_POINT('Ctrl Pts',(10.704303448854,4.42958624251035,-2.66820993668828));
#41613=CARTESIAN_POINT('Ctrl Pts',(10.8634033211187,4.63932753487269,2.28412315339565));
#41614=CARTESIAN_POINT('Ctrl Pts',(11.0225031933833,0.586393813370393,5.13777391729214));
#41615=CARTESIAN_POINT('Ctrl Pts',(11.181603065648,-4.00532623396138,3.27077059848325));
#41616=CARTESIAN_POINT('Ctrl Pts',(11.3407029379126,-4.91689999117348,-1.60145967239454));
#41617=CARTESIAN_POINT('Ctrl Pts',(11.4998028101773,-1.31076150706236,-5.00224776370858));
#41618=CARTESIAN_POINT('Ctrl Pts',(11.658902682442,3.49972182018105,-3.80690501300621));
#41619=CARTESIAN_POINT('Ctrl Pts',(11.8180025547066,5.09461487296727,0.886272086847998));
#41620=CARTESIAN_POINT('Ctrl Pts',(11.9771024269713,2.00850883058607,4.76513062511062));
#41621=CARTESIAN_POINT('Ctrl Pts',(12.136202299236,-2.92304128095414,4.26572488890354));
#41622=CARTESIAN_POINT('Ctrl Pts',(12.2953021715007,-5.16886309007812,-0.153085358464505));
#41623=CARTESIAN_POINT('Ctrl Pts',(12.4544020437653,-2.66546494290799,-4.43123778702695));
#41624=CARTESIAN_POINT('Ctrl Pts',(12.61350191603,2.28699597084696,-4.63791267903968));
#41625=CARTESIAN_POINT('Ctrl Pts',(12.7726017882947,5.13813765686258,-0.583208933669766));
#41626=CARTESIAN_POINT('Ctrl Pts',(12.9317016605593,3.2682859109503,4.00734790289743));
#41627=CARTESIAN_POINT('Ctrl Pts',(13.090801532824,-1.60449996642509,4.91591419297749));
#41628=CARTESIAN_POINT('Ctrl Pts',(13.2499014050887,-5.00306910342174,1.30764854213172));
#41629=CARTESIAN_POINT('Ctrl Pts',(13.4090012773533,-3.80471649711291,-3.50205289112016));
#41630=CARTESIAN_POINT('Ctrl Pts',(13.568101149618,0.889390123239341,-5.09411585972022));
#41631=CARTESIAN_POINT('Ctrl Pts',(13.7272010218827,4.7664465535393,-2.00545869799919));
#41632=CARTESIAN_POINT('Ctrl Pts',(13.8863008941473,4.26377407797028,2.92549576490892));
#41633=CARTESIAN_POINT('Ctrl Pts',(14.045400766412,-0.156020461739612,5.16912688108217));
#41634=CARTESIAN_POINT('Ctrl Pts',(14.2045006386767,-4.43340011533161,2.66202951501289));
#41635=CARTESIAN_POINT('Ctrl Pts',(14.3636005109413,-4.63551232968508,-2.28854382581323));
#41636=CARTESIAN_POINT('Ctrl Pts',(14.522700383206,-0.581919347715841,-5.1410577240212));
#41637=CARTESIAN_POINT('Ctrl Pts',(14.6818002554707,4.01308660375755,-3.2607181841902));
#41638=CARTESIAN_POINT('Ctrl Pts',(14.8143834823579,4.75806562994111,0.786704444467226));
#41639=CARTESIAN_POINT('Ctrl Pts',(14.9204500638677,3.11408383257965,3.31830903713004));
#41640=CARTESIAN_POINT('Ctrl Pts',(14.9734833546226,1.80781376844615,4.04682358287313));
#41641=CARTESIAN_POINT('Ctrl Pts',(15.,1.10295997362678,4.23058663740352));
#41642=CARTESIAN_POINT('Ctrl Pts',(2.22260689770794,-2.00237954638876,4.09906332620075));
#41643=CARTESIAN_POINT('Ctrl Pts',(2.24912354308539,-2.68532037429503,3.76544887910198));
#41644=CARTESIAN_POINT('Ctrl Pts',(2.30215683384027,-3.87080614621125,2.75038105804722));
#41645=CARTESIAN_POINT('Ctrl Pts',(2.40822341535006,-5.02907715778026,-0.178658710094689));
#41646=CARTESIAN_POINT('Ctrl Pts',(2.54080664223727,-3.43068896545911,-4.16436342244229));
#41647=CARTESIAN_POINT('Ctrl Pts',(2.69990651450196,1.65762077157099,-5.13796052424968));
#41648=CARTESIAN_POINT('Ctrl Pts',(2.8590063867666,5.21409784376103,-1.38273310829352));
#41649=CARTESIAN_POINT('Ctrl Pts',(3.01810625903129,3.98430482800797,3.63889215410996));
#41650=CARTESIAN_POINT('Ctrl Pts',(3.17720613129595,-0.908664557549035,
5.3191704066765));
#41651=CARTESIAN_POINT('Ctrl Pts',(3.33630600356062,-4.96551905943183,2.11102334806669));
#41652=CARTESIAN_POINT('Ctrl Pts',(3.49540587582528,-4.46062666336713,-3.03618522036417));
#41653=CARTESIAN_POINT('Ctrl Pts',(3.65450574808995,0.143080314496841,-5.39400653083915));
#41654=CARTESIAN_POINT('Ctrl Pts',(3.81360562035462,4.61514993964848,-2.79558764496926));
#41655=CARTESIAN_POINT('Ctrl Pts',(3.97270549261929,4.84684961235789,2.3713723801698));
#41656=CARTESIAN_POINT('Ctrl Pts',(4.13180536488395,0.625153138376691,5.35952683456545));
#41657=CARTESIAN_POINT('Ctrl Pts',(4.29090523714863,-4.17091766469395,3.42325555365425));
#41658=CARTESIAN_POINT('Ctrl Pts',(4.45000510941329,-5.13470740781455,-1.65833629147738));
#41659=CARTESIAN_POINT('Ctrl Pts',(4.60910498167796,-1.38065392780811,-5.2162330189771));
#41660=CARTESIAN_POINT('Ctrl Pts',(4.76820485394262,3.64195901082506,-3.98138326368112));
#41661=CARTESIAN_POINT('Ctrl Pts',(4.92730472620729,5.31829404195296,0.911612035230917));
#41662=CARTESIAN_POINT('Ctrl Pts',(5.08640459847196,2.10810977781265,4.96700708957871));
#41663=CARTESIAN_POINT('Ctrl Pts',(5.24550447073663,-3.03903291634182,4.45865041205641));
#41664=CARTESIAN_POINT('Ctrl Pts',(5.4046043430013,-5.39387254956214,-0.146372533690109));
#41665=CARTESIAN_POINT('Ctrl Pts',(5.56370421526596,-2.79275117663017,-4.61690659614762));
#41666=CARTESIAN_POINT('Ctrl Pts',(5.72280408753063,2.3743865510322,-4.84536623628618));
#41667=CARTESIAN_POINT('Ctrl Pts',(5.8819039597953,5.35990679778392,-0.621839835308898));
#41668=CARTESIAN_POINT('Ctrl Pts',(6.04100383205997,3.42067433217443,4.17304118272146));
#41669=CARTESIAN_POINT('Ctrl Pts',(6.20010370432463,-1.66151858265413,5.1336771985115));
#41670=CARTESIAN_POINT('Ctrl Pts',(6.35920357658931,-5.21708642809535,1.37742324986404));
#41671=CARTESIAN_POINT('Ctrl Pts',(6.51830344885397,-3.9791268071616,-3.64442525640584));
#41672=CARTESIAN_POINT('Ctrl Pts',(6.67740332111864,0.914906733015021,-5.31772801721321));
#41673=CARTESIAN_POINT('Ctrl Pts',(6.83650319338331,4.96831196311641,-2.1050325024112));
#41674=CARTESIAN_POINT('Ctrl Pts',(6.99560306564798,4.45676697176347,3.04179449614205));
#41675=CARTESIAN_POINT('Ctrl Pts',(7.15470293791264,-0.149713990408975,
5.3937807999895));
#41676=CARTESIAN_POINT('Ctrl Pts',(7.31380281017731,-4.61863577389657,2.78989053295287));
#41677=CARTESIAN_POINT('Ctrl Pts',(7.47290268244198,-4.84389440702522,-2.37738776204113));
#41678=CARTESIAN_POINT('Ctrl Pts',(7.63200255470664,-0.618519302134332,
-5.36029098747527));
#41679=CARTESIAN_POINT('Ctrl Pts',(7.79110242697132,4.17515945318134,-3.41808852110343));
#41680=CARTESIAN_POINT('Ctrl Pts',(7.95020229923597,5.13264692052304,1.66469852729966));
#41681=CARTESIAN_POINT('Ctrl Pts',(8.10930217150066,1.37419105168933,5.21793872626056));
#41682=CARTESIAN_POINT('Ctrl Pts',(8.26840204376531,-3.64688958623763,3.9768683588161));
#41683=CARTESIAN_POINT('Ctrl Pts',(8.42750191602999,-5.31716022138873,-0.91820083730981));
#41684=CARTESIAN_POINT('Ctrl Pts',(8.58660178829464,-2.10195427852144,-4.96961505637633));
#41685=CARTESIAN_POINT('Ctrl Pts',(8.74570166055932,3.04455483525227,-4.4548817551871));
#41686=CARTESIAN_POINT('Ctrl Pts',(8.90480153282398,5.39368701870719,0.153055355295186));
#41687=CARTESIAN_POINT('Ctrl Pts',(9.06390140508865,2.7870287986572,4.62036319708922));
#41688=CARTESIAN_POINT('Ctrl Pts',(9.22300127735332,-2.38038805028225,4.84242070948262));
#41689=CARTESIAN_POINT('Ctrl Pts',(9.38210114961799,-5.36067312548293,0.615198536468943));
#41690=CARTESIAN_POINT('Ctrl Pts',(9.54120102188265,-3.41550139545205,-4.17727612389385));
#41691=CARTESIAN_POINT('Ctrl Pts',(9.70030089414733,1.6678778316151,-5.13161467145851));
#41692=CARTESIAN_POINT('Ctrl Pts',(9.85940076641199,5.21878902271104,-1.37095832684435));
#41693=CARTESIAN_POINT('Ctrl Pts',(10.0185006386767,3.97460838388701,3.64935251688739));
#41694=CARTESIAN_POINT('Ctrl Pts',(10.1776005109413,-0.921494589043101,
5.31659038478835));
#41695=CARTESIAN_POINT('Ctrl Pts',(10.336700383206,-4.97091624252066,2.09887524812842));
#41696=CARTESIAN_POINT('Ctrl Pts',(10.4958002554707,-4.45299482900043,-3.04731400612877));
#41697=CARTESIAN_POINT('Ctrl Pts',(10.6549001277353,0.156396661581818,-5.39359116724809));
#41698=CARTESIAN_POINT('Ctrl Pts',(10.814,4.62208884682804,-2.78416599523604));
#41699=CARTESIAN_POINT('Ctrl Pts',(10.9730998722647,4.84094515418326,2.38338742584421));
#41700=CARTESIAN_POINT('Ctrl Pts',(11.1321997445293,0.611877533530606,5.36105320464015));
#41701=CARTESIAN_POINT('Ctrl Pts',(11.291299616794,-4.17939118923417,3.4129129620953));
#41702=CARTESIAN_POINT('Ctrl Pts',(11.4503994890587,-5.13058045739557,-1.67105650170719));
#41703=CARTESIAN_POINT('Ctrl Pts',(11.6094993613233,-1.36772506752482,-5.21963730513232));
#41704=CARTESIAN_POINT('Ctrl Pts',(11.768599233588,3.65181403103062,-3.97234690515425));
#41705=CARTESIAN_POINT('Ctrl Pts',(11.9276991058527,5.31601853853538,0.924788028408167));
#41706=CARTESIAN_POINT('Ctrl Pts',(12.0867989781174,2.09579535341577,4.9722154418469));
#41707=CARTESIAN_POINT('Ctrl Pts',(12.245898850382,-3.05007189471929,4.45110634564912));
#41708=CARTESIAN_POINT('Ctrl Pts',(12.4049987226467,-5.39349346224528,-0.159738198836918));
#41709=CARTESIAN_POINT('Ctrl Pts',(12.5640985949113,-2.78130170849642,-4.62381216477972));
#41710=CARTESIAN_POINT('Ctrl Pts',(12.723198467176,2.38638509126345,-4.83946881101991));
#41711=CARTESIAN_POINT('Ctrl Pts',(12.8822983394407,5.36143275173995,-0.608554244144905));
#41712=CARTESIAN_POINT('Ctrl Pts',(13.0413982117054,3.41032029408859,4.18150071660979));
#41713=CARTESIAN_POINT('Ctrl Pts',(13.20049808397,-1.67422892196505,5.1295518180154));
#41714=CARTESIAN_POINT('Ctrl Pts',(13.3595979562347,-5.22049433893182,1.36447681820791));
#41715=CARTESIAN_POINT('Ctrl Pts',(13.5186978284993,-3.97006327992432,-3.6542464065165));
#41716=CARTESIAN_POINT('Ctrl Pts',(13.677797700764,0.928041569583217,-5.31549783898529));
#41717=CARTESIAN_POINT('Ctrl Pts',(13.8368975730287,4.97358855838203,-2.09261266703394));
#41718=CARTESIAN_POINT('Ctrl Pts',(13.9959974452933,4.4490707556497,3.05263304654951));
#41719=CARTESIAN_POINT('Ctrl Pts',(14.155097317558,-0.162800856920419,5.39376871717677));
#41720=CARTESIAN_POINT('Ctrl Pts',(14.3141971898227,-4.62606846435103,2.77771698249975));
#41721=CARTESIAN_POINT('Ctrl Pts',(14.4732970620874,-4.83696414639145,-2.3880002134858));
#41722=CARTESIAN_POINT('Ctrl Pts',(14.632396934352,-0.607208614885573,-5.36447972026183));
#41723=CARTESIAN_POINT('Ctrl Pts',(14.7914968066167,4.18748881206356,-3.40242368624789));
#41724=CARTESIAN_POINT('Ctrl Pts',(14.9240800335039,4.96484341349299,0.820893338439942));
#41725=CARTESIAN_POINT('Ctrl Pts',(15.0301466150137,3.24941684451702,3.46251734386715));
#41726=CARTESIAN_POINT('Ctrl Pts',(15.0831799057686,1.88637841071624,4.22269194534932));
#41727=CARTESIAN_POINT('Ctrl Pts',(15.109696551146,1.15089281786034,4.41444104296314));
#41728=CARTESIAN_POINT('Ctrl Pts',(2.33230344885397,-2.08577545033743,4.26978275451687));
#41729=CARTESIAN_POINT('Ctrl Pts',(2.35882009423142,-2.7971596709009,3.92227379953806));
#41730=CARTESIAN_POINT('Ctrl Pts',(2.4118533849863,-4.03201902823232,2.8649300280229));
#41731=CARTESIAN_POINT('Ctrl Pts',(2.51791996649609,-5.23853017399645,-0.186099559484853));
#41732=CARTESIAN_POINT('Ctrl Pts',(2.6505031933833,-3.57357167116653,-4.33780249527526));
#41733=CARTESIAN_POINT('Ctrl Pts',(2.80960306564798,1.72665802422299,-5.35194835844684));
#41734=CARTESIAN_POINT('Ctrl Pts',(2.96870293791264,5.43125667548277,-1.44032172963851));
#41735=CARTESIAN_POINT('Ctrl Pts',(3.12780281017732,4.15024474850808,3.79044618946306));
#41736=CARTESIAN_POINT('Ctrl Pts',(3.28690268244198,-0.946508982348298,
5.54070534250915));
#41737=CARTESIAN_POINT('Ctrl Pts',(3.44600255470665,-5.1723249825559,2.19894409250613));
#41738=CARTESIAN_POINT('Ctrl Pts',(3.60510242697131,-4.6464046261115,-3.16263747636354));
#41739=CARTESIAN_POINT('Ctrl Pts',(3.76420229923598,0.149039380642027,-5.61865827149225));
#41740=CARTESIAN_POINT('Ctrl Pts',(3.92330217150065,4.80736354958561,-2.91201939695178));
#41741=CARTESIAN_POINT('Ctrl Pts',(4.08240204376532,5.04871314290327,2.4701362451922));
#41742=CARTESIAN_POINT('Ctrl Pts',(4.24150191602998,0.651189766235444,5.58274255104231));
#41743=CARTESIAN_POINT('Ctrl Pts',(4.40060178829465,-4.34462971122875,3.56582866965477));
#41744=CARTESIAN_POINT('Ctrl Pts',(4.55970166055932,-5.34855975491775,-1.72740334438853));
#41745=CARTESIAN_POINT('Ctrl Pts',(4.71880153282399,-1.43815595461293,-5.43348077732993));
#41746=CARTESIAN_POINT('Ctrl Pts',(4.87790140508865,3.79364077585284,-4.14720150570204));
#41747=CARTESIAN_POINT('Ctrl Pts',(5.03700127735333,5.53979247859722,0.949579217759153));
#41748=CARTESIAN_POINT('Ctrl Pts',(5.19610114961799,2.19590917671323,5.17387498677729));
#41749=CARTESIAN_POINT('Ctrl Pts',(5.35520102188265,-3.16560377432185,4.64434606709603));
#41750=CARTESIAN_POINT('Ctrl Pts',(5.51430089414734,-5.61851871010945,-0.152468715496564));
#41751=CARTESIAN_POINT('Ctrl Pts',(5.67340076641199,-2.9090647942452,-4.80919336801698));
#41752=CARTESIAN_POINT('Ctrl Pts',(5.83250063867666,2.47327595144782,-5.04716798659183));
#41753=CARTESIAN_POINT('Ctrl Pts',(5.99160051094134,5.58313833912081,-0.647738469396749));
#41754=CARTESIAN_POINT('Ctrl Pts',(6.15070038320599,3.56313994443072,4.34684167038412));
#41755=CARTESIAN_POINT('Ctrl Pts',(6.30980025547067,-1.73071817290056,5.34748663904573));
#41756=CARTESIAN_POINT('Ctrl Pts',(6.46890012773532,-5.43436972957236,1.43479072410215));
#41757=CARTESIAN_POINT('Ctrl Pts',(6.62800000000001,-4.14485107137922,-3.79620973661563));
#41758=CARTESIAN_POINT('Ctrl Pts',(6.78709987226466,0.953011134433869,-5.53920287983279));
#41759=CARTESIAN_POINT('Ctrl Pts',(6.94619974452934,5.17523420620982,-2.19270373771549));
#41760=CARTESIAN_POINT('Ctrl Pts',(7.10529961679399,4.64238418452872,3.16848036950175));
#41761=CARTESIAN_POINT('Ctrl Pts',(7.26439948905868,-0.155949338540855,
5.61842313931392));
#41762=CARTESIAN_POINT('Ctrl Pts',(7.42349936132333,-4.81099456325219,2.90608500933629));
#41763=CARTESIAN_POINT('Ctrl Pts',(7.58259923358801,-5.04563485799734,-2.47640215809281));
#41764=CARTESIAN_POINT('Ctrl Pts',(7.74169910585267,-0.644279641328896,
-5.58353852969804));
#41765=CARTESIAN_POINT('Ctrl Pts',(7.90079897811735,4.34904816341905,-3.56044643846636));
#41766=CARTESIAN_POINT('Ctrl Pts',(8.05989885038201,5.34641345162768,1.73403055715211));
#41767=CARTESIAN_POINT('Ctrl Pts',(8.21899872264668,1.43142391004554,5.43525752459233));
#41768=CARTESIAN_POINT('Ctrl Pts',(8.37809859491134,-3.79877670184155,4.14249856227404));
#41769=CARTESIAN_POINT('Ctrl Pts',(8.53719846717601,-5.53861143622079,-0.95644243290139));
#41770=CARTESIAN_POINT('Ctrl Pts',(8.69629833944068,-2.18949731072642,-5.17659157121883));
#41771=CARTESIAN_POINT('Ctrl Pts',(8.85539821170535,3.17135567231888,-4.64042045169863));
#41772=CARTESIAN_POINT('Ctrl Pts',(9.01449808397001,5.61832545219127,0.159429865927808));
#41773=CARTESIAN_POINT('Ctrl Pts',(9.17359795623469,2.90310408838647,4.81279393085663));
#41774=CARTESIAN_POINT('Ctrl Pts',(9.33269782849934,-2.47952740353819,5.04409978331027));
#41775=CARTESIAN_POINT('Ctrl Pts',(9.49179770076403,-5.58393658314223,0.640820571087352));
#41776=CARTESIAN_POINT('Ctrl Pts',(9.65089757302868,-3.55775156317145,-4.35125299007969));
#41777=CARTESIAN_POINT('Ctrl Pts',(9.80999744529336,1.73734227440484,-5.34533821104139));
#41778=CARTESIAN_POINT('Ctrl Pts',(9.96909731755802,5.43614323452935,-1.42805654738371));
#41779=CARTESIAN_POINT('Ctrl Pts',(10.1281971898227,4.1401444630055,3.80134220961176));
#41780=CARTESIAN_POINT('Ctrl Pts',(10.2872970620874,-0.959873364123795,
5.53801786683784));
#41781=CARTESIAN_POINT('Ctrl Pts',(10.446396934352,-5.17794694968394,2.18629004364453));
#41782=CARTESIAN_POINT('Ctrl Pts',(10.6054968066167,-4.6384549380557,-3.17422975824723));
#41783=CARTESIAN_POINT('Ctrl Pts',(10.7645966788814,0.162910332274605,-5.61822560867227));
#41784=CARTESIAN_POINT('Ctrl Pts',(10.923696551146,4.81459145114573,-2.90012205378381));
#41785=CARTESIAN_POINT('Ctrl Pts',(11.0827964234107,5.04256277349384,2.48265169829277));
#41786=CARTESIAN_POINT('Ctrl Pts',(11.2418962956754,0.637361253690814,5.58433249198815));
#41787=CARTESIAN_POINT('Ctrl Pts',(11.40099616794,-4.35345614450695,3.55505532570735));
#41788=CARTESIAN_POINT('Ctrl Pts',(11.5600960402047,-5.34426092361766,-1.74065333101984));
#41789=CARTESIAN_POINT('Ctrl Pts',(11.7191959124694,-1.42468862798729,-5.43702684655607));
#41790=CARTESIAN_POINT('Ctrl Pts',(11.878295784734,3.8039062418802,-4.13778879730229));
#41791=CARTESIAN_POINT('Ctrl Pts',(12.0373956569987,5.53742220410349,0.963303969968333));
#41792=CARTESIAN_POINT('Ctrl Pts',(12.1964955292634,2.18308187624546,5.17930025858317));
#41793=CARTESIAN_POINT('Ctrl Pts',(12.355595401528,-3.17710250848444,4.63648780239471));
#41794=CARTESIAN_POINT('Ctrl Pts',(12.5146952737927,-5.61812383441245,-0.166391039209329));
#41795=CARTESIAN_POINT('Ctrl Pts',(12.6737951460574,-2.89713847408484,-4.81638654253248));
#41796=CARTESIAN_POINT('Ctrl Pts',(12.832895018322,2.48577421167993,-5.04102494300014));
#41797=CARTESIAN_POINT('Ctrl Pts',(12.9919948905867,5.58472784661733,-0.63389955462005));
#41798=CARTESIAN_POINT('Ctrl Pts',(13.1510947628514,3.55235467722688,4.35565353032216));
#41799=CARTESIAN_POINT('Ctrl Pts',(13.3101946351161,-1.74395787750501,5.34318944305331));
#41800=CARTESIAN_POINT('Ctrl Pts',(13.4692945073807,-5.43791957444192,1.4213050942841));
#41801=CARTESIAN_POINT('Ctrl Pts',(13.6283943796454,-4.13541006273573,-3.80643992191284));
#41802=CARTESIAN_POINT('Ctrl Pts',(13.7874942519101,0.966693015927084,-5.53687981825035));
#41803=CARTESIAN_POINT('Ctrl Pts',(13.9465941241747,5.18073056322477,-2.17976663606868));
#41804=CARTESIAN_POINT('Ctrl Pts',(14.1056939964394,4.63436743332911,3.17977032819009));
#41805=CARTESIAN_POINT('Ctrl Pts',(14.264793868704,-0.169581252101216,5.61841055327138));
#41806=CARTESIAN_POINT('Ctrl Pts',(14.4238937409687,-4.81873681337047,2.89340444998659));
#41807=CARTESIAN_POINT('Ctrl Pts',(14.5829936132334,-5.0384159630978,-2.48745660115836));
#41808=CARTESIAN_POINT('Ctrl Pts',(14.7420934854981,-0.63249788205531,-5.58790171650246));
#41809=CARTESIAN_POINT('Ctrl Pts',(14.9011933577627,4.36189102036958,-3.54412918830557));
#41810=CARTESIAN_POINT('Ctrl Pts',(15.0337765846499,5.17162119704487,0.855082232412658));
#41811=CARTESIAN_POINT('Ctrl Pts',(15.1398431661597,3.38474985645439,3.60672565060427));
#41812=CARTESIAN_POINT('Ctrl Pts',(15.1928764569146,1.96494305298632,4.3985603078255));
#41813=CARTESIAN_POINT('Ctrl Pts',(15.2193931022921,1.19882566209391,4.59829544852276));
#41814=CARTESIAN_POINT('Ctrl Pts',(2.442,-2.16917135428609,4.440502182833));
#41815=CARTESIAN_POINT('Ctrl Pts',(2.46851664537744,-2.90899896750678,4.07909871997414));
#41816=CARTESIAN_POINT('Ctrl Pts',(2.52154993613233,-4.19323191025339,2.97947899799857));
#41817=CARTESIAN_POINT('Ctrl Pts',(2.62761651764211,-5.44798319021263,-0.193540408875019));
#41818=CARTESIAN_POINT('Ctrl Pts',(2.76019974452933,-3.71645437687396,-4.51124156810822));
#41819=CARTESIAN_POINT('Ctrl Pts',(2.919299616794,1.795695276875,-5.565936192644));
#41820=CARTESIAN_POINT('Ctrl Pts',(3.07839948905867,5.64841550720451,-1.4979103509835));
#41821=CARTESIAN_POINT('Ctrl Pts',(3.23749936132334,4.31618466900822,3.94200022481617));
#41822=CARTESIAN_POINT('Ctrl Pts',(3.39659923358801,-0.984353407147573,
5.7622402783418));
#41823=CARTESIAN_POINT('Ctrl Pts',(3.55569910585267,-5.37913090567997,2.28686483694558));
#41824=CARTESIAN_POINT('Ctrl Pts',(3.71479897811734,-4.83218258885587,-3.28908973236292));
#41825=CARTESIAN_POINT('Ctrl Pts',(3.87389885038201,0.154998446787216,-5.84331001214534));
#41826=CARTESIAN_POINT('Ctrl Pts',(4.03299872264668,4.99957715952273,-3.02845114893429));
#41827=CARTESIAN_POINT('Ctrl Pts',(4.19209859491135,5.25057667344865,2.5689001102146));
#41828=CARTESIAN_POINT('Ctrl Pts',(4.35119846717601,0.677226394094196,5.80595826751917));
#41829=CARTESIAN_POINT('Ctrl Pts',(4.51029833944069,-4.51834175776356,3.70840178565529));
#41830=CARTESIAN_POINT('Ctrl Pts',(4.66939821170534,-5.56241210202095,-1.79647039729968));
#41831=CARTESIAN_POINT('Ctrl Pts',(4.82849808397002,-1.49565798141775,-5.65072853568276));
#41832=CARTESIAN_POINT('Ctrl Pts',(4.98759795623469,3.94532254088061,-4.31301974772297));
#41833=CARTESIAN_POINT('Ctrl Pts',(5.14669782849935,5.76129091524147,0.987546400287391));
#41834=CARTESIAN_POINT('Ctrl Pts',(5.30579770076402,2.28370857561381,5.38074288397587));
#41835=CARTESIAN_POINT('Ctrl Pts',(5.46489757302869,-3.29217463230187,4.83004172213565));
#41836=CARTESIAN_POINT('Ctrl Pts',(5.62399744529335,-5.84316487065676,-0.158564897303022));
#41837=CARTESIAN_POINT('Ctrl Pts',(5.78309731755803,-3.02537841186024,-5.00148013988634));
#41838=CARTESIAN_POINT('Ctrl Pts',(5.94219718982269,2.57216535186344,-5.24896973689749));
#41839=CARTESIAN_POINT('Ctrl Pts',(6.10129706208736,5.80636988045771,-0.67363710348459));
#41840=CARTESIAN_POINT('Ctrl Pts',(6.26039693435203,3.70560555668701,4.52064215804677));
#41841=CARTESIAN_POINT('Ctrl Pts',(6.41949680661669,-1.79991776314699,5.56129607957998));
#41842=CARTESIAN_POINT('Ctrl Pts',(6.57859667888136,-5.65165303104936,1.49215819834025));
#41843=CARTESIAN_POINT('Ctrl Pts',(6.73769655114604,-4.31057533559683,-3.94799421682542));
#41844=CARTESIAN_POINT('Ctrl Pts',(6.89679642341068,0.991115535852721,-5.76067774245237));
#41845=CARTESIAN_POINT('Ctrl Pts',(7.05589629567538,5.38215644930322,-2.28037497301978));
#41846=CARTESIAN_POINT('Ctrl Pts',(7.21499616794003,4.82800139729398,3.29516624286144));
#41847=CARTESIAN_POINT('Ctrl Pts',(7.3740960402047,-0.162184686672736,5.84306547863835));
#41848=CARTESIAN_POINT('Ctrl Pts',(7.53319591246937,-5.0033533526078,3.02227948571969));
#41849=CARTESIAN_POINT('Ctrl Pts',(7.69229578473404,-5.24737530896947,-2.57541655414449));
#41850=CARTESIAN_POINT('Ctrl Pts',(7.8513956569987,-0.670039980523453,-5.80678607192081));
#41851=CARTESIAN_POINT('Ctrl Pts',(8.01049552926337,4.52293687365675,-3.7028043558293));
#41852=CARTESIAN_POINT('Ctrl Pts',(8.16959540152804,5.56017998273234,1.80336258700456));
#41853=CARTESIAN_POINT('Ctrl Pts',(8.32869527379271,1.48865676840175,5.65257632292408));
#41854=CARTESIAN_POINT('Ctrl Pts',(8.48779514605737,-3.95066381744548,4.30812876573197));
#41855=CARTESIAN_POINT('Ctrl Pts',(8.64689501832204,-5.76006265105285,-0.994684028492972));
#41856=CARTESIAN_POINT('Ctrl Pts',(8.80599489058671,-2.27704034293141,-5.38356808606133));
#41857=CARTESIAN_POINT('Ctrl Pts',(8.96509476285137,3.2981565093855,-4.82595914821016));
#41858=CARTESIAN_POINT('Ctrl Pts',(9.12419463511605,5.84296388567535,0.165804376560428));
#41859=CARTESIAN_POINT('Ctrl Pts',(9.2832945073807,3.01917937811574,5.00522466462404));
#41860=CARTESIAN_POINT('Ctrl Pts',(9.44239437964538,-2.57866675679413,5.24577885713792));
#41861=CARTESIAN_POINT('Ctrl Pts',(9.60149425191005,-5.80720004080153,0.666442605705756));
#41862=CARTESIAN_POINT('Ctrl Pts',(9.7605941241747,-3.70000173089087,-4.52522985626553));
#41863=CARTESIAN_POINT('Ctrl Pts',(9.9196939964394,1.80680671719459,-5.55906175062428));
#41864=CARTESIAN_POINT('Ctrl Pts',(10.078793868704,5.65349744634764,-1.48515476792305));
#41865=CARTESIAN_POINT('Ctrl Pts',(10.2378937409687,4.305680542124,3.95333190233613));
#41866=CARTESIAN_POINT('Ctrl Pts',(10.3969936132334,-0.998252139204486,
5.75944534888733));
#41867=CARTESIAN_POINT('Ctrl Pts',(10.5560934854981,-5.38497765684723,2.27370483916063));
#41868=CARTESIAN_POINT('Ctrl Pts',(10.7151933577627,-4.82391504711097,-3.30114551036569));
#41869=CARTESIAN_POINT('Ctrl Pts',(10.8742932300274,0.169424002967387,-5.84286005009646));
#41870=CARTESIAN_POINT('Ctrl Pts',(11.033393102292,5.00709405546342,-3.01607811233158));
#41871=CARTESIAN_POINT('Ctrl Pts',(11.1924929745567,5.24418039280442,2.58191597074134));
#41872=CARTESIAN_POINT('Ctrl Pts',(11.3515928468214,0.662844973851022,5.80761177933616));
#41873=CARTESIAN_POINT('Ctrl Pts',(11.5106927190861,-4.52752109977973,3.6971976893194));
#41874=CARTESIAN_POINT('Ctrl Pts',(11.6697925913507,-5.55794138983975,-1.81025016033249));
#41875=CARTESIAN_POINT('Ctrl Pts',(11.8288924636154,-1.48165218844976,-5.65441638797981));
#41876=CARTESIAN_POINT('Ctrl Pts',(11.9879923358801,3.95599845272978,-4.30323068945033));
#41877=CARTESIAN_POINT('Ctrl Pts',(12.1470922081447,5.75882586967161,1.0018199115285));
#41878=CARTESIAN_POINT('Ctrl Pts',(12.3061920804094,2.27036839907515,5.38638507531945));
#41879=CARTESIAN_POINT('Ctrl Pts',(12.4652919526741,-3.30413312224959,4.8218692591403));
#41880=CARTESIAN_POINT('Ctrl Pts',(12.6243918249387,-5.84275420657962,-0.173043879581744));
#41881=CARTESIAN_POINT('Ctrl Pts',(12.7834916972034,-3.01297523967326,-5.00896092028525));
#41882=CARTESIAN_POINT('Ctrl Pts',(12.9425915694681,2.58516333209641,-5.24258107498037));
#41883=CARTESIAN_POINT('Ctrl Pts',(13.1016914417327,5.80802294149471,-0.659244865095191));
#41884=CARTESIAN_POINT('Ctrl Pts',(13.2607913139974,3.69438906036517,4.52980634403453));
#41885=CARTESIAN_POINT('Ctrl Pts',(13.4198911862621,-1.81368683304497,5.55682706809122));
#41886=CARTESIAN_POINT('Ctrl Pts',(13.5789910585268,-5.655344809952,1.47813337036028));
#41887=CARTESIAN_POINT('Ctrl Pts',(13.7380909307914,-4.30075684554715,-3.95863343730917));
#41888=CARTESIAN_POINT('Ctrl Pts',(13.8971908030561,1.00534446227096,-5.75826179751541));
#41889=CARTESIAN_POINT('Ctrl Pts',(14.0562906753207,5.38787256806751,-2.26692060510343));
#41890=CARTESIAN_POINT('Ctrl Pts',(14.2153905475854,4.81966411100853,3.30690760983067));
#41891=CARTESIAN_POINT('Ctrl Pts',(14.3744904198501,-0.176361647282018,
5.84305238936599));
#41892=CARTESIAN_POINT('Ctrl Pts',(14.5335902921148,-5.01140516238991,3.00909191747344));
#41893=CARTESIAN_POINT('Ctrl Pts',(14.6926901643794,-5.23986777980416,-2.58691298883092));
#41894=CARTESIAN_POINT('Ctrl Pts',(14.8517900366441,-0.657787149225042,
-5.81132371274309));
#41895=CARTESIAN_POINT('Ctrl Pts',(15.0108899089088,4.53629322867559,-3.68583469036325));
#41896=CARTESIAN_POINT('Ctrl Pts',(15.143473135796,5.37839898059675,0.889271126385368));
#41897=CARTESIAN_POINT('Ctrl Pts',(15.2495397173057,3.52008286839176,3.75093395734139));
#41898=CARTESIAN_POINT('Ctrl Pts',(15.3025730080606,2.04350769525641,4.57442867030168));
#41899=CARTESIAN_POINT('Ctrl Pts',(15.3290896534381,1.24675850632747,4.78214985408238));
#41900=CARTESIAN_POINT('',(15.,3.61714728420828,-3.37770697643486));
#41901=CARTESIAN_POINT('Ctrl Pts',(15.,3.61714728420828,-3.37770697643486));
#41902=CARTESIAN_POINT('Ctrl Pts',(15.,3.68957840109089,-3.29192253111056));
#41903=CARTESIAN_POINT('Ctrl Pts',(15.,3.75871853092304,-3.20370683073969));
#41904=CARTESIAN_POINT('Ctrl Pts',(15.,3.82438207257458,-3.11313443623491));
#41905=CARTESIAN_POINT('Ctrl Pts',(15.,3.90791289962552,-2.99791696805269));
#41906=CARTESIAN_POINT('Ctrl Pts',(15.,3.98581952259522,-2.87888650317557));
#41907=CARTESIAN_POINT('Ctrl Pts',(15.,4.05811156137618,-2.75649539075295));
#41908=CARTESIAN_POINT('Ctrl Pts',(15.,4.13173944465282,-2.63184268083483));
#41909=CARTESIAN_POINT('Ctrl Pts',(15.,4.19954353035942,-2.50370321513495));
#41910=CARTESIAN_POINT('Ctrl Pts',(15.,4.26148524515888,-2.37253157027713));
#41911=CARTESIAN_POINT('Ctrl Pts',(15.,4.32381499703478,-2.24053819386494));
#41912=CARTESIAN_POINT('Ctrl Pts',(15.,4.38020882026663,-2.10547368153064));
#41913=CARTESIAN_POINT('Ctrl Pts',(15.,4.43057619978867,-1.96779009730298));
#41914=CARTESIAN_POINT('Ctrl Pts',(15.,4.45655213569676,-1.8967826318872));
#41915=CARTESIAN_POINT('Ctrl Pts',(15.,4.48092433553813,-1.8250784529312));
#41916=CARTESIAN_POINT('Ctrl Pts',(15.,4.50367494257293,-1.75273956196209));
#41917=CARTESIAN_POINT('Ctrl Pts',(15.,4.51067738059232,-1.730474283518));
#41918=CARTESIAN_POINT('Ctrl Pts',(15.,4.51752691038149,-1.70814614040682));
#41919=CARTESIAN_POINT('Ctrl Pts',(15.,4.52421615574277,-1.68578041462856));
#41920=CARTESIAN_POINT('Ctrl Pts',(15.,4.56556142875004,-1.54754104854681));
#41921=CARTESIAN_POINT('Ctrl Pts',(15.,4.6008467478143,-1.40768448094355));
#41922=CARTESIAN_POINT('Ctrl Pts',(15.,4.63006598166419,-1.26666139036611));
#41923=CARTESIAN_POINT('Ctrl Pts',(15.,4.65937480607125,-1.1252059018236));
#41924=CARTESIAN_POINT('Ctrl Pts',(15.,4.68258035315745,-0.982575874006902));
#41925=CARTESIAN_POINT('Ctrl Pts',(15.,4.69962490113214,-0.83921597561456));
#41926=CARTESIAN_POINT('Ctrl Pts',(15.,4.71652107743951,-0.697104015694111));
#41927=CARTESIAN_POINT('Ctrl Pts',(15.,4.72736302542697,-0.554274021959568));
#41928=CARTESIAN_POINT('Ctrl Pts',(15.,4.73204381389164,-0.41116162127756));
#41929=CARTESIAN_POINT('Ctrl Pts',(15.,4.73664109518138,-0.270602404181739));
#41930=CARTESIAN_POINT('Ctrl Pts',(15.,4.73529500312457,-0.129770054420742));
#41931=CARTESIAN_POINT('Ctrl Pts',(15.,4.72785605002238,0.010909094154732));
#41932=CARTESIAN_POINT('Ctrl Pts',(15.,4.72644560501024,0.037582229566991));
#41933=CARTESIAN_POINT('Ctrl Pts',(15.,4.72481598741633,0.0642497999003566));
#41934=CARTESIAN_POINT('Ctrl Pts',(15.,4.72296598198155,0.0909088105373209));
#41935=CARTESIAN_POINT('Ctrl Pts',(15.,4.72160216103772,0.110561789044773));
#41936=CARTESIAN_POINT('Ctrl Pts',(15.,4.72011835426907,0.130212130596743));
#41937=CARTESIAN_POINT('Ctrl Pts',(15.,4.71851563947719,0.149840943089536));
#41938=CARTESIAN_POINT('Ctrl Pts',(15.,4.70701478457874,0.290694528176004));
#41939=CARTESIAN_POINT('Ctrl Pts',(15.,4.68938349296752,0.430628932810751));
#41940=CARTESIAN_POINT('Ctrl Pts',(15.,4.66556557715506,0.569230026091733));
#41941=CARTESIAN_POINT('Ctrl Pts',(15.,4.64202084297191,0.706241422239518));
#41942=CARTESIAN_POINT('Ctrl Pts',(15.,4.61243051523659,0.841950655426112));
#41943=CARTESIAN_POINT('Ctrl Pts',(15.,4.57669086926763,0.975947063455624));
#41944=CARTESIAN_POINT('Ctrl Pts',(15.,4.54180219894916,1.10675296197131));
#41945=CARTESIAN_POINT('Ctrl Pts',(15.,4.50105340728844,1.23592722645281));
#41946=CARTESIAN_POINT('Ctrl Pts',(15.,4.45430240519226,1.36306795813444));
#41947=CARTESIAN_POINT('Ctrl Pts',(15.,4.44403793093735,1.39098249918347));
#41948=CARTESIAN_POINT('Ctrl Pts',(15.,4.43348394709866,1.41879891703032));
#41949=CARTESIAN_POINT('Ctrl Pts',(15.,4.42263865647625,1.44651278257324));
#41950=CARTESIAN_POINT('Ctrl Pts',(15.,4.38789959528659,1.53528437057554));
#41951=CARTESIAN_POINT('Ctrl Pts',(15.,4.35017225985734,1.62300434398871));
#41952=CARTESIAN_POINT('Ctrl Pts',(15.,4.30955405365424,1.70955383489484));
#41953=CARTESIAN_POINT('Ctrl Pts',(15.,4.28785544355993,1.75578934927581));
#41954=CARTESIAN_POINT('Ctrl Pts',(15.,4.26533170166485,1.80169070105758));
#41955=CARTESIAN_POINT('Ctrl Pts',(15.,4.24199681605842,1.84723878333485));
#41956=CARTESIAN_POINT('Ctrl Pts',(15.,4.23276596498054,1.86525676600147));
#41957=CARTESIAN_POINT('Ctrl Pts',(15.,4.22341148066082,1.8832129271299));
#41958=CARTESIAN_POINT('Ctrl Pts',(15.,4.21393845086224,1.9010989158475));
#41959=CARTESIAN_POINT('Ctrl Pts',(15.,4.15009794689424,2.02163590960511));
#41960=CARTESIAN_POINT('Ctrl Pts',(15.,4.08082383939265,2.13909255365038));
#41961=CARTESIAN_POINT('Ctrl Pts',(15.,4.00648273399672,2.25317473996996));
#41962=CARTESIAN_POINT('Ctrl Pts',(15.,3.93094927503506,2.36908668522197));
#41963=CARTESIAN_POINT('Ctrl Pts',(15.,3.85018442561141,2.48151572963273));
#41964=CARTESIAN_POINT('Ctrl Pts',(15.,3.76452857661151,2.59012356957856));
#41965=CARTESIAN_POINT('Ctrl Pts',(15.,3.67917632204047,2.69834646517415));
#41966=CARTESIAN_POINT('Ctrl Pts',(15.,3.58896700611038,2.80277576926211));
#41967=CARTESIAN_POINT('Ctrl Pts',(15.,3.49420334350769,2.90303817573571));
#41968=CARTESIAN_POINT('Ctrl Pts',(15.,3.43040339532139,2.97054017135684));
#41969=CARTESIAN_POINT('Ctrl Pts',(15.,3.36453840688444,3.03615263398548));
#41970=CARTESIAN_POINT('Ctrl Pts',(15.,3.29669428988104,3.09974975199444));
#41971=CARTESIAN_POINT('Ctrl Pts',(15.,3.2611435518308,3.13307503623351));
#41972=CARTESIAN_POINT('Ctrl Pts',(15.,3.2250493045892,3.16584677269137));
#41973=CARTESIAN_POINT('Ctrl Pts',(15.,3.18842348307835,3.19804567312667));
#41974=CARTESIAN_POINT('Ctrl Pts',(15.,3.17313594847647,3.2114854209396));
#41975=CARTESIAN_POINT('Ctrl Pts',(15.,3.15775579949857,3.22482535854092));
#41976=CARTESIAN_POINT('Ctrl Pts',(15.,3.14228389185458,3.23806403845506));
#41977=CARTESIAN_POINT('Ctrl Pts',(15.,3.12716082301245,3.25100423124363));
#41978=CARTESIAN_POINT('Ctrl Pts',(15.,3.1119569353217,3.26384180774895));
#41979=CARTESIAN_POINT('Ctrl Pts',(15.,3.09667494792814,3.276574287178));
#41980=CARTESIAN_POINT('Ctrl Pts',(15.,3.09356639373681,3.27916423842426));
#41981=CARTESIAN_POINT('Ctrl Pts',(15.,3.09045458489432,3.28174986078853));
#41982=CARTESIAN_POINT('Ctrl Pts',(15.,3.08733952984974,3.28433114559335));
#41983=CARTESIAN_POINT('Ctrl Pts',(15.,2.98213805185187,3.37150616263602));
#41984=CARTESIAN_POINT('Ctrl Pts',(15.,2.87323649961196,3.45373767302407));
#41985=CARTESIAN_POINT('Ctrl Pts',(15.,2.76096821108068,3.53084903830942));
#41986=CARTESIAN_POINT('Ctrl Pts',(15.,2.64885274757775,3.607855435872));
#41987=CARTESIAN_POINT('Ctrl Pts',(15.,2.53337902731004,3.67975592914996));
#41988=CARTESIAN_POINT('Ctrl Pts',(15.,2.41485687951612,3.74632782212485));
#41989=CARTESIAN_POINT('Ctrl Pts',(15.,2.36383379103652,3.77498663103725));
#41990=CARTESIAN_POINT('Ctrl Pts',(15.,2.31224553332968,3.80265729945555));
#41991=CARTESIAN_POINT('Ctrl Pts',(15.,2.26011603649344,3.82931916305926));
#41992=CARTESIAN_POINT('Ctrl Pts',(15.,2.23334563507941,3.8430110042324));
#41993=CARTESIAN_POINT('Ctrl Pts',(15.,2.20643249237716,3.85643677448972));
#41994=CARTESIAN_POINT('Ctrl Pts',(15.,2.17937981938905,3.8695934871651));
#41995=CARTESIAN_POINT('Ctrl Pts',(15.,2.15885041590124,3.87957769328051));
#41996=CARTESIAN_POINT('Ctrl Pts',(15.,2.13824932722211,3.889402721209));
#41997=CARTESIAN_POINT('Ctrl Pts',(15.,2.11758052897823,3.89906654384036));
#41998=CARTESIAN_POINT('Ctrl Pts',(15.,1.99606455224882,3.95588207961238));
#41999=CARTESIAN_POINT('Ctrl Pts',(15.,1.87218227454613,4.00714279893364));
#42000=CARTESIAN_POINT('Ctrl Pts',(15.,1.74623943949728,4.05264771511785));
#42001=CARTESIAN_POINT('Ctrl Pts',(15.,1.62228293761301,4.09743494121565));
#42002=CARTESIAN_POINT('Ctrl Pts',(15.,1.49632971967395,4.13664664515206));
#42003=CARTESIAN_POINT('Ctrl Pts',(15.,1.36866090588019,4.17004234853293));
#42004=CARTESIAN_POINT('Ctrl Pts',(15.,1.28087501187527,4.19300544805659));
#42005=CARTESIAN_POINT('Ctrl Pts',(15.,1.19227776673793,4.21321772214408));
#42006=CARTESIAN_POINT('Ctrl Pts',(15.,1.10295997362678,4.23058663740352));
#42007=CARTESIAN_POINT('Ctrl Pts',(14.6196795453431,-4.93380912478971,-0.000781869070653209));
#42008=CARTESIAN_POINT('Ctrl Pts',(14.6440164183552,-4.93522618578535,-0.759185507612087));
#42009=CARTESIAN_POINT('Ctrl Pts',(14.6683532913673,-4.77108836500343,-1.5170353890311));
#42010=CARTESIAN_POINT('Ctrl Pts',(14.6926901643794,-4.43811057180526,-2.19164729176556));
#42011=CARTESIAN_POINT('Ctrl Pts',(14.7457234551343,-3.71250756961112,-3.66171656346831));
#42012=CARTESIAN_POINT('Ctrl Pts',(14.7987567458892,-2.18514735941808,-4.7365201381057));
#42013=CARTESIAN_POINT('Ctrl Pts',(14.8517900366441,-0.555787191338123,
-4.91967375502775));
#42014=CARTESIAN_POINT('Ctrl Pts',(14.9011933577627,0.962048161810347,-5.09029105638777));
#42015=CARTESIAN_POINT('Ctrl Pts',(14.9505966788814,2.56839815963549,-4.48714255609281));
#42016=CARTESIAN_POINT('Ctrl Pts',(15.,3.61714728420828,-3.37770697643486));
#42017=CARTESIAN_POINT('',(2.442,-2.53835875722685,-3.55965150255047));
#42018=CARTESIAN_POINT('Ctrl Pts',(2.442,-2.54476592700513,-3.5626931430771));
#42019=CARTESIAN_POINT('Ctrl Pts',(2.442,-2.62978545394211,-3.51047303783495));
#42020=CARTESIAN_POINT('Ctrl Pts',(2.442,-2.71273826723953,-3.45525941651742));
#42021=CARTESIAN_POINT('Ctrl Pts',(2.442,-2.79343800990703,-3.3970840011207));
#42022=CARTESIAN_POINT('Ctrl Pts',(2.442,-2.89895370622653,-3.32101908119211));
#42023=CARTESIAN_POINT('Ctrl Pts',(2.442,-3.00061904678095,-3.23989255120093));
#42024=CARTESIAN_POINT('Ctrl Pts',(2.442,-3.09834171154448,-3.15412282181048));
#42025=CARTESIAN_POINT('Ctrl Pts',(2.442,-3.1628382401109,-3.09751517797319));
#42026=CARTESIAN_POINT('Ctrl Pts',(2.442,-3.2256168811051,-3.03888395058717));
#42027=CARTESIAN_POINT('Ctrl Pts',(2.442,-3.28664452788624,-2.97833910745001));
#42028=CARTESIAN_POINT('Ctrl Pts',(2.442,-3.32011196664812,-2.94513643723554));
#42029=CARTESIAN_POINT('Ctrl Pts',(2.442,-3.35305271398046,-2.91135813117016));
#42030=CARTESIAN_POINT('Ctrl Pts',(2.442,-3.3854605609159,-2.8770214217979));
#42031=CARTESIAN_POINT('Ctrl Pts',(2.442,-3.40589909658775,-2.85536641766396));
#42032=CARTESIAN_POINT('Ctrl Pts',(2.442,-3.42612869710155,-2.83348579784071));
#42033=CARTESIAN_POINT('Ctrl Pts',(2.442,-3.44612818959239,-2.81140576655678));
#42034=CARTESIAN_POINT('Ctrl Pts',(2.442,-3.53547878676924,-2.71276006433175));
#42035=CARTESIAN_POINT('Ctrl Pts',(2.442,-3.62031028150167,-2.61006461635602));
#42036=CARTESIAN_POINT('Ctrl Pts',(2.442,-3.70052458494235,-2.50375047198745));
#42037=CARTESIAN_POINT('Ctrl Pts',(2.442,-3.7820321149224,-2.39572231568946));
#42038=CARTESIAN_POINT('Ctrl Pts',(2.442,-3.85877282818418,-2.28395727639001));
#42039=CARTESIAN_POINT('Ctrl Pts',(2.442,-3.93061046973195,-2.16886637126524));
#42040=CARTESIAN_POINT('Ctrl Pts',(2.442,-3.9620394379091,-2.11851410027316));
#42041=CARTESIAN_POINT('Ctrl Pts',(2.442,-3.9925294608403,-2.06752476305505));
#42042=CARTESIAN_POINT('Ctrl Pts',(2.442,-4.02206682291391,-2.01593079161707));
#42043=CARTESIAN_POINT('Ctrl Pts',(2.442,-4.03680819585422,-1.99018150593124));
#42044=CARTESIAN_POINT('Ctrl Pts',(2.442,-4.05131226051438,-1.96428160335949));
#42045=CARTESIAN_POINT('Ctrl Pts',(2.442,-4.06557717039628,-1.93823502190503));
#42046=CARTESIAN_POINT('Ctrl Pts',(2.442,-4.07800796634773,-1.91553738539882));
#42047=CARTESIAN_POINT('Ctrl Pts',(2.442,-4.09025879764027,-1.89272505333989));
#42048=CARTESIAN_POINT('Ctrl Pts',(2.442,-4.10231620390219,-1.86982427382633));
#42049=CARTESIAN_POINT('Ctrl Pts',(2.442,-4.16671595836278,-1.74750903076393));
#42050=CARTESIAN_POINT('Ctrl Pts',(2.442,-4.22567136107007,-1.62254840773803));
#42051=CARTESIAN_POINT('Ctrl Pts',(2.442,-4.27907565912676,-1.49538917481992));
#42052=CARTESIAN_POINT('Ctrl Pts',(2.442,-4.33307972063718,-1.3668018646967));
#42053=CARTESIAN_POINT('Ctrl Pts',(2.442,-4.38140775201378,-1.23596560038919));
#42054=CARTESIAN_POINT('Ctrl Pts',(2.442,-4.4239099749577,-1.10330645426441));
#42055=CARTESIAN_POINT('Ctrl Pts',(2.442,-4.46640455952458,-0.970671149259102));
#42056=CARTESIAN_POINT('Ctrl Pts',(2.442,-4.50307583544893,-0.836212855602582));
#42057=CARTESIAN_POINT('Ctrl Pts',(2.442,-4.53372854767286,-0.700332695469703));
#42058=CARTESIAN_POINT('Ctrl Pts',(2.442,-4.55671808184081,-0.598422575370044));
#42059=CARTESIAN_POINT('Ctrl Pts',(2.442,-4.57632128194439,-0.495712076186221));
#42060=CARTESIAN_POINT('Ctrl Pts',(2.442,-4.59243682756127,-0.392365211825747));
#42061=CARTESIAN_POINT('Ctrl Pts',(2.442,-4.59910320879343,-0.349614589950796));
#42062=CARTESIAN_POINT('Ctrl Pts',(2.442,-4.60517259456302,-0.306755042017714));
#42063=CARTESIAN_POINT('Ctrl Pts',(2.442,-4.61063692900446,-0.263798081557451));
#42064=CARTESIAN_POINT('Ctrl Pts',(2.442,-4.61410845547613,-0.236507250994499));
#42065=CARTESIAN_POINT('Ctrl Pts',(2.442,-4.61733639162291,-0.209170445649368));
#42066=CARTESIAN_POINT('Ctrl Pts',(2.442,-4.62031493224596,-0.18182658773287));
#42067=CARTESIAN_POINT('Ctrl Pts',(2.442,-4.63566282271897,-0.0409285475431649));
#42068=CARTESIAN_POINT('Ctrl Pts',(2.442,-4.64441339445427,0.100293053460323));
#42069=CARTESIAN_POINT('Ctrl Pts',(2.442,-4.64641666149764,0.241410427951467));
#42070=CARTESIAN_POINT('Ctrl Pts',(2.442,-4.64785067414324,0.34242746419886));
#42071=CARTESIAN_POINT('Ctrl Pts',(2.442,-4.64582632158149,0.44339171925975));
#42072=CARTESIAN_POINT('Ctrl Pts',(2.442,-4.64027315559012,0.544151909983444));
#42073=CARTESIAN_POINT('Ctrl Pts',(2.442,-4.63271766788419,0.681243504839959));
#42074=CARTESIAN_POINT('Ctrl Pts',(2.442,-4.61863213421743,0.817957532855541));
#42075=CARTESIAN_POINT('Ctrl Pts',(2.442,-4.59828444891196,0.953915700962727));
#42076=CARTESIAN_POINT('Ctrl Pts',(2.442,-4.57764456106668,1.09182629370359));
#42077=CARTESIAN_POINT('Ctrl Pts',(2.442,-4.55056120109121,1.22895990852911));
#42078=CARTESIAN_POINT('Ctrl Pts',(2.442,-4.51726046982246,1.36491871255982));
#42079=CARTESIAN_POINT('Ctrl Pts',(2.442,-4.50842331151333,1.40099868524999));
#42080=CARTESIAN_POINT('Ctrl Pts',(2.442,-4.49914802401335,1.43699587249988));
#42081=CARTESIAN_POINT('Ctrl Pts',(2.442,-4.48943823757219,1.47290269877862));
#42082=CARTESIAN_POINT('Ctrl Pts',(2.442,-4.48092388288684,1.50438881398979));
#42083=CARTESIAN_POINT('Ctrl Pts',(2.442,-4.47207542720719,1.53580544774456));
#42084=CARTESIAN_POINT('Ctrl Pts',(2.442,-4.46289516701416,1.56714743748963));
#42085=CARTESIAN_POINT('Ctrl Pts',(2.442,-4.4581432952735,1.58337062857943));
#42086=CARTESIAN_POINT('Ctrl Pts',(2.442,-4.453303331417,1.59957094704679));
#42087=CARTESIAN_POINT('Ctrl Pts',(2.442,-4.44837819999916,1.61573970578171));
#42088=CARTESIAN_POINT('Ctrl Pts',(2.442,-4.40742424060596,1.75018783162665));
#42089=CARTESIAN_POINT('Ctrl Pts',(2.442,-4.36053854645612,1.8826158785883));
#42090=CARTESIAN_POINT('Ctrl Pts',(2.442,-4.30802922843631,2.01263872476853));
#42091=CARTESIAN_POINT('Ctrl Pts',(2.442,-4.25424635130186,2.1458151403934));
#42092=CARTESIAN_POINT('Ctrl Pts',(2.442,-4.19456362122613,2.2764690547453));
#42093=CARTESIAN_POINT('Ctrl Pts',(2.442,-4.12925671054388,2.40418379216483));
#42094=CARTESIAN_POINT('Ctrl Pts',(2.442,-4.06394979986163,2.53189852958436));
#42095=CARTESIAN_POINT('Ctrl Pts',(2.442,-3.99301835733987,2.65667490140106));
#42096=CARTESIAN_POINT('Ctrl Pts',(2.442,-3.91668729343188,2.77808134282536));
#42097=CARTESIAN_POINT('Ctrl Pts',(2.442,-3.86260196243339,2.86410539690767));
#42098=CARTESIAN_POINT('Ctrl Pts',(2.442,-3.80580461723952,2.94843722848745));
#42099=CARTESIAN_POINT('Ctrl Pts',(2.442,-3.74638249061058,3.03097790114148));
#42100=CARTESIAN_POINT('Ctrl Pts',(2.442,-3.71992510293393,3.06772869919243));
#42101=CARTESIAN_POINT('Ctrl Pts',(2.442,-3.69294722628387,3.10412431349132));
#42102=CARTESIAN_POINT('Ctrl Pts',(2.442,-3.66545589048721,3.14015549455613));
#42103=CARTESIAN_POINT('Ctrl Pts',(2.442,-3.65033714917244,3.15997068687031));
#42104=CARTESIAN_POINT('Ctrl Pts',(2.442,-3.63506311013638,3.17967565396125));
#42105=CARTESIAN_POINT('Ctrl Pts',(2.442,-3.61963489260881,3.19926881184803));
#42106=CARTESIAN_POINT('Ctrl Pts',(2.442,-3.60720401841877,3.21505547548825));
#42107=CARTESIAN_POINT('Ctrl Pts',(2.442,-3.59467227033619,3.23077043036965));
#42108=CARTESIAN_POINT('Ctrl Pts',(2.442,-3.58205135250517,3.24639931681853));
#42109=CARTESIAN_POINT('Ctrl Pts',(2.442,-3.49134773591549,3.35872050796831));
#42110=CARTESIAN_POINT('Ctrl Pts',(2.442,-3.39591563875028,3.46676085122522));
#42111=CARTESIAN_POINT('Ctrl Pts',(2.442,-3.29608057910503,3.57028822611568));
#42112=CARTESIAN_POINT('Ctrl Pts',(2.442,-3.19517230794316,3.67492850434302));
#42113=CARTESIAN_POINT('Ctrl Pts',(2.442,-3.0897655304088,3.77495887254834));
#42114=CARTESIAN_POINT('Ctrl Pts',(2.442,-2.98014938690035,3.87011544671376));
#42115=CARTESIAN_POINT('Ctrl Pts',(2.442,-2.87082805651637,3.96501609683327));
#42116=CARTESIAN_POINT('Ctrl Pts',(2.442,-2.75731950265513,4.0550696988635));
#42117=CARTESIAN_POINT('Ctrl Pts',(2.442,-2.63987053755491,4.13998182739019));
#42118=CARTESIAN_POINT('Ctrl Pts',(2.442,-2.52418958462514,4.22361573540189));
#42119=CARTESIAN_POINT('Ctrl Pts',(2.442,-2.40468545676967,4.30226226485196));
#42120=CARTESIAN_POINT('Ctrl Pts',(2.442,-2.28156245177909,4.37560083866042));
#42121=CARTESIAN_POINT('Ctrl Pts',(2.442,-2.24442645244809,4.39772100400316));
#42122=CARTESIAN_POINT('Ctrl Pts',(2.442,-2.20696104153711,4.41935798923143));
#42123=CARTESIAN_POINT('Ctrl Pts',(2.442,-2.16917135428609,4.440502182833));
#42124=CARTESIAN_POINT('Ctrl Pts',(2.442,-2.54476592700512,-3.56269314307711));
#42125=CARTESIAN_POINT('Ctrl Pts',(2.49140332111864,-1.44097312181521,-4.34097806869132));
#42126=CARTESIAN_POINT('Ctrl Pts',(2.59383993299217,1.66634742138771,-4.84186302574293));
#42127=CARTESIAN_POINT('Ctrl Pts',(2.74930983562058,4.99693901203929,-1.32514448694853));
#42128=CARTESIAN_POINT('Ctrl Pts',(2.90840970788525,3.81836490750785,3.48733811875686));
#42129=CARTESIAN_POINT('Ctrl Pts',(3.06750958014992,-0.870820132749773,
5.09763547084385));
#42130=CARTESIAN_POINT('Ctrl Pts',(3.19490297482318,-3.98390803658994,2.63581590170141));
#42131=CARTESIAN_POINT('Ctrl Pts',(3.26926307874154,-4.36855469401081,0.589937737338669));
#42132=CARTESIAN_POINT('Ctrl Pts',(3.29058989190502,-4.36585073597542,0.00220040158241119));
#42133=CARTESIAN_POINT('Origin',(2.442,-4.51336705371395E-16,0.));
#42134=CARTESIAN_POINT('',(2.442,-4.942,-6.05220448138622E-16));
#42135=CARTESIAN_POINT('Origin',(2.442,0.,0.));
#42136=CARTESIAN_POINT('Origin',(2.442,0.,0.));
#42137=CARTESIAN_POINT('',(2.442,2.53835875722685,-3.55965150255046));
#42138=CARTESIAN_POINT('Ctrl Pts',(2.442,2.17574915139363,4.44508346536535));
#42139=CARTESIAN_POINT('Ctrl Pts',(2.442,2.27393842303551,4.39078104776067));
#42140=CARTESIAN_POINT('Ctrl Pts',(2.442,2.36998244314937,4.3330049458102));
#42141=CARTESIAN_POINT('Ctrl Pts',(2.442,2.46367187398648,4.27174666136024));
#42142=CARTESIAN_POINT('Ctrl Pts',(2.442,2.5844170631878,4.19279812810554));
#42143=CARTESIAN_POINT('Ctrl Pts',(2.442,2.70125282028097,4.10806686721375));
#42144=CARTESIAN_POINT('Ctrl Pts',(2.442,2.81399829649834,4.0179742426192));
#42145=CARTESIAN_POINT('Ctrl Pts',(2.442,2.88459899475852,3.96155865577824));
#42146=CARTESIAN_POINT('Ctrl Pts',(2.442,2.95359512383052,3.90303992936404));
#42147=CARTESIAN_POINT('Ctrl Pts',(2.442,3.02093464599862,3.84251467551746));
#42148=CARTESIAN_POINT('Ctrl Pts',(2.442,3.05981425658111,3.80756939785292));
#42149=CARTESIAN_POINT('Ctrl Pts',(2.442,3.09814151990465,3.77195515070165));
#42150=CARTESIAN_POINT('Ctrl Pts',(2.442,3.13590544710532,3.73568989784483));
#42151=CARTESIAN_POINT('Ctrl Pts',(2.442,3.15300708404911,3.71926694520179));
#42152=CARTESIAN_POINT('Ctrl Pts',(2.442,3.16999457279843,3.70270910164703));
#42153=CARTESIAN_POINT('Ctrl Pts',(2.442,3.18686241961533,3.68602239183288));
#42154=CARTESIAN_POINT('Ctrl Pts',(2.442,3.28923141842677,3.58475269240563));
#42155=CARTESIAN_POINT('Ctrl Pts',(2.442,3.38701377017835,3.47892244063486));
#42156=CARTESIAN_POINT('Ctrl Pts',(2.442,3.48003362886399,3.36895094136753));
#42157=CARTESIAN_POINT('Ctrl Pts',(2.442,3.57217417702745,3.26001899535055));
#42158=CARTESIAN_POINT('Ctrl Pts',(2.442,3.65964211140465,3.14702295122995));
#42159=CARTESIAN_POINT('Ctrl Pts',(2.442,3.7422262628366,3.03034212452304));
#42160=CARTESIAN_POINT('Ctrl Pts',(2.442,3.78089446668873,2.97570890598769));
#42161=CARTESIAN_POINT('Ctrl Pts',(2.442,3.81849136080162,2.92026751227786));
#42162=CARTESIAN_POINT('Ctrl Pts',(2.442,3.85499193604736,2.86405544490254));
#42163=CARTESIAN_POINT('Ctrl Pts',(2.442,3.87362735212517,2.83535630092795));
#42164=CARTESIAN_POINT('Ctrl Pts',(2.442,3.89197696341109,2.80645625920063));
#42165=CARTESIAN_POINT('Ctrl Pts',(2.442,3.91003721456594,2.77736024690742));
#42166=CARTESIAN_POINT('Ctrl Pts',(2.442,3.92205565721194,2.75799790515617));
#42167=CARTESIAN_POINT('Ctrl Pts',(2.442,3.93394595584916,2.73854877858126));
#42168=CARTESIAN_POINT('Ctrl Pts',(2.442,3.94570702391603,2.71901431104455));
#42169=CARTESIAN_POINT('Ctrl Pts',(2.442,3.95577364652109,2.70229422139244));
#42170=CARTESIAN_POINT('Ctrl Pts',(2.442,3.96574336530622,2.68551524968513));
#42171=CARTESIAN_POINT('Ctrl Pts',(2.442,3.97561165866684,2.66868529315884));
#42172=CARTESIAN_POINT('Ctrl Pts',(2.442,4.0484785180189,2.54441394954467));
#42173=CARTESIAN_POINT('Ctrl Pts',(2.442,4.11588703074174,2.417252482731));
#42174=CARTESIAN_POINT('Ctrl Pts',(2.442,4.17765759536301,2.28760379752714));
#42175=CARTESIAN_POINT('Ctrl Pts',(2.442,4.23930632062562,2.1582108378902));
#42176=CARTESIAN_POINT('Ctrl Pts',(2.442,4.29533963180827,2.02633968480384));
#42177=CARTESIAN_POINT('Ctrl Pts',(2.442,4.34553172404092,1.89237006930549));
#42178=CARTESIAN_POINT('Ctrl Pts',(2.442,4.3954097927595,1.75923862586906));
#42179=CARTESIAN_POINT('Ctrl Pts',(2.442,4.43951977998791,1.62403415245028));
#42180=CARTESIAN_POINT('Ctrl Pts',(2.442,4.47758902444189,1.48712008745362));
#42181=CARTESIAN_POINT('Ctrl Pts',(2.442,4.50614095778236,1.38443453870612));
#42182=CARTESIAN_POINT('Ctrl Pts',(2.442,4.53129396154129,1.28078709139831));
#42183=CARTESIAN_POINT('Ctrl Pts',(2.442,4.55291251756889,1.17633139028504));
#42184=CARTESIAN_POINT('Ctrl Pts',(2.442,4.56133538043379,1.13563412795118));
#42185=CARTESIAN_POINT('Ctrl Pts',(2.442,4.56922152498248,1.09481419371376));
#42186=CARTESIAN_POINT('Ctrl Pts',(2.442,4.57656216912564,1.05388078213205));
#42187=CARTESIAN_POINT('Ctrl Pts',(2.442,4.57999850661446,1.03471883748249));
#42188=CARTESIAN_POINT('Ctrl Pts',(2.442,4.58331529642097,1.0155320264721));
#42189=CARTESIAN_POINT('Ctrl Pts',(2.442,4.58651160414136,0.996321299140574));
#42190=CARTESIAN_POINT('Ctrl Pts',(2.442,4.58947907947802,0.978485920152514));
#42191=CARTESIAN_POINT('Ctrl Pts',(2.442,4.59234189163767,0.96063463462557));
#42192=CARTESIAN_POINT('Ctrl Pts',(2.442,4.5950983362346,0.942776006748339));
#42193=CARTESIAN_POINT('Ctrl Pts',(2.442,4.61625709495595,0.80569130032306));
#42194=CARTESIAN_POINT('Ctrl Pts',(2.442,4.63117586815545,0.668035160277971));
#42195=CARTESIAN_POINT('Ctrl Pts',(2.442,4.63964588153731,0.530152019773935));
#42196=CARTESIAN_POINT('Ctrl Pts',(2.442,4.64589434249683,0.428433476771435));
#42197=CARTESIAN_POINT('Ctrl Pts',(2.442,4.64863225146208,0.326591103300644));
#42198=CARTESIAN_POINT('Ctrl Pts',(2.442,4.64775755650822,0.224762372538238));
#42199=CARTESIAN_POINT('Ctrl Pts',(2.442,4.64656482049337,0.0859084852581371));
#42200=CARTESIAN_POINT('Ctrl Pts',(2.442,4.63865657058669,-0.0529208546614462));
#42201=CARTESIAN_POINT('Ctrl Pts',(2.442,4.62423104198867,-0.191283307402043));
#42202=CARTESIAN_POINT('Ctrl Pts',(2.442,4.60977115054211,-0.329975351392945));
#42203=CARTESIAN_POINT('Ctrl Pts',(2.442,4.58876252367756,-0.46819910089437));
#42204=CARTESIAN_POINT('Ctrl Pts',(2.442,4.56135630357545,-0.605490145703256));
#42205=CARTESIAN_POINT('Ctrl Pts',(2.442,4.55350762775731,-0.644807968424675));
#42206=CARTESIAN_POINT('Ctrl Pts',(2.442,4.54513396735176,-0.684049133988946));
#42207=CARTESIAN_POINT('Ctrl Pts',(2.442,4.53623820728588,-0.723202303446103));
#42208=CARTESIAN_POINT('Ctrl Pts',(2.442,4.5313324340908,-0.744794226767168));
#42209=CARTESIAN_POINT('Ctrl Pts',(2.442,4.52626787353334,-0.766359384643764));
#42210=CARTESIAN_POINT('Ctrl Pts',(2.442,4.52104497323125,-0.787895845429721));
#42211=CARTESIAN_POINT('Ctrl Pts',(2.442,4.5172361488522,-0.8036014097973));
#42212=CARTESIAN_POINT('Ctrl Pts',(2.442,4.51334341520424,-0.819290338968791));
#42213=CARTESIAN_POINT('Ctrl Pts',(2.442,4.50936943923919,-0.834952609158587));
#42214=CARTESIAN_POINT('Ctrl Pts',(2.442,4.47555821798973,-0.968209701630727));
#42215=CARTESIAN_POINT('Ctrl Pts',(2.442,4.43582542541766,-1.09972449252871));
#42216=CARTESIAN_POINT('Ctrl Pts',(2.442,4.39039730266716,-1.22908266281593));
#42217=CARTESIAN_POINT('Ctrl Pts',(2.442,4.34489179137645,-1.3586611996813));
#42218=CARTESIAN_POINT('Ctrl Pts',(2.442,4.29367113064587,-1.48607655014092));
#42219=CARTESIAN_POINT('Ctrl Pts',(2.442,4.23691420217938,-1.61089379623584));
#42220=CARTESIAN_POINT('Ctrl Pts',(2.442,4.18155469671018,-1.73263789346833));
#42221=CARTESIAN_POINT('Ctrl Pts',(2.442,4.12092766181959,-1.85191084354222));
#42222=CARTESIAN_POINT('Ctrl Pts',(2.442,4.05516007761845,-1.96828148190162));
#42223=CARTESIAN_POINT('Ctrl Pts',(2.442,4.00954370013694,-2.04899612318953));
#42224=CARTESIAN_POINT('Ctrl Pts',(2.442,3.96145346076867,-2.12831387894083));
#42225=CARTESIAN_POINT('Ctrl Pts',(2.442,3.91094915975807,-2.20613095532952));
#42226=CARTESIAN_POINT('Ctrl Pts',(2.442,3.88614906048688,-2.24434297254026));
#42227=CARTESIAN_POINT('Ctrl Pts',(2.442,3.86076675497426,-2.282193003155));
#42228=CARTESIAN_POINT('Ctrl Pts',(2.442,3.83480875614052,-2.31966796647033));
#42229=CARTESIAN_POINT('Ctrl Pts',(2.442,3.81920063335576,-2.34220105280439));
#42230=CARTESIAN_POINT('Ctrl Pts',(2.442,3.80338436629605,-2.36459852612736));
#42231=CARTESIAN_POINT('Ctrl Pts',(2.442,3.7873613119109,-2.38685744513759));
#42232=CARTESIAN_POINT('Ctrl Pts',(2.442,3.7758201780042,-2.4028901664116));
#42233=CARTESIAN_POINT('Ctrl Pts',(2.442,3.76417601821905,-2.41884502890004));
#42234=CARTESIAN_POINT('Ctrl Pts',(2.442,3.75243436377876,-2.43471475864026));
#42235=CARTESIAN_POINT('Ctrl Pts',(2.442,3.66960454851416,-2.54666548835777));
#42236=CARTESIAN_POINT('Ctrl Pts',(2.442,3.58185449040889,-2.65448334060622));
#42237=CARTESIAN_POINT('Ctrl Pts',(2.442,3.48945737545467,-2.75787873450307));
#42238=CARTESIAN_POINT('Ctrl Pts',(2.442,3.4000952056859,-2.85787792546587));
#42239=CARTESIAN_POINT('Ctrl Pts',(2.442,3.30638549610641,-2.9537407482109));
#42240=CARTESIAN_POINT('Ctrl Pts',(2.442,3.2085383796773,-3.0451683648695));
#42241=CARTESIAN_POINT('Ctrl Pts',(2.442,3.11163722459243,-3.13571208229519));
#42242=CARTESIAN_POINT('Ctrl Pts',(2.442,3.01067774999476,-3.2219063667006));
#42243=CARTESIAN_POINT('Ctrl Pts',(2.442,2.90583625254343,-3.3034183821363));
#42244=CARTESIAN_POINT('Ctrl Pts',(2.442,2.80312546231272,-3.38327381841128));
#42245=CARTESIAN_POINT('Ctrl Pts',(2.442,2.69668833862294,-3.45863567293516));
#42246=CARTESIAN_POINT('Ctrl Pts',(2.442,2.58667139778511,-3.52914465758715));
#42247=CARTESIAN_POINT('Ctrl Pts',(2.442,2.57064305173904,-3.53941709742008));
#42248=CARTESIAN_POINT('Ctrl Pts',(2.442,2.55453869568167,-3.54958644617886));
#42249=CARTESIAN_POINT('Ctrl Pts',(2.442,2.53835875722688,-3.55965150255044));
#42250=CARTESIAN_POINT('Origin',(2.442,0.,0.));
#42251=CARTESIAN_POINT('Origin',(0.59341010809499,0.,0.));
#42252=CARTESIAN_POINT('Ctrl Pts',(2.442,2.53835875722685,-3.55965150255046));
#42253=CARTESIAN_POINT('Ctrl Pts',(2.46851664537744,3.13142872242371,-3.13673809691875));
#42254=CARTESIAN_POINT('Ctrl Pts',(2.52154993613233,4.09225274784706,-1.99049633126479));
#42255=CARTESIAN_POINT('Ctrl Pts',(2.62761651764211,4.7260019639421,0.960791047637318));
#42256=CARTESIAN_POINT('Ctrl Pts',(2.76019974452934,2.58737835299157,4.47689474139548));
#42257=CARTESIAN_POINT('Ctrl Pts',(2.919299616794,-2.37603566784794,4.59603588578678));
#42258=CARTESIAN_POINT('Ctrl Pts',(3.03036973798255,-4.31032048543761,1.72682559663222));
#42259=CARTESIAN_POINT('Ctrl Pts',(3.08840656841621,-4.37812303221146,0.139072831115389));
#42260=CARTESIAN_POINT('Ctrl Pts',(3.09341010809498,-4.3772103018885,0.00211459834950896));
#42261=CARTESIAN_POINT('Ctrl Pts',(2.11291034656191,2.86929757049747,-4.02374147429197));
#42262=CARTESIAN_POINT('Ctrl Pts',(2.13942699193936,3.53968910023281,-3.5456906850349));
#42263=CARTESIAN_POINT('Ctrl Pts',(2.19246028269425,4.62578066785455,-2.25000751809486));
#42264=CARTESIAN_POINT('Ctrl Pts',(2.29852686420402,5.34215501047619,1.08605429035303));
#42265=CARTESIAN_POINT('Ctrl Pts',(2.43111009109125,2.92470810166618,5.06057040530109));
#42266=CARTESIAN_POINT('Ctrl Pts',(2.59020996335591,-2.68581158977685,5.19524459001793));
#42267=CARTESIAN_POINT('Ctrl Pts',(2.74930983562059,-5.81776718514297,0.549476222463121));
#42268=CARTESIAN_POINT('Ctrl Pts',(2.90840970788525,-3.60982419207306,-4.59760538215123));
#42269=CARTESIAN_POINT('Ctrl Pts',(3.06750958014992,1.91775327909424,-5.52219013742084));
#42270=CARTESIAN_POINT('Ctrl Pts',(3.22660945241459,5.68177238095773,-1.37195370543713));
#42271=CARTESIAN_POINT('Ctrl Pts',(3.38570932467925,4.22608756769742,4.03835092191338));
#42272=CARTESIAN_POINT('Ctrl Pts',(3.54480919694392,-1.11299042776881,5.73842699095229));
#42273=CARTESIAN_POINT('Ctrl Pts',(3.70390906920859,-5.4292251435763,2.16582476905545));
#42274=CARTESIAN_POINT('Ctrl Pts',(3.86300894147326,-4.75712770456746,-3.39669458215663));
#42275=CARTESIAN_POINT('Ctrl Pts',(4.02210881373792,0.285939063906139,-5.83832346391982));
#42276=CARTESIAN_POINT('Ctrl Pts',(4.18120868600259,5.06625102656692,-2.91560479978825));
#42277=CARTESIAN_POINT('Ctrl Pts',(4.34030855826727,5.19164084677873,2.6859997205203));
#42278=CARTESIAN_POINT('Ctrl Pts',(4.49940843053192,0.54687470849627,5.81967771757739));
#42279=CARTESIAN_POINT('Ctrl Pts',(4.6585083027966,-4.60036279511536,3.60615672221117));
#42280=CARTESIAN_POINT('Ctrl Pts',(4.81760817506126,-5.52072884012978,-1.92074695394265));
#42281=CARTESIAN_POINT('Ctrl Pts',(4.97670804732594,-1.36857562124414,-5.68284387364681));
#42282=CARTESIAN_POINT('Ctrl Pts',(5.1358079195906,4.04104222632025,-4.2234688878305));
#42283=CARTESIAN_POINT('Ctrl Pts',(5.29490779185526,5.73769777151174,1.11648452511799));
#42284=CARTESIAN_POINT('Ctrl Pts',(5.45400766411994,2.16248115397357,5.4305974129897));
#42285=CARTESIAN_POINT('Ctrl Pts',(5.61310753638461,-3.39965143533879,4.75500608748046));
#42286=CARTESIAN_POINT('Ctrl Pts',(5.77220740864926,-5.83813972404732,-0.289547192923355));
#42287=CARTESIAN_POINT('Ctrl Pts',(5.93130728091394,-2.91246860837872,-5.0680607283612));
#42288=CARTESIAN_POINT('Ctrl Pts',(6.0904071531786,2.68921686697644,-5.1899735605652));
#42289=CARTESIAN_POINT('Ctrl Pts',(6.24950702544328,5.82001460606655,-0.543270591629312));
#42290=CARTESIAN_POINT('Ctrl Pts',(6.40860689770793,3.60330655718976,4.60259652730006));
#42291=CARTESIAN_POINT('Ctrl Pts',(6.56770676997262,-1.92416683377643,5.51953756503503));
#42292=CARTESIAN_POINT('Ctrl Pts',(6.72680664223726,-5.68369049173104,1.3650550665912));
#42293=CARTESIAN_POINT('Ctrl Pts',(6.88590651450195,-4.22096474954825,-4.04365793826525));
#42294=CARTESIAN_POINT('Ctrl Pts',(7.04500638676661,1.12003878766801,-5.73700497233726));
#42295=CARTESIAN_POINT('Ctrl Pts',(7.20410625903129,5.43193599084382,-2.15911656250658));
#42296=CARTESIAN_POINT('Ctrl Pts',(7.36320613129594,4.75289913298194,3.4025964748266));
#42297=CARTESIAN_POINT('Ctrl Pts',(7.52230600356062,-0.293163811150279,
5.83795922550374));
#42298=CARTESIAN_POINT('Ctrl Pts',(7.68140587582529,-5.06986399900541,2.90932843977449));
#42299=CARTESIAN_POINT('Ctrl Pts',(7.84050574808994,-5.18830662273838,-2.69243148980496));
#42300=CARTESIAN_POINT('Ctrl Pts',(7.99960562035463,-0.539665045588934,
-5.82035003908004));
#42301=CARTESIAN_POINT('Ctrl Pts',(8.15870549261927,4.6048278564103,-3.6004546034754));
#42302=CARTESIAN_POINT('Ctrl Pts',(8.31780536488397,5.51834450386409,1.92758576346817));
#42303=CARTESIAN_POINT('Ctrl Pts',(8.47690523714861,1.3615338148167,5.68453503903047));
#42304=CARTESIAN_POINT('Ctrl Pts',(8.6360051094133,-4.04627200800777,4.21845893378935));
#42305=CARTESIAN_POINT('Ctrl Pts',(8.79510498167795,-5.73631001862683,-1.12359259033407));
#42306=CARTESIAN_POINT('Ctrl Pts',(8.95420485394264,-2.15575111784886,-5.43327249976962));
#42307=CARTESIAN_POINT('Ctrl Pts',(9.11330472620728,3.40554019567974,-4.75079034629598));
#42308=CARTESIAN_POINT('Ctrl Pts',(9.27240459847197,5.83777649322883,0.29678031260383));
#42309=CARTESIAN_POINT('Ctrl Pts',(9.43150447073662,2.90618715117436,5.07166532622579));
#42310=CARTESIAN_POINT('Ctrl Pts',(9.5906043430013,-2.69564507754667,5.18663769263969));
#42311=CARTESIAN_POINT('Ctrl Pts',(9.74970421526597,-5.82068323937394,0.536059293058277));
#42312=CARTESIAN_POINT('Ctrl Pts',(9.90880408753062,-3.59760126753682,-4.60705741867106));
#42313=CARTESIAN_POINT('Ctrl Pts',(10.0679039597953,1.93100395317568,-5.51714932472587));
#42314=CARTESIAN_POINT('Ctrl Pts',(10.22700383206,5.68537740488418,-1.35801204068925));
#42315=CARTESIAN_POINT('Ctrl Pts',(10.3861037043246,4.21595149912367,4.04888452510772));
#42316=CARTESIAN_POINT('Ctrl Pts',(10.5452035765893,-1.12714596190438,5.7356128632083));
#42317=CARTESIAN_POINT('Ctrl Pts',(10.704303448854,-5.43460692333051,2.15238484641792));
#42318=CARTESIAN_POINT('Ctrl Pts',(10.8634033211186,-4.74867973691283,-3.40848261060413));
#42319=CARTESIAN_POINT('Ctrl Pts',(11.0225031933833,0.300396701142615,-5.83759151867781));
#42320=CARTESIAN_POINT('Ctrl Pts',(11.181603065648,5.07346470521744,-2.90304475095743));
#42321=CARTESIAN_POINT('Ctrl Pts',(11.3407029379127,5.18496677569499,2.6988576378476));
#42322=CARTESIAN_POINT('Ctrl Pts',(11.4998028101773,0.532453327864645,5.82101419233996));
#42323=CARTESIAN_POINT('Ctrl Pts',(11.658902682442,-4.60928519958409,3.59474657690306));
#42324=CARTESIAN_POINT('Ctrl Pts',(11.8180025547066,-5.51595205379273,-1.93442145157114));
#42325=CARTESIAN_POINT('Ctrl Pts',(11.9771024269713,-1.35448969649516,-5.68621749350692));
#42326=CARTESIAN_POINT('Ctrl Pts',(12.136202299236,4.0514953946209,-4.21344262933229));
#42327=CARTESIAN_POINT('Ctrl Pts',(12.2953021715007,5.73491368637922,1.13069925139314));
#42328=CARTESIAN_POINT('Ctrl Pts',(12.4544020437653,2.14901740440843,5.435938589368));
#42329=CARTESIAN_POINT('Ctrl Pts',(12.61350191603,-3.41142305691351,4.74656859320694));
#42330=CARTESIAN_POINT('Ctrl Pts',(12.7726017882947,-5.83740557016221,-0.304015443712614));
#42331=CARTESIAN_POINT('Ctrl Pts',(12.9317016605593,-2.89989880903194,-5.0752574033357));
#42332=CARTESIAN_POINT('Ctrl Pts',(13.090801532824,2.70206450851665,-5.18330294401542));
#42333=CARTESIAN_POINT('Ctrl Pts',(13.2499014050887,5.82135183321988,-0.528829760776661));
#42334=CARTESIAN_POINT('Ctrl Pts',(13.4090012773533,3.5918734029674,4.61147785931481));
#42335=CARTESIAN_POINT('Ctrl Pts',(13.568101149618,-1.93780541854324,5.51481660462604));
#42336=CARTESIAN_POINT('Ctrl Pts',(13.7272010218827,-5.68711825886611,1.35084425750601));
#42337=CARTESIAN_POINT('Ctrl Pts',(13.8863008941473,-4.21081163680671,-4.05386972141555));
#42338=CARTESIAN_POINT('Ctrl Pts',(14.045400766412,1.13402108049327,-5.73466282725512));
#42339=CARTESIAN_POINT('Ctrl Pts',(14.2045006386766,5.43771114302852,-2.14478518100188));
#42340=CARTESIAN_POINT('Ctrl Pts',(14.3636005109413,4.74360568499834,3.41270336314633));
#42341=CARTESIAN_POINT('Ctrl Pts',(14.522700383206,-0.305998010418999,5.84042082931615));
#42342=CARTESIAN_POINT('Ctrl Pts',(14.6818002554707,-5.08024498950095,2.89039809604342));
#42343=CARTESIAN_POINT('Ctrl Pts',(14.8143834823579,-5.15920127145973,-1.76090213189674));
#42344=CARTESIAN_POINT('Ctrl Pts',(14.9204500638677,-2.85592546693168,-4.27832564748306));
#42345=CARTESIAN_POINT('Ctrl Pts',(14.9734833546226,-1.26412269067526,-4.84802178039354));
#42346=CARTESIAN_POINT('Ctrl Pts',(15.,-0.444071852043585,-4.9220081460947));
#42347=CARTESIAN_POINT('Ctrl Pts',(2.22260689770794,2.7589846327406,-3.8690448170448));
#42348=CARTESIAN_POINT('Ctrl Pts',(2.24912354308539,3.40360230762978,-3.40937315566285));
#42349=CARTESIAN_POINT('Ctrl Pts',(2.30215683384028,4.44793802785205,-2.16350378915151));
#42350=CARTESIAN_POINT('Ctrl Pts',(2.40822341535005,5.13677066163149,1.04429987611446));
#42351=CARTESIAN_POINT('Ctrl Pts',(2.54080664223728,2.81226485210798,4.86601185066588));
#42352=CARTESIAN_POINT('Ctrl Pts',(2.69990651450194,-2.58255294913388,4.99550835527422));
#42353=CARTESIAN_POINT('Ctrl Pts',(2.85900638676662,-5.59409746333456,0.528351074290705));
#42354=CARTESIAN_POINT('Ctrl Pts',(3.01810625903128,-3.47104098760242,-4.42084596843032));
#42355=CARTESIAN_POINT('Ctrl Pts',(3.17720613129595,1.84402338774907,-5.30988416289433));
#42356=CARTESIAN_POINT('Ctrl Pts',(3.33630600356061,5.46333111175862,-1.31920760992254));
#42357=CARTESIAN_POINT('Ctrl Pts',(3.49540587582529,4.06361151794782,3.88309259023319));
#42358=CARTESIAN_POINT('Ctrl Pts',(3.65450574808995,-1.07020042751062,5.51780758013057));
#42359=CARTESIAN_POINT('Ctrl Pts',(3.81360562035462,-5.22049329872007,2.08255752783316));
#42360=CARTESIAN_POINT('Ctrl Pts',(3.97270549261928,-4.57423529989974,-3.2661053529762));
#42361=CARTESIAN_POINT('Ctrl Pts',(4.13180536488396,0.274945858292602,-5.6138634359666));
#42362=CARTESIAN_POINT('Ctrl Pts',(4.29090523714862,4.87147407491826,-2.8035115355309));
#42363=CARTESIAN_POINT('Ctrl Pts',(4.45000510941329,4.99204316145134,2.5827338470078));
#42364=CARTESIAN_POINT('Ctrl Pts',(4.60910498167796,0.525849578060337,5.59593454349003));
#42365=CARTESIAN_POINT('Ctrl Pts',(4.76820485394263,-4.42349736996929,3.46751451718887));
#42366=CARTESIAN_POINT('Ctrl Pts',(4.92730472620729,-5.30847904659991,-1.84690196785421));
#42367=CARTESIAN_POINT('Ctrl Pts',(5.08640459847196,-1.3159593994642,-5.46436140986841));
#42368=CARTESIAN_POINT('Ctrl Pts',(5.24550447073663,3.88568042482271,-4.06109351577712));
#42369=CARTESIAN_POINT('Ctrl Pts',(5.40460434300129,5.51710639624116,1.07356019088643));
#42370=CARTESIAN_POINT('Ctrl Pts',(5.56370421526597,2.0793424612874,5.22181280990026));
#42371=CARTESIAN_POINT('Ctrl Pts',(5.72280408753062,-3.26894852705989,4.57219525044661));
#42372=CARTESIAN_POINT('Ctrl Pts',(5.8819039597953,-5.61368676015234,-0.278415269277996));
#42373=CARTESIAN_POINT('Ctrl Pts',(6.04100383205997,-2.80049591805253,-4.87321420096569));
#42374=CARTESIAN_POINT('Ctrl Pts',(6.20010370432464,2.58582730713721,-4.99043997567904));
#42375=CARTESIAN_POINT('Ctrl Pts',(6.35920357658931,5.59625847997334,-0.522384024974179));
#42376=CARTESIAN_POINT('Ctrl Pts',(6.51830344885396,3.46477392953576,4.42564522414607));
#42377=CARTESIAN_POINT('Ctrl Pts',(6.67740332111864,-1.85019036707925,5.30733357123562));
#42378=CARTESIAN_POINT('Ctrl Pts',(6.83650319338331,-5.46517547889638,1.31257419596142));
#42379=CARTESIAN_POINT('Ctrl Pts',(6.99560306564797,-4.05868565152838,-3.88819557317615));
#42380=CARTESIAN_POINT('Ctrl Pts',(7.15470293791265,1.07697780635339,-5.51644023240523));
#42381=CARTESIAN_POINT('Ctrl Pts',(7.3138028101773,5.22309992482595,-2.07610722481408));
#42382=CARTESIAN_POINT('Ctrl Pts',(7.47290268244198,4.57016929986445,3.27178034163821));
#42383=CARTESIAN_POINT('Ctrl Pts',(7.63200255470663,-0.281892843097165,
5.61351320105094));
#42384=CARTESIAN_POINT('Ctrl Pts',(7.79110242697132,-4.87494814311488,2.79747647628658));
#42385=CARTESIAN_POINT('Ctrl Pts',(7.95020229923598,-4.98883712489937,-2.58891834066233));
#42386=CARTESIAN_POINT('Ctrl Pts',(8.10930217150065,-0.518917097660577,
-5.59658101693815));
#42387=CARTESIAN_POINT('Ctrl Pts',(8.26840204376531,4.42779076763695,-3.46203162195772));
#42388=CARTESIAN_POINT('Ctrl Pts',(8.42750191602998,5.30618637846259,1.85347785269139));
#42389=CARTESIAN_POINT('Ctrl Pts',(8.58660178829465,1.30918832213859,5.4659875567529));
#42390=CARTESIAN_POINT('Ctrl Pts',(8.74570166055931,-3.89070914246317,4.05627617429522));
#42391=CARTESIAN_POINT('Ctrl Pts',(8.90480153282399,-5.51577199686659,-1.08039497961707));
#42392=CARTESIAN_POINT('Ctrl Pts',(9.06390140508865,-2.07287116795179,-5.22438505036529));
#42393=CARTESIAN_POINT('Ctrl Pts',(9.22300127735332,3.27461088827806,-4.5681415875351));
#42394=CARTESIAN_POINT('Ctrl Pts',(9.38210114961799,5.6133374940962,0.285370304632429));
#42395=CARTESIAN_POINT('Ctrl Pts',(9.54120102188265,2.79445595758408,4.87668021655706));
#42396=CARTESIAN_POINT('Ctrl Pts',(9.70030089414733,-2.59200837889555,4.98723235844268));
#42397=CARTESIAN_POINT('Ctrl Pts',(9.85940076641198,-5.59690140702245,0.515449971795401));
#42398=CARTESIAN_POINT('Ctrl Pts',(10.0185006386767,-3.45928798529643,-4.42993461220659));
#42399=CARTESIAN_POINT('Ctrl Pts',(10.1776005109413,1.8567646267687,-5.30503714914959));
#42400=CARTESIAN_POINT('Ctrl Pts',(10.336700383206,5.46679753703149,-1.30580194604518));
#42401=CARTESIAN_POINT('Ctrl Pts',(10.4958002554707,4.05386514039572,3.89322121880048));
#42402=CARTESIAN_POINT('Ctrl Pts',(10.6549001277353,-1.0838117383589,5.51510164426666));
#42403=CARTESIAN_POINT('Ctrl Pts',(10.814,-5.2256681707136,2.06963431610236));
#42404=CARTESIAN_POINT('Ctrl Pts',(10.9730998722647,-4.56611212258392,-3.27744017919686));
#42405=CARTESIAN_POINT('Ctrl Pts',(11.1321997445293,0.288847657594046,-5.61315963107182));
#42406=CARTESIAN_POINT('Ctrl Pts',(11.291299616794,4.87841041667205,-2.79143437000195));
#42407=CARTESIAN_POINT('Ctrl Pts',(11.4503994890586,4.98562568152621,2.59509742918897));
#42408=CARTESIAN_POINT('Ctrl Pts',(11.6094993613234,0.511982641443287,5.59721963617958));
#42409=CARTESIAN_POINT('Ctrl Pts',(11.768599233588,-4.43207674391413,3.45654304602252));
#42410=CARTESIAN_POINT('Ctrl Pts',(11.9276991058527,-5.30388590846277,-1.86005073611213));
#42411=CARTESIAN_POINT('Ctrl Pts',(12.0867989781173,-1.3024150218019,-5.46760532762948));
#42412=CARTESIAN_POINT('Ctrl Pts',(12.245898850382,3.89573171089409,-4.05145272654532));
#42413=CARTESIAN_POINT('Ctrl Pts',(12.4049987226467,5.51442934797128,1.08722841817489));
#42414=CARTESIAN_POINT('Ctrl Pts',(12.5640985949113,2.06639633867842,5.22694863955418));
#42415=CARTESIAN_POINT('Ctrl Pts',(12.723198467176,-3.28026757718596,4.56408214385256));
#42416=CARTESIAN_POINT('Ctrl Pts',(12.8822983394407,-5.61298083152789,-0.292327274083852));
#42417=CARTESIAN_POINT('Ctrl Pts',(13.0413982117053,-2.7884093768757,-4.88013419276635));
#42418=CARTESIAN_POINT('Ctrl Pts',(13.20049808397,2.59818100859393,-4.98402581747495));
#42419=CARTESIAN_POINT('Ctrl Pts',(13.3595979562347,5.59754429612724,-0.508498385918783));
#42420=CARTESIAN_POINT('Ctrl Pts',(13.5186978284993,3.45378033405525,4.43418510470741));
#42421=CARTESIAN_POINT('Ctrl Pts',(13.677797700764,-1.8633046031804,5.30279411274442));
#42422=CARTESIAN_POINT('Ctrl Pts',(13.8368975730287,-5.46847146218773,1.29890973526275));
#42423=CARTESIAN_POINT('Ctrl Pts',(13.9959974452934,-4.04892288508812,-3.89801475438421));
#42424=CARTESIAN_POINT('Ctrl Pts',(14.155097317558,1.09042253632216,-5.51418813337035));
#42425=CARTESIAN_POINT('Ctrl Pts',(14.3141971898227,5.22865304566401,-2.06232682721993));
#42426=CARTESIAN_POINT('Ctrl Pts',(14.4732970620873,4.56123314753381,3.28149866079956));
#42427=CARTESIAN_POINT('Ctrl Pts',(14.632396934352,-0.294233619083599,5.61588016610892));
#42428=CARTESIAN_POINT('Ctrl Pts',(14.7914968066167,-4.8849300263271,2.77927392804497));
#42429=CARTESIAN_POINT('Ctrl Pts',(14.9240800335039,-4.9608507571786,-1.69320253556725));
#42430=CARTESIAN_POINT('Ctrl Pts',(15.0301466150137,-2.74612663271131,-4.1138412539133));
#42431=CARTESIAN_POINT('Ctrl Pts',(15.0831799057686,-1.21552226347405,-4.66163486451439));
#42432=CARTESIAN_POINT('Ctrl Pts',(15.109696551146,-0.426999077480991,-4.73277675237597));
#42433=CARTESIAN_POINT('Ctrl Pts',(2.33230344885397,2.64867169498373,-3.71434815979763));
#42434=CARTESIAN_POINT('Ctrl Pts',(2.35882009423141,3.26751551502674,-3.2730556262908));
#42435=CARTESIAN_POINT('Ctrl Pts',(2.41185338498631,4.27009538784955,-2.07700006020815));
#42436=CARTESIAN_POINT('Ctrl Pts',(2.51791996649608,4.9313863127868,1.00254546187589));
#42437=CARTESIAN_POINT('Ctrl Pts',(2.65050319338331,2.69982160254977,4.67145329603068));
#42438=CARTESIAN_POINT('Ctrl Pts',(2.80960306564797,-2.47929430849091,4.7957721205305));
#42439=CARTESIAN_POINT('Ctrl Pts',(2.96870293791264,-5.37042774152615,0.507225926118294));
#42440=CARTESIAN_POINT('Ctrl Pts',(3.12780281017731,-3.33225778313177,-4.24408655470942));
#42441=CARTESIAN_POINT('Ctrl Pts',(3.28690268244198,1.7702934964039,-5.09757818836783));
#42442=CARTESIAN_POINT('Ctrl Pts',(3.44600255470665,5.24488984255953,-1.26646151440794));
#42443=CARTESIAN_POINT('Ctrl Pts',(3.60510242697131,3.90113546819821,3.727834258553));
#42444=CARTESIAN_POINT('Ctrl Pts',(3.76420229923598,-1.02741042725242,5.29718816930885));
#42445=CARTESIAN_POINT('Ctrl Pts',(3.92330217150065,-5.01176145386385,1.99929028661086));
#42446=CARTESIAN_POINT('Ctrl Pts',(4.08240204376532,-4.39134289523202,-3.13551612379576));
#42447=CARTESIAN_POINT('Ctrl Pts',(4.24150191602998,0.263952652679065,-5.38940340801339));
#42448=CARTESIAN_POINT('Ctrl Pts',(4.40060178829465,4.6766971232696,-2.69141827127356));
#42449=CARTESIAN_POINT('Ctrl Pts',(4.55970166055932,4.79244547612395,2.4794679734953));
#42450=CARTESIAN_POINT('Ctrl Pts',(4.71880153282398,0.504824447624409,5.37219136940268));
#42451=CARTESIAN_POINT('Ctrl Pts',(4.87790140508866,-4.24663194482322,3.32887231216658));
#42452=CARTESIAN_POINT('Ctrl Pts',(5.03700127735332,-5.09622925307003,-1.77305698176578));
#42453=CARTESIAN_POINT('Ctrl Pts',(5.196101149618,-1.26334317768426,-5.24587894609));
#42454=CARTESIAN_POINT('Ctrl Pts',(5.35520102188265,3.73031862332518,-3.89871814372373));
#42455=CARTESIAN_POINT('Ctrl Pts',(5.51430089414733,5.29651502097057,1.03063585665488));
#42456=CARTESIAN_POINT('Ctrl Pts',(5.67340076641199,1.99620376860123,5.01302820681081));
#42457=CARTESIAN_POINT('Ctrl Pts',(5.83250063867667,-3.13824561878099,4.38938441341275));
#42458=CARTESIAN_POINT('Ctrl Pts',(5.99160051094132,-5.38923379625736,-0.267283345632638));
#42459=CARTESIAN_POINT('Ctrl Pts',(6.15070038320601,-2.68852322772634,-4.67836767357019));
#42460=CARTESIAN_POINT('Ctrl Pts',(6.30980025547066,2.48243774729798,-4.79090639079288));
#42461=CARTESIAN_POINT('Ctrl Pts',(6.46890012773534,5.37250235388013,-0.501497458319054));
#42462=CARTESIAN_POINT('Ctrl Pts',(6.62799999999999,3.32624130188175,4.24869392099209));
#42463=CARTESIAN_POINT('Ctrl Pts',(6.78709987226468,-1.77621390038207,5.09512957743621));
#42464=CARTESIAN_POINT('Ctrl Pts',(6.94619974452933,-5.24666046606172,1.26009332533163));
#42465=CARTESIAN_POINT('Ctrl Pts',(7.10529961679401,-3.89640655350851,-3.73273320808705));
#42466=CARTESIAN_POINT('Ctrl Pts',(7.26439948905867,1.03391682503877,-5.2958754924732));
#42467=CARTESIAN_POINT('Ctrl Pts',(7.42349936132334,5.01426385880808,-1.99309788712159));
#42468=CARTESIAN_POINT('Ctrl Pts',(7.582599233588,4.38743946674697,3.14096420844982));
#42469=CARTESIAN_POINT('Ctrl Pts',(7.74169910585268,-0.270621875044055,
5.38906717659815));
#42470=CARTESIAN_POINT('Ctrl Pts',(7.90079897811734,-4.68003228722435,2.68562451279868));
#42471=CARTESIAN_POINT('Ctrl Pts',(8.05989885038201,-4.78936762706038,-2.4854051915197));
#42472=CARTESIAN_POINT('Ctrl Pts',(8.21899872264668,-0.498169149732212,
-5.37281199479628));
#42473=CARTESIAN_POINT('Ctrl Pts',(8.37809859491134,4.25075367886359,-3.32360864044003));
#42474=CARTESIAN_POINT('Ctrl Pts',(8.53719846717601,5.0940282530611,1.77936994191459));
#42475=CARTESIAN_POINT('Ctrl Pts',(8.69629833944068,1.25684282946048,5.24744007447532));
#42476=CARTESIAN_POINT('Ctrl Pts',(8.85539821170534,-3.73514627691857,3.89409341480108));
#42477=CARTESIAN_POINT('Ctrl Pts',(9.01449808397002,-5.29523397510635,-1.03719736890007));
#42478=CARTESIAN_POINT('Ctrl Pts',(9.17359795623469,-1.98999121805471,-5.01549760096096));
#42479=CARTESIAN_POINT('Ctrl Pts',(9.33269782849935,3.14368158087639,-4.38549282877422));
#42480=CARTESIAN_POINT('Ctrl Pts',(9.49179770076402,5.38889849496356,0.273960296661032));
#42481=CARTESIAN_POINT('Ctrl Pts',(9.65089757302868,2.68272476399379,4.68169510688832));
#42482=CARTESIAN_POINT('Ctrl Pts',(9.80999744529335,-2.48837168024444,4.78782702424569));
#42483=CARTESIAN_POINT('Ctrl Pts',(9.96909731755802,-5.37311957467096,0.494840650532518));
#42484=CARTESIAN_POINT('Ctrl Pts',(10.1281971898227,-3.32097470305603,-4.2528118057421));
#42485=CARTESIAN_POINT('Ctrl Pts',(10.2872970620874,1.78252530036171,-5.09292497357333));
#42486=CARTESIAN_POINT('Ctrl Pts',(10.446396934352,5.24821766917881,-1.2535918514011));
#42487=CARTESIAN_POINT('Ctrl Pts',(10.6054968066167,3.89177878166777,3.73755791249323));
#42488=CARTESIAN_POINT('Ctrl Pts',(10.7645966788814,-1.04047751481342,5.29459042532502));
#42489=CARTESIAN_POINT('Ctrl Pts',(10.923696551146,-5.01672941809669,1.98688378578681));
#42490=CARTESIAN_POINT('Ctrl Pts',(11.0827964234107,-4.383544508255,-3.14639774778959));
#42491=CARTESIAN_POINT('Ctrl Pts',(11.2418962956754,0.277298614045473,-5.38872774346583));
#42492=CARTESIAN_POINT('Ctrl Pts',(11.40099616794,4.68335612812668,-2.67982398904647));
#42493=CARTESIAN_POINT('Ctrl Pts',(11.5600960402047,4.78628458735744,2.49133722053032));
#42494=CARTESIAN_POINT('Ctrl Pts',(11.7191959124694,0.491511955021929,5.37342508001921));
#42495=CARTESIAN_POINT('Ctrl Pts',(11.878295784734,-4.25486828824417,3.31833951514198));
#42496=CARTESIAN_POINT('Ctrl Pts',(12.0373956569987,-5.09181976313282,-1.78568002065311));
#42497=CARTESIAN_POINT('Ctrl Pts',(12.1964955292634,-1.25034034710862,-5.24899316175204));
#42498=CARTESIAN_POINT('Ctrl Pts',(12.355595401528,3.73996802716727,-3.88946282375836));
#42499=CARTESIAN_POINT('Ctrl Pts',(12.5146952737927,5.29394500956333,1.04375758495663));
#42500=CARTESIAN_POINT('Ctrl Pts',(12.6737951460574,1.98377527294843,5.01795868974035));
#42501=CARTESIAN_POINT('Ctrl Pts',(12.832895018322,-3.14911209745843,4.38159569449818));
#42502=CARTESIAN_POINT('Ctrl Pts',(12.9919948905867,-5.38855609289356,-0.280639104455098));
#42503=CARTESIAN_POINT('Ctrl Pts',(13.1510947628514,-2.67691994471947,-4.68501098219699));
#42504=CARTESIAN_POINT('Ctrl Pts',(13.310194635116,2.4942975086712,-4.7847486909345));
#42505=CARTESIAN_POINT('Ctrl Pts',(13.4692945073807,5.37373675903462,-0.488167011060903));
#42506=CARTESIAN_POINT('Ctrl Pts',(13.6283943796454,3.31568726514309,4.25689235010001));
#42507=CARTESIAN_POINT('Ctrl Pts',(13.78749425191,-1.78880378781756,5.0907716208628));
#42508=CARTESIAN_POINT('Ctrl Pts',(13.9465941241747,-5.24982466550936,1.24697521301949));
#42509=CARTESIAN_POINT('Ctrl Pts',(14.1056939964394,-3.88703413336951,-3.74215978735286));
#42510=CARTESIAN_POINT('Ctrl Pts',(14.2647938687041,1.04682399215104,-5.2937134394856));
#42511=CARTESIAN_POINT('Ctrl Pts',(14.4238937409687,5.01959494829951,-1.97986847343797));
#42512=CARTESIAN_POINT('Ctrl Pts',(14.5829936132334,4.37886061006927,3.15029395845279));
#42513=CARTESIAN_POINT('Ctrl Pts',(14.742093485498,-0.282469227748196,5.39133950290171));
#42514=CARTESIAN_POINT('Ctrl Pts',(14.9011933577627,-4.68961506315326,2.66814976004653));
#42515=CARTESIAN_POINT('Ctrl Pts',(15.0337765846499,-4.76250024289745,-1.62550293923777));
#42516=CARTESIAN_POINT('Ctrl Pts',(15.1398431661597,-2.63632779849094,-3.94935686034355));
#42517=CARTESIAN_POINT('Ctrl Pts',(15.1928764569146,-1.16692183627285,-4.47524794863524));
#42518=CARTESIAN_POINT('Ctrl Pts',(15.2193931022921,-0.409926302918398,
-4.54354535865723));
#42519=CARTESIAN_POINT('Ctrl Pts',(2.442,2.53835875722685,-3.55965150255046));
#42520=CARTESIAN_POINT('Ctrl Pts',(2.46851664537744,3.13142872242371,-3.13673809691875));
#42521=CARTESIAN_POINT('Ctrl Pts',(2.52154993613233,4.09225274784706,-1.99049633126479));
#42522=CARTESIAN_POINT('Ctrl Pts',(2.62761651764211,4.7260019639421,0.960791047637318));
#42523=CARTESIAN_POINT('Ctrl Pts',(2.76019974452934,2.58737835299157,4.47689474139548));
#42524=CARTESIAN_POINT('Ctrl Pts',(2.919299616794,-2.37603566784794,4.59603588578678));
#42525=CARTESIAN_POINT('Ctrl Pts',(3.07839948905867,-5.14675801971775,0.48610077794589));
#42526=CARTESIAN_POINT('Ctrl Pts',(3.23749936132335,-3.19347457866112,-4.06732714098853));
#42527=CARTESIAN_POINT('Ctrl Pts',(3.396599233588,1.69656360505873,-4.88527221384132));
#42528=CARTESIAN_POINT('Ctrl Pts',(3.55569910585268,5.02644857336042,-1.21371541889335));
#42529=CARTESIAN_POINT('Ctrl Pts',(3.71479897811734,3.73865941844861,3.57257592687282));
#42530=CARTESIAN_POINT('Ctrl Pts',(3.87389885038201,-0.984620426994229,
5.07656875848712));
#42531=CARTESIAN_POINT('Ctrl Pts',(4.03299872264668,-4.80302960900762,1.91602304538856));
#42532=CARTESIAN_POINT('Ctrl Pts',(4.19209859491134,-4.2084504905643,-3.00492689461532));
#42533=CARTESIAN_POINT('Ctrl Pts',(4.35119846717601,0.252959447065525,-5.16494338006019));
#42534=CARTESIAN_POINT('Ctrl Pts',(4.51029833944068,4.48192017162094,-2.5793250070162));
#42535=CARTESIAN_POINT('Ctrl Pts',(4.66939821170534,4.59284779079654,2.37620209998279));
#42536=CARTESIAN_POINT('Ctrl Pts',(4.82849808397002,0.483799317188488,5.14844819531533));
#42537=CARTESIAN_POINT('Ctrl Pts',(4.98759795623468,-4.06976651967716,3.19023010714429));
#42538=CARTESIAN_POINT('Ctrl Pts',(5.14669782849936,-4.88397945954014,-1.69921199567735));
#42539=CARTESIAN_POINT('Ctrl Pts',(5.30579770076401,-1.21072695590433,-5.0273964823116));
#42540=CARTESIAN_POINT('Ctrl Pts',(5.46489757302869,3.57495682182765,-3.73634277167034));
#42541=CARTESIAN_POINT('Ctrl Pts',(5.62399744529335,5.07592364569998,0.98771152242332));
#42542=CARTESIAN_POINT('Ctrl Pts',(5.78309731755802,1.91306507591506,4.80424360372137));
#42543=CARTESIAN_POINT('Ctrl Pts',(5.94219718982269,-3.00754271050209,4.20657357637889));
#42544=CARTESIAN_POINT('Ctrl Pts',(6.10129706208735,-5.16478083236238,-0.256151421987276));
#42545=CARTESIAN_POINT('Ctrl Pts',(6.26039693435203,-2.57655053740016,-4.48352114617468));
#42546=CARTESIAN_POINT('Ctrl Pts',(6.41949680661669,2.37904818745876,-4.59137280590671));
#42547=CARTESIAN_POINT('Ctrl Pts',(6.57859667888136,5.14874622778692,-0.48061089166393));
#42548=CARTESIAN_POINT('Ctrl Pts',(6.73769655114603,3.18770867422774,4.07174261783812));
#42549=CARTESIAN_POINT('Ctrl Pts',(6.8967964234107,-1.70223743368489,4.8829255836368));
#42550=CARTESIAN_POINT('Ctrl Pts',(7.05589629567536,-5.02814545322706,1.20761245470185));
#42551=CARTESIAN_POINT('Ctrl Pts',(7.21499616794003,-3.73412745548863,-3.57727084299794));
#42552=CARTESIAN_POINT('Ctrl Pts',(7.3740960402047,0.990855843724147,-5.07531075254117));
#42553=CARTESIAN_POINT('Ctrl Pts',(7.53319591246937,4.80542779279021,-1.91008854942909));
#42554=CARTESIAN_POINT('Ctrl Pts',(7.69229578473403,4.20470963362949,3.01014807526144));
#42555=CARTESIAN_POINT('Ctrl Pts',(7.8513956569987,-0.25935090699094,5.16462115214535));
#42556=CARTESIAN_POINT('Ctrl Pts',(8.01049552926338,-4.48511643133383,2.57377254931078));
#42557=CARTESIAN_POINT('Ctrl Pts',(8.16959540152803,-4.58989812922139,-2.38189204237707));
#42558=CARTESIAN_POINT('Ctrl Pts',(8.32869527379272,-0.477421201803847,
-5.14904297265438));
#42559=CARTESIAN_POINT('Ctrl Pts',(8.48779514605736,4.07371659009023,-3.18518565892236));
#42560=CARTESIAN_POINT('Ctrl Pts',(8.64689501832206,4.8818701276596,1.70526203113781));
#42561=CARTESIAN_POINT('Ctrl Pts',(8.8059948905867,1.20449733678236,5.02889259219775));
#42562=CARTESIAN_POINT('Ctrl Pts',(8.96509476285138,-3.57958341137396,3.73191065530694));
#42563=CARTESIAN_POINT('Ctrl Pts',(9.12419463511603,-5.07469595334611,-0.993999758183069));
#42564=CARTESIAN_POINT('Ctrl Pts',(9.28329450738073,-1.90711126815764,-4.80661015155663));
#42565=CARTESIAN_POINT('Ctrl Pts',(9.44239437964536,3.01275227347471,-4.20284407001334));
#42566=CARTESIAN_POINT('Ctrl Pts',(9.60149425191006,5.16445949583093,0.26255028868963));
#42567=CARTESIAN_POINT('Ctrl Pts',(9.76059412417471,2.5709935704035,4.48670999721959));
#42568=CARTESIAN_POINT('Ctrl Pts',(9.91969399643938,-2.38473498159332,4.58842169004869));
#42569=CARTESIAN_POINT('Ctrl Pts',(10.0787938687041,-5.14933774231948,0.474231329269644));
#42570=CARTESIAN_POINT('Ctrl Pts',(10.2378937409687,-3.18266142081563,-4.07568899927763));
#42571=CARTESIAN_POINT('Ctrl Pts',(10.3969936132334,1.70828597395473,-4.88081279799705));
#42572=CARTESIAN_POINT('Ctrl Pts',(10.556093485498,5.02963780132612,-1.20138175675703));
#42573=CARTESIAN_POINT('Ctrl Pts',(10.7151933577627,3.72969242293982,3.58189460618598));
#42574=CARTESIAN_POINT('Ctrl Pts',(10.8742932300274,-0.997143291267936,
5.07407920638337));
#42575=CARTESIAN_POINT('Ctrl Pts',(11.0333931022921,-4.80779066547978,1.90413325547126));
#42576=CARTESIAN_POINT('Ctrl Pts',(11.1924929745567,-4.20097689392609,-3.01535531638232));
#42577=CARTESIAN_POINT('Ctrl Pts',(11.3515928468214,0.265749570496903,-5.16429585585985));
#42578=CARTESIAN_POINT('Ctrl Pts',(11.5106927190861,4.4883018395813,-2.56821360809099));
#42579=CARTESIAN_POINT('Ctrl Pts',(11.6697925913507,4.58694349318866,2.38757701187169));
#42580=CARTESIAN_POINT('Ctrl Pts',(11.8288924636154,0.471041268600573,5.14963052385883));
#42581=CARTESIAN_POINT('Ctrl Pts',(11.9879923358801,-4.07765983257421,3.18013598426144));
#42582=CARTESIAN_POINT('Ctrl Pts',(12.1470922081447,-4.87975361780286,-1.7113093051941));
#42583=CARTESIAN_POINT('Ctrl Pts',(12.3061920804094,-1.19826567241535,-5.0303809958746));
#42584=CARTESIAN_POINT('Ctrl Pts',(12.4652919526741,3.58420434344045,-3.72747292097139));
#42585=CARTESIAN_POINT('Ctrl Pts',(12.6243918249387,5.07346067115539,1.00028675173837));
#42586=CARTESIAN_POINT('Ctrl Pts',(12.7834916972034,1.90115420721842,4.80896873992654));
#42587=CARTESIAN_POINT('Ctrl Pts',(12.9425915694681,-3.01795661773088,4.19910924514379));
#42588=CARTESIAN_POINT('Ctrl Pts',(13.1016914417327,-5.16413135425925,-0.268950934826332));
#42589=CARTESIAN_POINT('Ctrl Pts',(13.2607913139974,-2.56543051256322,-4.48988777162764));
#42590=CARTESIAN_POINT('Ctrl Pts',(13.4198911862621,2.39041400874848,-4.58547156439403));
#42591=CARTESIAN_POINT('Ctrl Pts',(13.5789910585267,5.14992922194199,-0.467835636203029));
#42592=CARTESIAN_POINT('Ctrl Pts',(13.7380909307914,3.17759419623094,4.07959959549261));
#42593=CARTESIAN_POINT('Ctrl Pts',(13.8971908030561,-1.71430297245472,4.87874912898118));
#42594=CARTESIAN_POINT('Ctrl Pts',(14.0562906753207,-5.03117786883098,1.19504069077622));
#42595=CARTESIAN_POINT('Ctrl Pts',(14.2153905475854,-3.72514538165091,-3.58630482032152));
#42596=CARTESIAN_POINT('Ctrl Pts',(14.3744904198501,1.00322544797992,-5.07323874560084));
#42597=CARTESIAN_POINT('Ctrl Pts',(14.5335902921147,4.810536850935,-1.89741011965601));
#42598=CARTESIAN_POINT('Ctrl Pts',(14.6926901643794,4.19648807260473,3.01908925610601));
#42599=CARTESIAN_POINT('Ctrl Pts',(14.8517900366441,-0.270704836412793,
5.16679883969449));
#42600=CARTESIAN_POINT('Ctrl Pts',(15.0108899089087,-4.49430009997942,2.55702559204809));
#42601=CARTESIAN_POINT('Ctrl Pts',(15.143473135796,-4.56414972861631,-1.55780334290828));
#42602=CARTESIAN_POINT('Ctrl Pts',(15.2495397173057,-2.52652896427057,-3.78487246677379));
#42603=CARTESIAN_POINT('Ctrl Pts',(15.3025730080606,-1.11832140907164,-4.28886103275609));
#42604=CARTESIAN_POINT('Ctrl Pts',(15.3290896534381,-0.392853528355804,
-4.3543139649385));
#42605=CARTESIAN_POINT('',(15.,-0.444071852043585,-4.9220081460947));
#42606=CARTESIAN_POINT('Ctrl Pts',(15.,-3.64743349744463,2.4217429795102));
#42607=CARTESIAN_POINT('Ctrl Pts',(15.,-3.7082898637292,2.34260869181596));
#42608=CARTESIAN_POINT('Ctrl Pts',(15.,-3.76611345131222,2.26145305032969));
#42609=CARTESIAN_POINT('Ctrl Pts',(15.,-3.82075032258788,2.17837970357634));
#42610=CARTESIAN_POINT('Ctrl Pts',(15.,-3.89159249211755,2.07066679877978));
#42611=CARTESIAN_POINT('Ctrl Pts',(15.,-3.95707930631556,1.95973124308563));
#42612=CARTESIAN_POINT('Ctrl Pts',(15.,-4.0172930750217,1.84600005851335));
#42613=CARTESIAN_POINT('Ctrl Pts',(15.,-4.07888289152636,1.72966980815403));
#42614=CARTESIAN_POINT('Ctrl Pts',(15.,-4.13495615398629,1.61041413582088));
#42615=CARTESIAN_POINT('Ctrl Pts',(15.,-4.18555885319492,1.48865487734055));
#42616=CARTESIAN_POINT('Ctrl Pts',(15.,-4.23700268046163,1.36487171242361));
#42617=CARTESIAN_POINT('Ctrl Pts',(15.,-4.28279281221221,1.23850035311616));
#42618=CARTESIAN_POINT('Ctrl Pts',(15.,-4.32293081471277,1.10995769229629));
#42619=CARTESIAN_POINT('Ctrl Pts',(15.,-4.33504493319114,1.07116201424341));
#42620=CARTESIAN_POINT('Ctrl Pts',(15.,-4.34664386538786,1.03216841226631));
#42621=CARTESIAN_POINT('Ctrl Pts',(15.,-4.35772678427811,0.992988037261006));
#42622=CARTESIAN_POINT('Ctrl Pts',(15.,-4.36488134209109,0.967695218565394));
#42623=CARTESIAN_POINT('Ctrl Pts',(15.,-4.3718208521776,0.942324563071167));
#42624=CARTESIAN_POINT('Ctrl Pts',(15.,-4.37854500096099,0.916879049181161));
#42625=CARTESIAN_POINT('Ctrl Pts',(15.,-4.38421840264999,0.895409770893104));
#42626=CARTESIAN_POINT('Ctrl Pts',(15.,-4.38973902219339,0.873884734398618));
#42627=CARTESIAN_POINT('Ctrl Pts',(15.,-4.3951011031017,0.852328924497718));
#42628=CARTESIAN_POINT('Ctrl Pts',(15.,-4.42797349404255,0.720180413084934));
#42629=CARTESIAN_POINT('Ctrl Pts',(15.,-4.45494081833527,0.58669596358257));
#42630=CARTESIAN_POINT('Ctrl Pts',(15.,-4.47607666705785,0.452331314099685));
#42631=CARTESIAN_POINT('Ctrl Pts',(15.,-4.49752457608506,0.315982837328957));
#42632=CARTESIAN_POINT('Ctrl Pts',(15.,-4.51296775060728,0.178727229649941));
#42633=CARTESIAN_POINT('Ctrl Pts',(15.,-4.52243514398287,0.0410146220670506));
#42634=CARTESIAN_POINT('Ctrl Pts',(15.,-4.53194192100607,-0.0972708596527243));
#42635=CARTESIAN_POINT('Ctrl Pts',(15.,-4.53542324150019,-0.236017985118476));
#42636=CARTESIAN_POINT('Ctrl Pts',(15.,-4.53285786554154,-0.374785067473027));
#42637=CARTESIAN_POINT('Ctrl Pts',(15.,-4.53031342129,-0.512419905676942));
#42638=CARTESIAN_POINT('Ctrl Pts',(15.,-4.52182060592257,-0.650075216592292));
#42639=CARTESIAN_POINT('Ctrl Pts',(15.,-4.50730773271262,-0.787321336183077));
#42640=CARTESIAN_POINT('Ctrl Pts',(15.,-4.50515840901136,-0.807647176109848));
#42641=CARTESIAN_POINT('Ctrl Pts',(15.,-4.50287695500964,-0.82796403036086));
#42642=CARTESIAN_POINT('Ctrl Pts',(15.,-4.50046304054395,-0.848270488261463));
#42643=CARTESIAN_POINT('Ctrl Pts',(15.,-4.49855407636242,-0.864329176892247));
#42644=CARTESIAN_POINT('Ctrl Pts',(15.,-4.49656237244444,-0.880380229709894));
#42645=CARTESIAN_POINT('Ctrl Pts',(15.,-4.49448916865398,-0.896413081113118));
#42646=CARTESIAN_POINT('Ctrl Pts',(15.,-4.47634947236908,-1.03669405897637));
#42647=CARTESIAN_POINT('Ctrl Pts',(15.,-4.4519508282184,-1.17578554412336));
#42648=CARTESIAN_POINT('Ctrl Pts',(15.,-4.42132243491177,-1.3132290481336));
#42649=CARTESIAN_POINT('Ctrl Pts',(15.,-4.39075380118495,-1.45040438378239));
#42650=CARTESIAN_POINT('Ctrl Pts',(15.,-4.35397977833926,-1.58593903131621));
#42651=CARTESIAN_POINT('Ctrl Pts',(15.,-4.31097798157061,-1.71938254118705));
#42652=CARTESIAN_POINT('Ctrl Pts',(15.,-4.2687043897354,-1.85056627985004));
#42653=CARTESIAN_POINT('Ctrl Pts',(15.,-4.22041211971183,-1.97972990602547));
#42654=CARTESIAN_POINT('Ctrl Pts',(15.,-4.16603015137339,-2.10643831260173));
#42655=CARTESIAN_POINT('Ctrl Pts',(15.,-4.15802001293815,-2.12510170248253));
#42656=CARTESIAN_POINT('Ctrl Pts',(15.,-4.14987766647486,-2.14371179984538));
#42657=CARTESIAN_POINT('Ctrl Pts',(15.,-4.14160279252619,-2.16226718465083));
#42658=CARTESIAN_POINT('Ctrl Pts',(15.,-4.10146980039451,-2.25226047240565));
#42659=CARTESIAN_POINT('Ctrl Pts',(15.,-4.05822043039043,-2.34096727307218));
#42660=CARTESIAN_POINT('Ctrl Pts',(15.,-4.01198020214139,-2.42828555150392));
#42661=CARTESIAN_POINT('Ctrl Pts',(15.,-3.99642623237433,-2.45765707310465));
#42662=CARTESIAN_POINT('Ctrl Pts',(15.,-3.98053375519778,-2.48687143593773));
#42663=CARTESIAN_POINT('Ctrl Pts',(15.,-3.96430725035697,-2.51592458767279));
#42664=CARTESIAN_POINT('Ctrl Pts',(15.,-3.95490325737157,-2.53276220229163));
#42665=CARTESIAN_POINT('Ctrl Pts',(15.,-3.94538617715611,-2.54954721951204));
#42666=CARTESIAN_POINT('Ctrl Pts',(15.,-3.93575967760122,-2.56627394730149));
#42667=CARTESIAN_POINT('Ctrl Pts',(15.,-3.86759024667037,-2.68472318300139));
#42668=CARTESIAN_POINT('Ctrl Pts',(15.,-3.79413538181915,-2.79990975721909));
#42669=CARTESIAN_POINT('Ctrl Pts',(15.,-3.71581656760059,-2.9116041082618));
#42670=CARTESIAN_POINT('Ctrl Pts',(15.,-3.63503278498645,-3.02681387316811));
#42671=CARTESIAN_POINT('Ctrl Pts',(15.,-3.5490737856704,-3.13830875738446));
#42672=CARTESIAN_POINT('Ctrl Pts',(15.,-3.45834874984291,-3.24582141311442));
#42673=CARTESIAN_POINT('Ctrl Pts',(15.,-3.36674247041888,-3.35437837638909));
#42674=CARTESIAN_POINT('Ctrl Pts',(15.,-3.2702766055505,-3.45887601759371));
#42675=CARTESIAN_POINT('Ctrl Pts',(15.,-3.16932511812227,-3.55901400521376));
#42676=CARTESIAN_POINT('Ctrl Pts',(15.,-3.09115822859782,-3.63655100060535));
#42677=CARTESIAN_POINT('Ctrl Pts',(15.,-3.01030098340661,-3.71147378219999));
#42678=CARTESIAN_POINT('Ctrl Pts',(15.,-2.92691083995722,-3.78362897614142));
#42679=CARTESIAN_POINT('Ctrl Pts',(15.,-2.88521576823253,-3.81970657311214));
#42680=CARTESIAN_POINT('Ctrl Pts',(15.,-2.84288727059802,-3.85509206296282));
#42681=CARTESIAN_POINT('Ctrl Pts',(15.,-2.79994392620086,-3.88976489887852));
#42682=CARTESIAN_POINT('Ctrl Pts',(15.,-2.77692979182587,-3.90834671443407));
#42683=CARTESIAN_POINT('Ctrl Pts',(15.,-2.75373905644439,-3.92672383301606));
#42684=CARTESIAN_POINT('Ctrl Pts',(15.,-2.73037450355138,-3.94489297201166));
#42685=CARTESIAN_POINT('Ctrl Pts',(15.,-2.71464882485127,-3.95712184039235));
#42686=CARTESIAN_POINT('Ctrl Pts',(15.,-2.69885251683566,-3.96925018247846));
#42687=CARTESIAN_POINT('Ctrl Pts',(15.,-2.68298667657367,-3.9812772548001));
#42688=CARTESIAN_POINT('Ctrl Pts',(15.,-2.67843952821254,-3.98472421262228));
#42689=CARTESIAN_POINT('Ctrl Pts',(15.,-2.67388666838095,-3.98816285215109));
#42690=CARTESIAN_POINT('Ctrl Pts',(15.,-2.66932812263831,-3.99159315574737));
#42691=CARTESIAN_POINT('Ctrl Pts',(15.,-2.55443810398459,-4.07804784248627));
#42692=CARTESIAN_POINT('Ctrl Pts',(15.,-2.43593971533117,-4.15921041969436));
#42693=CARTESIAN_POINT('Ctrl Pts',(15.,-2.31421368015325,-4.23496729168326));
#42694=CARTESIAN_POINT('Ctrl Pts',(15.,-2.19161738873209,-4.31126577246374));
#42695=CARTESIAN_POINT('Ctrl Pts',(15.,-2.06574656365596,-4.38208139752043));
#42696=CARTESIAN_POINT('Ctrl Pts',(15.,-1.93695462293276,-4.44725913313952));
#42697=CARTESIAN_POINT('Ctrl Pts',(15.,-1.87847558199184,-4.47685362056088));
#42698=CARTESIAN_POINT('Ctrl Pts',(15.,-1.81939386822387,-4.50528518256321));
#42699=CARTESIAN_POINT('Ctrl Pts',(15.,-1.75974066697738,-4.53253631662746));
#42700=CARTESIAN_POINT('Ctrl Pts',(15.,-1.72832141961374,-4.54688944611948));
#42701=CARTESIAN_POINT('Ctrl Pts',(15.,-1.69674361756834,-4.56091507907796));
#42702=CARTESIAN_POINT('Ctrl Pts',(15.,-1.66501170956427,-4.57461043436351));
#42703=CARTESIAN_POINT('Ctrl Pts',(15.,-1.64184014412444,-4.58461118254354));
#42704=CARTESIAN_POINT('Ctrl Pts',(15.,-1.6185938221782,-4.59443257119121));
#42705=CARTESIAN_POINT('Ctrl Pts',(15.,-1.59528099966613,-4.60407127664067));
#42706=CARTESIAN_POINT('Ctrl Pts',(15.,-1.46028192957332,-4.65988675208995));
#42707=CARTESIAN_POINT('Ctrl Pts',(15.,-1.32298927848311,-4.70960834354769));
#42708=CARTESIAN_POINT('Ctrl Pts',(15.,-1.18377213314752,-4.75309202784066));
#42709=CARTESIAN_POINT('Ctrl Pts',(15.,-1.04542344044048,-4.79630445588977));
#42710=CARTESIAN_POINT('Ctrl Pts',(15.,-0.90517353780007,-4.83335688725323));
#42711=CARTESIAN_POINT('Ctrl Pts',(15.,-0.763360003752109,-4.86406332913526));
#42712=CARTESIAN_POINT('Ctrl Pts',(15.,-0.657753741735435,-4.88692992341883));
#42713=CARTESIAN_POINT('Ctrl Pts',(15.,-0.551279803770889,-4.90627644088498));
#42714=CARTESIAN_POINT('Ctrl Pts',(15.,-0.444071852043585,-4.9220081460947));
#42715=CARTESIAN_POINT('Ctrl Pts',(15.,-0.444071852043585,-4.9220081460947));
#42716=CARTESIAN_POINT('Ctrl Pts',(14.9734833546226,-1.26412269067527,-4.84802178039354));
#42717=CARTESIAN_POINT('Ctrl Pts',(14.9469667092451,-2.06002407880351,-4.56317371393828));
#42718=CARTESIAN_POINT('Ctrl Pts',(14.9204500638677,-2.74588424843362,-4.10607174126237));
#42719=CARTESIAN_POINT('Ctrl Pts',(14.8939334184902,-3.43174441806373,-3.64896976858645));
#42720=CARTESIAN_POINT('Ctrl Pts',(14.8674167731128,-4.00756336919571,-3.01961388968989));
#42721=CARTESIAN_POINT('Ctrl Pts',(14.8409001277353,-4.3861789178198,-2.28995662189616));
#42722=CARTESIAN_POINT('Ctrl Pts',(14.8153735700425,-4.75065758802023,-1.58754354976006));
#42723=CARTESIAN_POINT('Ctrl Pts',(14.7898470123497,-4.93238442199734,-0.792179429297219));
#42724=CARTESIAN_POINT('Ctrl Pts',(14.7643204546569,-4.93235156762733,0.00248647065513752));
#42725=CARTESIAN_POINT('Origin',(15.,4.,0.));
#42726=CARTESIAN_POINT('Origin',(15.,0.,0.));
#42727=CARTESIAN_POINT('',(15.,-4.,-4.89858719658941E-16));
#42728=CARTESIAN_POINT('Origin',(15.,0.,0.));
#42729=CARTESIAN_POINT('Ctrl Pts',(26.5,4.59649122554347,-5.29039824318981));
#42730=CARTESIAN_POINT('Ctrl Pts',(26.25,4.59649122554347,-5.29039824318981));
#42731=CARTESIAN_POINT('Ctrl Pts',(26.5,4.91129522759113,-5.10151584196121));
#42732=CARTESIAN_POINT('Ctrl Pts',(26.25,4.91129522759113,-5.10151584196121));
#42733=CARTESIAN_POINT('Ctrl Pts',(26.5,5.25043192007604,-5.1048615648549));
#42734=CARTESIAN_POINT('Ctrl Pts',(26.25,5.25043192007604,-5.1048615648549));
#42735=CARTESIAN_POINT('',(26.5,4.59649122554347,-5.29039824318981));
#42736=CARTESIAN_POINT('',(26.5,5.25043192007604,-5.1048615648549));
#42737=CARTESIAN_POINT('Ctrl Pts',(26.5,4.59649122554347,-5.29039824318981));
#42738=CARTESIAN_POINT('Ctrl Pts',(26.5,4.91129522759113,-5.10151584196121));
#42739=CARTESIAN_POINT('Ctrl Pts',(26.5,5.25043192007604,-5.1048615648549));
#42740=CARTESIAN_POINT('',(26.25,4.59649122554347,-5.29039824318981));
#42741=CARTESIAN_POINT('',(26.5,4.59649122554347,-5.29039824318981));
#42742=CARTESIAN_POINT('',(26.25,5.25043192007604,-5.1048615648549));
#42743=CARTESIAN_POINT('Ctrl Pts',(26.25,4.59649122554347,-5.29039824318981));
#42744=CARTESIAN_POINT('Ctrl Pts',(26.25,4.91129522759113,-5.10151584196121));
#42745=CARTESIAN_POINT('Ctrl Pts',(26.25,5.25043192007604,-5.1048615648549));
#42746=CARTESIAN_POINT('',(26.5,5.25043192007604,-5.1048615648549));
#42747=CARTESIAN_POINT('Ctrl Pts',(26.5,4.13766826737842,-5.75287126208542));
#42748=CARTESIAN_POINT('Ctrl Pts',(26.25,4.13766826737842,-5.75287126208542));
#42749=CARTESIAN_POINT('Ctrl Pts',(26.5,4.30601993948832,-5.46468101482289));
#42750=CARTESIAN_POINT('Ctrl Pts',(26.25,4.30601993948832,-5.46468101482289));
#42751=CARTESIAN_POINT('Ctrl Pts',(26.5,4.59649122554347,-5.29039824318981));
#42752=CARTESIAN_POINT('Ctrl Pts',(26.25,4.59649122554347,-5.29039824318981));
#42753=CARTESIAN_POINT('',(26.5,4.13766826737842,-5.75287126208542));
#42754=CARTESIAN_POINT('Ctrl Pts',(26.5,4.13766826737842,-5.75287126208542));
#42755=CARTESIAN_POINT('Ctrl Pts',(26.5,4.30601993948832,-5.46468101482289));
#42756=CARTESIAN_POINT('Ctrl Pts',(26.5,4.59649122554347,-5.29039824318981));
#42757=CARTESIAN_POINT('',(26.25,4.13766826737842,-5.75287126208542));
#42758=CARTESIAN_POINT('',(26.5,4.13766826737842,-5.75287126208542));
#42759=CARTESIAN_POINT('Ctrl Pts',(26.25,4.13766826737842,-5.75287126208542));
#42760=CARTESIAN_POINT('Ctrl Pts',(26.25,4.30601993948832,-5.46468101482289));
#42761=CARTESIAN_POINT('Ctrl Pts',(26.25,4.59649122554347,-5.29039824318981));
#42762=CARTESIAN_POINT('Ctrl Pts',(26.5,3.99304081447426,-6.39084371396902));
#42763=CARTESIAN_POINT('Ctrl Pts',(26.25,3.99304081447426,-6.39084371396902));
#42764=CARTESIAN_POINT('Ctrl Pts',(26.5,3.96931659526851,-6.04106150934795));
#42765=CARTESIAN_POINT('Ctrl Pts',(26.25,3.96931659526851,-6.04106150934795));
#42766=CARTESIAN_POINT('Ctrl Pts',(26.5,4.13766826737842,-5.75287126208542));
#42767=CARTESIAN_POINT('Ctrl Pts',(26.25,4.13766826737842,-5.75287126208542));
#42768=CARTESIAN_POINT('',(26.5,3.99304081447426,-6.39084371396902));
#42769=CARTESIAN_POINT('Ctrl Pts',(26.5,3.99304081447426,-6.39084371396902));
#42770=CARTESIAN_POINT('Ctrl Pts',(26.5,3.96931659526851,-6.04106150934795));
#42771=CARTESIAN_POINT('Ctrl Pts',(26.5,4.13766826737842,-5.75287126208542));
#42772=CARTESIAN_POINT('',(26.25,3.99304081447426,-6.39084371396902));
#42773=CARTESIAN_POINT('',(26.5,3.99304081447426,-6.39084371396902));
#42774=CARTESIAN_POINT('Ctrl Pts',(26.25,3.99304081447426,-6.39084371396902));
#42775=CARTESIAN_POINT('Ctrl Pts',(26.25,3.96931659526851,-6.04106150934795));
#42776=CARTESIAN_POINT('Ctrl Pts',(26.25,4.13766826737842,-5.75287126208542));
#42777=CARTESIAN_POINT('Ctrl Pts',(26.5,4.22024719228052,-7.07976255996445));
#42778=CARTESIAN_POINT('Ctrl Pts',(26.25,4.22024719228052,-7.07976255996445));
#42779=CARTESIAN_POINT('Ctrl Pts',(26.5,4.01676516145641,-6.74062584192426));
#42780=CARTESIAN_POINT('Ctrl Pts',(26.25,4.01676516145641,-6.74062584192426));
#42781=CARTESIAN_POINT('Ctrl Pts',(26.5,3.99304081447426,-6.39084371396902));
#42782=CARTESIAN_POINT('Ctrl Pts',(26.25,3.99304081447426,-6.39084371396902));
#42783=CARTESIAN_POINT('',(26.5,4.22024719228052,-7.07976255996445));
#42784=CARTESIAN_POINT('Ctrl Pts',(26.5,4.22024719228052,-7.07976255996445));
#42785=CARTESIAN_POINT('Ctrl Pts',(26.5,4.01676516145641,-6.74062584192426));
#42786=CARTESIAN_POINT('Ctrl Pts',(26.5,3.99304081447426,-6.39084371396902));
#42787=CARTESIAN_POINT('',(26.25,4.22024719228052,-7.07976255996445));
#42788=CARTESIAN_POINT('',(26.5,4.22024719228052,-7.07976255996445));
#42789=CARTESIAN_POINT('Ctrl Pts',(26.25,4.22024719228052,-7.07976255996445));
#42790=CARTESIAN_POINT('Ctrl Pts',(26.25,4.01676516145641,-6.74062584192426));
#42791=CARTESIAN_POINT('Ctrl Pts',(26.25,3.99304081447426,-6.39084371396902));
#42792=CARTESIAN_POINT('Ctrl Pts',(26.5,4.70933386374015,-7.60017785881726));
#42793=CARTESIAN_POINT('Ctrl Pts',(26.25,4.70933386374015,-7.60017785881726));
#42794=CARTESIAN_POINT('Ctrl Pts',(26.5,4.42099179255547,-7.41433689375604));
#42795=CARTESIAN_POINT('Ctrl Pts',(26.25,4.42099179255547,-7.41433689375604));
#42796=CARTESIAN_POINT('Ctrl Pts',(26.5,4.22024719228052,-7.07976255996445));
#42797=CARTESIAN_POINT('Ctrl Pts',(26.25,4.22024719228052,-7.07976255996445));
#42798=CARTESIAN_POINT('',(26.5,4.70933386374015,-7.60017785881726));
#42799=CARTESIAN_POINT('Ctrl Pts',(26.5,4.70933386374015,-7.60017785881726));
#42800=CARTESIAN_POINT('Ctrl Pts',(26.5,4.42099179255547,-7.41433689375604));
#42801=CARTESIAN_POINT('Ctrl Pts',(26.5,4.22024719228052,-7.07976255996445));
#42802=CARTESIAN_POINT('',(26.25,4.70933386374015,-7.60017785881726));
#42803=CARTESIAN_POINT('',(26.5,4.70933386374015,-7.60017785881726));
#42804=CARTESIAN_POINT('Ctrl Pts',(26.25,4.70933386374015,-7.60017785881726));
#42805=CARTESIAN_POINT('Ctrl Pts',(26.25,4.42099179255547,-7.41433689375604));
#42806=CARTESIAN_POINT('Ctrl Pts',(26.25,4.22024719228052,-7.07976255996445));
#42807=CARTESIAN_POINT('Ctrl Pts',(26.5,5.33407558018978,-7.78480193252604));
#42808=CARTESIAN_POINT('Ctrl Pts',(26.25,5.33407558018978,-7.78480193252604));
#42809=CARTESIAN_POINT('Ctrl Pts',(26.5,4.99767624158819,-7.78601846610455));
#42810=CARTESIAN_POINT('Ctrl Pts',(26.25,4.99767624158819,-7.78601846610455));
#42811=CARTESIAN_POINT('Ctrl Pts',(26.5,4.70933386374015,-7.60017785881726));
#42812=CARTESIAN_POINT('Ctrl Pts',(26.25,4.70933386374015,-7.60017785881726));
#42813=CARTESIAN_POINT('',(26.5,5.33407558018978,-7.78480193252604));
#42814=CARTESIAN_POINT('Ctrl Pts',(26.5,5.33407558018978,-7.78480193252604));
#42815=CARTESIAN_POINT('Ctrl Pts',(26.5,4.99767624158819,-7.78601846610455));
#42816=CARTESIAN_POINT('Ctrl Pts',(26.5,4.70933386374015,-7.60017785881726));
#42817=CARTESIAN_POINT('',(26.25,5.33407558018978,-7.78480193252604));
#42818=CARTESIAN_POINT('',(26.5,5.33407558018978,-7.78480193252604));
#42819=CARTESIAN_POINT('Ctrl Pts',(26.25,5.33407558018978,-7.78480193252604));
#42820=CARTESIAN_POINT('Ctrl Pts',(26.25,4.99767624158819,-7.78601846610455));
#42821=CARTESIAN_POINT('Ctrl Pts',(26.25,4.70933386374015,-7.60017785881726));
#42822=CARTESIAN_POINT('Ctrl Pts',(26.5,5.97919566517507,-7.59835277734141));
#42823=CARTESIAN_POINT('Ctrl Pts',(26.25,5.97919566517507,-7.59835277734141));
#42824=CARTESIAN_POINT('Ctrl Pts',(26.5,5.67047484212553,-7.78358527117114));
#42825=CARTESIAN_POINT('Ctrl Pts',(26.25,5.67047484212553,-7.78358527117114));
#42826=CARTESIAN_POINT('Ctrl Pts',(26.5,5.33407558018978,-7.78480193252604));
#42827=CARTESIAN_POINT('Ctrl Pts',(26.25,5.33407558018978,-7.78480193252604));
#42828=CARTESIAN_POINT('',(26.5,5.97919566517507,-7.59835277734141));
#42829=CARTESIAN_POINT('Ctrl Pts',(26.5,5.97919566517507,-7.59835277734141));
#42830=CARTESIAN_POINT('Ctrl Pts',(26.5,5.67047484212553,-7.78358527117114));
#42831=CARTESIAN_POINT('Ctrl Pts',(26.5,5.33407558018978,-7.78480193252604));
#42832=CARTESIAN_POINT('',(26.25,5.97919566517507,-7.59835277734141));
#42833=CARTESIAN_POINT('',(26.5,5.97919566517507,-7.59835277734141));
#42834=CARTESIAN_POINT('Ctrl Pts',(26.25,5.97919566517507,-7.59835277734141));
#42835=CARTESIAN_POINT('Ctrl Pts',(26.25,5.67047484212553,-7.78358527117114));
#42836=CARTESIAN_POINT('Ctrl Pts',(26.25,5.33407558018978,-7.78480193252604));
#42837=CARTESIAN_POINT('Ctrl Pts',(26.5,6.56029043175907,-6.82259661503587));
#42838=CARTESIAN_POINT('Ctrl Pts',(26.25,6.56029043175907,-6.82259661503587));
#42839=CARTESIAN_POINT('Ctrl Pts',(26.5,6.45064133476,-7.31548537559045));
#42840=CARTESIAN_POINT('Ctrl Pts',(26.25,6.45064133476,-7.31548537559045));
#42841=CARTESIAN_POINT('Ctrl Pts',(26.5,5.97919566517507,-7.59835277734141));
#42842=CARTESIAN_POINT('Ctrl Pts',(26.25,5.97919566517507,-7.59835277734141));
#42843=CARTESIAN_POINT('',(26.5,6.56029043175907,-6.82259661503587));
#42844=CARTESIAN_POINT('Ctrl Pts',(26.5,6.56029043175907,-6.82259661503587));
#42845=CARTESIAN_POINT('Ctrl Pts',(26.5,6.45064133476,-7.31548537559045));
#42846=CARTESIAN_POINT('Ctrl Pts',(26.5,5.97919566517507,-7.59835277734141));
#42847=CARTESIAN_POINT('',(26.25,6.56029043175907,-6.82259661503587));
#42848=CARTESIAN_POINT('',(26.5,6.56029043175907,-6.82259661503587));
#42849=CARTESIAN_POINT('Ctrl Pts',(26.25,6.56029043175907,-6.82259661503587));
#42850=CARTESIAN_POINT('Ctrl Pts',(26.25,6.45064133476,-7.31548537559045));
#42851=CARTESIAN_POINT('Ctrl Pts',(26.25,5.97919566517507,-7.59835277734141));
#42852=CARTESIAN_POINT('Ctrl Pts',(26.5,6.33688598652166,-5.77461850881057));
#42853=CARTESIAN_POINT('Ctrl Pts',(26.25,6.33688598652166,-5.77461850881057));
#42854=CARTESIAN_POINT('Ctrl Pts',(26.5,6.66993957667428,-6.3297078257316));
#42855=CARTESIAN_POINT('Ctrl Pts',(26.25,6.66993957667428,-6.3297078257316));
#42856=CARTESIAN_POINT('Ctrl Pts',(26.5,6.56029043175907,-6.82259661503587));
#42857=CARTESIAN_POINT('Ctrl Pts',(26.25,6.56029043175907,-6.82259661503587));
#42858=CARTESIAN_POINT('',(26.5,6.33688598652166,-5.77461850881057));
#42859=CARTESIAN_POINT('Ctrl Pts',(26.5,6.33688598652166,-5.77461850881057));
#42860=CARTESIAN_POINT('Ctrl Pts',(26.5,6.66993957667428,-6.3297078257316));
#42861=CARTESIAN_POINT('Ctrl Pts',(26.5,6.56029043175907,-6.82259661503587));
#42862=CARTESIAN_POINT('',(26.25,6.33688598652166,-5.77461850881057));
#42863=CARTESIAN_POINT('',(26.5,6.33688598652166,-5.77461850881057));
#42864=CARTESIAN_POINT('Ctrl Pts',(26.25,6.33688598652166,-5.77461850881057));
#42865=CARTESIAN_POINT('Ctrl Pts',(26.25,6.66993957667428,-6.3297078257316));
#42866=CARTESIAN_POINT('Ctrl Pts',(26.25,6.56029043175907,-6.82259661503587));
#42867=CARTESIAN_POINT('Ctrl Pts',(26.5,5.87517352152691,-5.29465658348726));
#42868=CARTESIAN_POINT('Ctrl Pts',(26.25,5.87517352152691,-5.29465658348726));
#42869=CARTESIAN_POINT('Ctrl Pts',(26.5,6.16077826118914,-5.48110563325636));
#42870=CARTESIAN_POINT('Ctrl Pts',(26.25,6.16077826118914,-5.48110563325636));
#42871=CARTESIAN_POINT('Ctrl Pts',(26.5,6.33688598652166,-5.77461850881057));
#42872=CARTESIAN_POINT('Ctrl Pts',(26.25,6.33688598652166,-5.77461850881057));
#42873=CARTESIAN_POINT('',(26.5,5.87517352152691,-5.29465658348726));
#42874=CARTESIAN_POINT('Ctrl Pts',(26.5,5.87517352152691,-5.29465658348726));
#42875=CARTESIAN_POINT('Ctrl Pts',(26.5,6.16077826118914,-5.48110563325636));
#42876=CARTESIAN_POINT('Ctrl Pts',(26.5,6.33688598652166,-5.77461850881057));
#42877=CARTESIAN_POINT('',(26.25,5.87517352152691,-5.29465658348726));
#42878=CARTESIAN_POINT('',(26.5,5.87517352152691,-5.29465658348726));
#42879=CARTESIAN_POINT('Ctrl Pts',(26.25,5.87517352152691,-5.29465658348726));
#42880=CARTESIAN_POINT('Ctrl Pts',(26.25,6.16077826118914,-5.48110563325636));
#42881=CARTESIAN_POINT('Ctrl Pts',(26.25,6.33688598652166,-5.77461850881057));
#42882=CARTESIAN_POINT('Ctrl Pts',(26.5,5.25043192007604,-5.1048615648549));
#42883=CARTESIAN_POINT('Ctrl Pts',(26.25,5.25043192007604,-5.1048615648549));
#42884=CARTESIAN_POINT('Ctrl Pts',(26.5,5.58956861256095,-5.10820728774859));
#42885=CARTESIAN_POINT('Ctrl Pts',(26.25,5.58956861256095,-5.10820728774859));
#42886=CARTESIAN_POINT('Ctrl Pts',(26.5,5.87517352152691,-5.29465658348726));
#42887=CARTESIAN_POINT('Ctrl Pts',(26.25,5.87517352152691,-5.29465658348726));
#42888=CARTESIAN_POINT('Ctrl Pts',(26.5,5.25043192007604,-5.1048615648549));
#42889=CARTESIAN_POINT('Ctrl Pts',(26.5,5.58956861256095,-5.10820728774859));
#42890=CARTESIAN_POINT('Ctrl Pts',(26.5,5.87517352152691,-5.29465658348726));
#42891=CARTESIAN_POINT('Ctrl Pts',(26.25,5.25043192007604,-5.1048615648549));
#42892=CARTESIAN_POINT('Ctrl Pts',(26.25,5.58956861256095,-5.10820728774859));
#42893=CARTESIAN_POINT('Ctrl Pts',(26.25,5.87517352152691,-5.29465658348726));
#42894=CARTESIAN_POINT('Origin',(26.25,5.3196280859714,-6.44376715403288));
#42895=CARTESIAN_POINT('Origin',(26.5,1.72219374887709,-7.06668375067375));
#42896=CARTESIAN_POINT('',(26.5,1.72219374887709,-7.06668375067375));
#42897=CARTESIAN_POINT('',(26.5,3.94437549748797,-8.11603042842518));
#42898=CARTESIAN_POINT('',(26.5,-0.346179236230716,-6.0899678175011));
#42899=CARTESIAN_POINT('',(26.25,1.72219374887709,-7.06668375067375));
#42900=CARTESIAN_POINT('',(26.5,1.72219374887709,-7.06668375067375));
#42901=CARTESIAN_POINT('',(26.25,3.94437549748797,-8.11603042842518));
#42902=CARTESIAN_POINT('',(26.25,1.72219374887709,-7.06668375067375));
#42903=CARTESIAN_POINT('',(26.5,3.94437549748797,-8.11603042842518));
#42904=CARTESIAN_POINT('Origin',(26.5,1.41955597704928,-7.24826641377043));
#42905=CARTESIAN_POINT('',(26.5,1.41955597704928,-7.24826641377043));
#42906=CARTESIAN_POINT('',(26.5,2.496542694407,-6.6020743833558));
#42907=CARTESIAN_POINT('',(26.25,1.41955597704928,-7.24826641377043));
#42908=CARTESIAN_POINT('',(26.5,1.41955597704928,-7.24826641377043));
#42909=CARTESIAN_POINT('',(26.25,1.41955597704928,-7.24826641377043));
#42910=CARTESIAN_POINT('Origin',(26.5,2.75724489209471,-9.47774793884615));
#42911=CARTESIAN_POINT('',(26.5,2.75724489209471,-9.47774793884615));
#42912=CARTESIAN_POINT('',(26.5,0.301635728689645,-5.3850659998377));
#42913=CARTESIAN_POINT('',(26.25,2.75724489209471,-9.47774793884615));
#42914=CARTESIAN_POINT('',(26.5,2.75724489209471,-9.47774793884615));
#42915=CARTESIAN_POINT('',(26.25,2.75724489209471,-9.47774793884615));
#42916=CARTESIAN_POINT('Origin',(26.5,3.04011233217859,-9.30802747479582));
#42917=CARTESIAN_POINT('',(26.5,3.04011233217859,-9.30802747479582));
#42918=CARTESIAN_POINT('',(26.5,3.97566532949436,-8.74669567640636));
#42919=CARTESIAN_POINT('',(26.25,3.04011233217859,-9.30802747479582));
#42920=CARTESIAN_POINT('',(26.5,3.04011233217859,-9.30802747479582));
#42921=CARTESIAN_POINT('',(26.25,3.04011233217859,-9.30802747479582));
#42922=CARTESIAN_POINT('Origin',(26.5,1.9898531647998,-7.5575955291645));
#42923=CARTESIAN_POINT('',(26.5,1.9898531647998,-7.5575955291645));
#42924=CARTESIAN_POINT('',(26.5,0.05937358508413,-4.34012956297171));
#42925=CARTESIAN_POINT('',(26.25,1.9898531647998,-7.5575955291645));
#42926=CARTESIAN_POINT('',(26.5,1.9898531647998,-7.5575955291645));
#42927=CARTESIAN_POINT('',(26.25,1.9898531647998,-7.5575955291645));
#42928=CARTESIAN_POINT('Origin',(26.5,4.21112243656096,-8.6054214121664));
#42929=CARTESIAN_POINT('',(26.5,4.21112243656096,-8.6054214121664));
#42930=CARTESIAN_POINT('',(26.5,0.828567464789562,-7.00978926834771));
#42931=CARTESIAN_POINT('',(26.25,4.21112243656096,-8.6054214121664));
#42932=CARTESIAN_POINT('',(26.5,4.21112243656096,-8.6054214121664));
#42933=CARTESIAN_POINT('',(26.25,4.21112243656096,-8.6054214121664));
#42934=CARTESIAN_POINT('Origin',(26.5,4.51376012852852,-8.42383879698586));
#42935=CARTESIAN_POINT('',(26.5,4.51376012852852,-8.42383879698586));
#42936=CARTESIAN_POINT('',(26.5,4.71248922766934,-8.30460133750137));
#42937=CARTESIAN_POINT('',(26.25,4.51376012852852,-8.42383879698586));
#42938=CARTESIAN_POINT('',(26.5,4.51376012852852,-8.42383879698586));
#42939=CARTESIAN_POINT('',(26.25,4.51376012852852,-8.42383879698586));
#42940=CARTESIAN_POINT('Origin',(26.5,3.17607121348309,-6.19435727191015));
#42941=CARTESIAN_POINT('',(26.5,3.17607121348309,-6.19435727191015));
#42942=CARTESIAN_POINT('',(26.5,1.38930650760073,-3.21641609543956));
#42943=CARTESIAN_POINT('',(26.25,3.17607121348309,-6.19435727191015));
#42944=CARTESIAN_POINT('',(26.5,3.17607121348309,-6.19435727191015));
#42945=CARTESIAN_POINT('',(26.25,3.17607121348309,-6.19435727191015));
#42946=CARTESIAN_POINT('Origin',(26.5,2.89320385325946,-6.36407768804433));
#42947=CARTESIAN_POINT('',(26.5,2.89320385325946,-6.36407768804433));
#42948=CARTESIAN_POINT('',(26.5,3.23336663251209,-6.15998002049275));
#42949=CARTESIAN_POINT('',(26.25,2.89320385325946,-6.36407768804433));
#42950=CARTESIAN_POINT('',(26.5,2.89320385325946,-6.36407768804433));
#42951=CARTESIAN_POINT('',(26.25,2.89320385325946,-6.36407768804433));
#42952=CARTESIAN_POINT('Origin',(26.5,3.94437549748797,-8.11603042842518));
#42953=CARTESIAN_POINT('',(26.5,1.63202496949136,-4.26211288176416));
#42954=CARTESIAN_POINT('',(26.25,3.94437549748797,-8.11603042842518));
#42955=CARTESIAN_POINT('Origin',(26.25,2.9666580527889,-7.83605260537815));
#42956=CARTESIAN_POINT('Ctrl Pts',(26.5,0.501266317583819,6.69979499726322));
#42957=CARTESIAN_POINT('Ctrl Pts',(26.25,0.501266317583819,6.69979499726322));
#42958=CARTESIAN_POINT('Ctrl Pts',(26.5,0.172902956413169,6.86397667784855));
#42959=CARTESIAN_POINT('Ctrl Pts',(26.25,0.172902956413169,6.86397667784855));
#42960=CARTESIAN_POINT('Ctrl Pts',(26.5,-0.00634856473139531,7.15188948100021));
#42961=CARTESIAN_POINT('Ctrl Pts',(26.25,-0.00634856473139531,7.15188948100021));
#42962=CARTESIAN_POINT('',(26.5,0.501266317583819,6.69979499726322));
#42963=CARTESIAN_POINT('',(26.5,-0.00634856473139531,7.15188948100021));
#42964=CARTESIAN_POINT('Ctrl Pts',(26.5,0.501266317583819,6.69979499726322));
#42965=CARTESIAN_POINT('Ctrl Pts',(26.5,0.172902956413169,6.86397667784855));
#42966=CARTESIAN_POINT('Ctrl Pts',(26.5,-0.00634856473139531,7.15188948100021));
#42967=CARTESIAN_POINT('',(26.25,0.501266317583819,6.69979499726322));
#42968=CARTESIAN_POINT('',(26.5,0.501266317583819,6.69979499726322));
#42969=CARTESIAN_POINT('',(26.25,-0.00634856473139531,7.15188948100021));
#42970=CARTESIAN_POINT('Ctrl Pts',(26.25,0.501266317583819,6.69979499726322));
#42971=CARTESIAN_POINT('Ctrl Pts',(26.25,0.172902956413169,6.86397667784855));
#42972=CARTESIAN_POINT('Ctrl Pts',(26.25,-0.00634856473139531,7.15188948100021));
#42973=CARTESIAN_POINT('',(26.5,-0.00634856473139531,7.15188948100021));
#42974=CARTESIAN_POINT('Ctrl Pts',(26.5,1.13776779423563,6.56099416741769));
#42975=CARTESIAN_POINT('Ctrl Pts',(26.25,1.13776779423563,6.56099416741769));
#42976=CARTESIAN_POINT('Ctrl Pts',(26.5,0.804248894654697,6.54830370872778));
#42977=CARTESIAN_POINT('Ctrl Pts',(26.25,0.804248894654697,6.54830370872778));
#42978=CARTESIAN_POINT('Ctrl Pts',(26.5,0.501266317583819,6.69979499726322));
#42979=CARTESIAN_POINT('Ctrl Pts',(26.25,0.501266317583819,6.69979499726322));
#42980=CARTESIAN_POINT('',(26.5,1.13776779423563,6.56099416741769));
#42981=CARTESIAN_POINT('Ctrl Pts',(26.5,1.13776779423563,6.56099416741769));
#42982=CARTESIAN_POINT('Ctrl Pts',(26.5,0.804248894654697,6.54830370872778));
#42983=CARTESIAN_POINT('Ctrl Pts',(26.5,0.501266317583819,6.69979499726322));
#42984=CARTESIAN_POINT('',(26.25,1.13776779423563,6.56099416741769));
#42985=CARTESIAN_POINT('',(26.5,1.13776779423563,6.56099416741769));
#42986=CARTESIAN_POINT('Ctrl Pts',(26.25,1.13776779423563,6.56099416741769));
#42987=CARTESIAN_POINT('Ctrl Pts',(26.25,0.804248894654697,6.54830370872778));
#42988=CARTESIAN_POINT('Ctrl Pts',(26.25,0.501266317583819,6.69979499726322));
#42989=CARTESIAN_POINT('Ctrl Pts',(26.5,1.75364751708642,6.78148932944435));
#42990=CARTESIAN_POINT('Ctrl Pts',(26.25,1.75364751708642,6.78148932944435));
#42991=CARTESIAN_POINT('Ctrl Pts',(26.5,1.47128669381657,6.57368462610759));
#42992=CARTESIAN_POINT('Ctrl Pts',(26.25,1.47128669381657,6.57368462610759));
#42993=CARTESIAN_POINT('Ctrl Pts',(26.5,1.13776779423563,6.56099416741769));
#42994=CARTESIAN_POINT('Ctrl Pts',(26.25,1.13776779423563,6.56099416741769));
#42995=CARTESIAN_POINT('',(26.5,1.75364751708642,6.78148932944435));
#42996=CARTESIAN_POINT('Ctrl Pts',(26.5,1.75364751708642,6.78148932944435));
#42997=CARTESIAN_POINT('Ctrl Pts',(26.5,1.47128669381657,6.57368462610759));
#42998=CARTESIAN_POINT('Ctrl Pts',(26.5,1.13776779423563,6.56099416741769));
#42999=CARTESIAN_POINT('',(26.25,1.75364751708642,6.78148932944435));
#43000=CARTESIAN_POINT('',(26.5,1.75364751708642,6.78148932944435));
#43001=CARTESIAN_POINT('Ctrl Pts',(26.25,1.75364751708642,6.78148932944435));
#43002=CARTESIAN_POINT('Ctrl Pts',(26.25,1.47128669381657,6.57368462610759));
#43003=CARTESIAN_POINT('Ctrl Pts',(26.25,1.13776779423563,6.56099416741769));
#43004=CARTESIAN_POINT('Ctrl Pts',(26.5,2.21288027971144,7.34303824469154));
#43005=CARTESIAN_POINT('Ctrl Pts',(26.25,2.21288027971144,7.34303824469154));
#43006=CARTESIAN_POINT('Ctrl Pts',(26.5,2.03600820707623,6.98929409942112));
#43007=CARTESIAN_POINT('Ctrl Pts',(26.25,2.03600820707623,6.98929409942112));
#43008=CARTESIAN_POINT('Ctrl Pts',(26.5,1.75364751708642,6.78148932944435));
#43009=CARTESIAN_POINT('Ctrl Pts',(26.25,1.75364751708642,6.78148932944435));
#43010=CARTESIAN_POINT('',(26.5,2.21288027971144,7.34303824469154));
#43011=CARTESIAN_POINT('Ctrl Pts',(26.5,2.21288027971144,7.34303824469154));
#43012=CARTESIAN_POINT('Ctrl Pts',(26.5,2.03600820707623,6.98929409942112));
#43013=CARTESIAN_POINT('Ctrl Pts',(26.5,1.75364751708642,6.78148932944435));
#43014=CARTESIAN_POINT('',(26.25,2.21288027971144,7.34303824469154));
#43015=CARTESIAN_POINT('',(26.5,2.21288027971144,7.34303824469154));
#43016=CARTESIAN_POINT('Ctrl Pts',(26.25,2.21288027971144,7.34303824469154));
#43017=CARTESIAN_POINT('Ctrl Pts',(26.25,2.03600820707623,6.98929409942112));
#43018=CARTESIAN_POINT('Ctrl Pts',(26.25,1.75364751708642,6.78148932944435));
#43019=CARTESIAN_POINT('Ctrl Pts',(26.5,2.38935597751515,8.03506005328157));
#43020=CARTESIAN_POINT('Ctrl Pts',(26.25,2.38935597751515,8.03506005328157));
#43021=CARTESIAN_POINT('Ctrl Pts',(26.5,2.3873729038373,7.69202349294325));
#43022=CARTESIAN_POINT('Ctrl Pts',(26.25,2.3873729038373,7.69202349294325));
#43023=CARTESIAN_POINT('Ctrl Pts',(26.5,2.21288027971144,7.34303824469154));
#43024=CARTESIAN_POINT('Ctrl Pts',(26.25,2.21288027971144,7.34303824469154));
#43025=CARTESIAN_POINT('',(26.5,2.38935597751515,8.03506005328157));
#43026=CARTESIAN_POINT('Ctrl Pts',(26.5,2.38935597751515,8.03506005328157));
#43027=CARTESIAN_POINT('Ctrl Pts',(26.5,2.3873729038373,7.69202349294325));
#43028=CARTESIAN_POINT('Ctrl Pts',(26.5,2.21288027971144,7.34303824469154));
#43029=CARTESIAN_POINT('',(26.25,2.38935597751515,8.03506005328157));
#43030=CARTESIAN_POINT('',(26.5,2.38935597751515,8.03506005328157));
#43031=CARTESIAN_POINT('Ctrl Pts',(26.25,2.38935597751515,8.03506005328157));
#43032=CARTESIAN_POINT('Ctrl Pts',(26.25,2.3873729038373,7.69202349294325));
#43033=CARTESIAN_POINT('Ctrl Pts',(26.25,2.21288027971144,7.34303824469154));
#43034=CARTESIAN_POINT('Ctrl Pts',(26.5,2.20970768169897,8.66125071967288));
#43035=CARTESIAN_POINT('Ctrl Pts',(26.25,2.20970768169897,8.66125071967288));
#43036=CARTESIAN_POINT('Ctrl Pts',(26.5,2.39133858471287,8.3780966802599));
#43037=CARTESIAN_POINT('Ctrl Pts',(26.25,2.39133858471287,8.3780966802599));
#43038=CARTESIAN_POINT('Ctrl Pts',(26.5,2.38935597751515,8.03506005328157));
#43039=CARTESIAN_POINT('Ctrl Pts',(26.25,2.38935597751515,8.03506005328157));
#43040=CARTESIAN_POINT('',(26.5,2.20970768169897,8.66125071967288));
#43041=CARTESIAN_POINT('Ctrl Pts',(26.5,2.20970768169897,8.66125071967288));
#43042=CARTESIAN_POINT('Ctrl Pts',(26.5,2.39133858471287,8.3780966802599));
#43043=CARTESIAN_POINT('Ctrl Pts',(26.5,2.38935597751515,8.03506005328157));
#43044=CARTESIAN_POINT('',(26.25,2.20970768169897,8.66125071967288));
#43045=CARTESIAN_POINT('',(26.5,2.20970768169897,8.66125071967288));
#43046=CARTESIAN_POINT('Ctrl Pts',(26.25,2.20970768169897,8.66125071967288));
#43047=CARTESIAN_POINT('Ctrl Pts',(26.25,2.39133858471287,8.3780966802599));
#43048=CARTESIAN_POINT('Ctrl Pts',(26.25,2.38935597751515,8.03506005328157));
#43049=CARTESIAN_POINT('Ctrl Pts',(26.5,1.70605854689935,9.10541370837869));
#43050=CARTESIAN_POINT('Ctrl Pts',(26.25,1.70605854689935,9.10541370837869));
#43051=CARTESIAN_POINT('Ctrl Pts',(26.5,2.02807671204505,8.94440462580583));
#43052=CARTESIAN_POINT('Ctrl Pts',(26.25,2.02807671204505,8.94440462580583));
#43053=CARTESIAN_POINT('Ctrl Pts',(26.5,2.20970768169897,8.66125071967288));
#43054=CARTESIAN_POINT('Ctrl Pts',(26.25,2.20970768169897,8.66125071967288));
#43055=CARTESIAN_POINT('',(26.5,1.70605854689935,9.10541370837869));
#43056=CARTESIAN_POINT('Ctrl Pts',(26.5,1.70605854689935,9.10541370837869));
#43057=CARTESIAN_POINT('Ctrl Pts',(26.5,2.02807671204505,8.94440462580583));
#43058=CARTESIAN_POINT('Ctrl Pts',(26.5,2.20970768169897,8.66125071967288));
#43059=CARTESIAN_POINT('',(26.25,1.70605854689935,9.10541370837869));
#43060=CARTESIAN_POINT('',(26.5,1.70605854689935,9.10541370837869));
#43061=CARTESIAN_POINT('Ctrl Pts',(26.25,1.70605854689935,9.10541370837869));
#43062=CARTESIAN_POINT('Ctrl Pts',(26.25,2.02807671204505,8.94440462580583));
#43063=CARTESIAN_POINT('Ctrl Pts',(26.25,2.20970768169897,8.66125071967288));
#43064=CARTESIAN_POINT('Ctrl Pts',(26.5,0.739607410070647,9.17917651220862));
#43065=CARTESIAN_POINT('Ctrl Pts',(26.25,0.739607410070647,9.17917651220862));
#43066=CARTESIAN_POINT('Ctrl Pts',(26.5,1.21430658800647,9.35128968782512));
#43067=CARTESIAN_POINT('Ctrl Pts',(26.25,1.21430658800647,9.35128968782512));
#43068=CARTESIAN_POINT('Ctrl Pts',(26.5,1.70605854689935,9.10541370837869));
#43069=CARTESIAN_POINT('Ctrl Pts',(26.25,1.70605854689935,9.10541370837869));
#43070=CARTESIAN_POINT('',(26.5,0.739607410070647,9.17917651220862));
#43071=CARTESIAN_POINT('Ctrl Pts',(26.5,0.739607410070647,9.17917651220862));
#43072=CARTESIAN_POINT('Ctrl Pts',(26.5,1.21430658800647,9.35128968782512));
#43073=CARTESIAN_POINT('Ctrl Pts',(26.5,1.70605854689935,9.10541370837869));
#43074=CARTESIAN_POINT('',(26.25,0.739607410070647,9.17917651220862));
#43075=CARTESIAN_POINT('',(26.5,0.739607410070647,9.17917651220862));
#43076=CARTESIAN_POINT('Ctrl Pts',(26.25,0.739607410070647,9.17917651220862));
#43077=CARTESIAN_POINT('Ctrl Pts',(26.25,1.21430658800647,9.35128968782512));
#43078=CARTESIAN_POINT('Ctrl Pts',(26.25,1.70605854689935,9.10541370837869));
#43079=CARTESIAN_POINT('Ctrl Pts',(26.5,-0.0245909866431014,8.4280650239863));
#43080=CARTESIAN_POINT('Ctrl Pts',(26.25,-0.0245909866431014,8.4280650239863));
#43081=CARTESIAN_POINT('Ctrl Pts',(26.5,0.26490818215481,9.00706336158212));
#43082=CARTESIAN_POINT('Ctrl Pts',(26.25,0.26490818215481,9.00706336158212));
#43083=CARTESIAN_POINT('Ctrl Pts',(26.5,0.739607410070647,9.17917651220862));
#43084=CARTESIAN_POINT('Ctrl Pts',(26.25,0.739607410070647,9.17917651220862));
#43085=CARTESIAN_POINT('',(26.5,-0.0245909866431014,8.4280650239863));
#43086=CARTESIAN_POINT('Ctrl Pts',(26.5,-0.0245909866431014,8.4280650239863));
#43087=CARTESIAN_POINT('Ctrl Pts',(26.5,0.26490818215481,9.00706336158212));
#43088=CARTESIAN_POINT('Ctrl Pts',(26.5,0.739607410070647,9.17917651220862));
#43089=CARTESIAN_POINT('',(26.25,-0.0245909866431014,8.4280650239863));
#43090=CARTESIAN_POINT('',(26.5,-0.0245909866431014,8.4280650239863));
#43091=CARTESIAN_POINT('Ctrl Pts',(26.25,-0.0245909866431014,8.4280650239863));
#43092=CARTESIAN_POINT('Ctrl Pts',(26.25,0.26490818215481,9.00706336158212));
#43093=CARTESIAN_POINT('Ctrl Pts',(26.25,0.739607410070647,9.17917651220862));
#43094=CARTESIAN_POINT('Ctrl Pts',(26.5,-0.181634271720352,7.78085620397245));
#43095=CARTESIAN_POINT('Ctrl Pts',(26.25,-0.181634271720352,7.78085620397245));
#43096=CARTESIAN_POINT('Ctrl Pts',(26.5,-0.177668574184776,8.12190984890295));
#43097=CARTESIAN_POINT('Ctrl Pts',(26.25,-0.177668574184776,8.12190984890295));
#43098=CARTESIAN_POINT('Ctrl Pts',(26.5,-0.0245909866431014,8.4280650239863));
#43099=CARTESIAN_POINT('Ctrl Pts',(26.25,-0.0245909866431014,8.4280650239863));
#43100=CARTESIAN_POINT('',(26.5,-0.181634271720352,7.78085620397245));
#43101=CARTESIAN_POINT('Ctrl Pts',(26.5,-0.181634271720352,7.78085620397245));
#43102=CARTESIAN_POINT('Ctrl Pts',(26.5,-0.177668574184776,8.12190984890295));
#43103=CARTESIAN_POINT('Ctrl Pts',(26.5,-0.0245909866431014,8.4280650239863));
#43104=CARTESIAN_POINT('',(26.25,-0.181634271720352,7.78085620397245));
#43105=CARTESIAN_POINT('',(26.5,-0.181634271720352,7.78085620397245));
#43106=CARTESIAN_POINT('Ctrl Pts',(26.25,-0.181634271720352,7.78085620397245));
#43107=CARTESIAN_POINT('Ctrl Pts',(26.25,-0.177668574184776,8.12190984890295));
#43108=CARTESIAN_POINT('Ctrl Pts',(26.25,-0.0245909866431014,8.4280650239863));
#43109=CARTESIAN_POINT('Ctrl Pts',(26.5,-0.00634856473139531,7.15188948100021));
#43110=CARTESIAN_POINT('Ctrl Pts',(26.25,-0.00634856473139531,7.15188948100021));
#43111=CARTESIAN_POINT('Ctrl Pts',(26.5,-0.18560008587596,7.43980228415186));
#43112=CARTESIAN_POINT('Ctrl Pts',(26.25,-0.18560008587596,7.43980228415186));
#43113=CARTESIAN_POINT('Ctrl Pts',(26.5,-0.181634271720352,7.78085620397245));
#43114=CARTESIAN_POINT('Ctrl Pts',(26.25,-0.181634271720352,7.78085620397245));
#43115=CARTESIAN_POINT('Ctrl Pts',(26.5,-0.00634856473139531,7.15188948100021));
#43116=CARTESIAN_POINT('Ctrl Pts',(26.5,-0.18560008587596,7.43980228415186));
#43117=CARTESIAN_POINT('Ctrl Pts',(26.5,-0.181634271720352,7.78085620397245));
#43118=CARTESIAN_POINT('Ctrl Pts',(26.25,-0.00634856473139531,7.15188948100021));
#43119=CARTESIAN_POINT('Ctrl Pts',(26.25,-0.18560008587596,7.43980228415186));
#43120=CARTESIAN_POINT('Ctrl Pts',(26.25,-0.181634271720352,7.78085620397245));
#43121=CARTESIAN_POINT('Origin',(26.25,1.10286924941845,7.94979669827645));
#43122=CARTESIAN_POINT('Origin',(26.5,3.97287629488924,6.33415360944603));
#43123=CARTESIAN_POINT('',(26.5,3.97287629488924,6.33415360944603));
#43124=CARTESIAN_POINT('',(26.5,2.88150424459951,6.8798396345909));
#43125=CARTESIAN_POINT('',(26.5,3.65055649882275,6.49531350747928));
#43126=CARTESIAN_POINT('',(26.25,3.97287629488924,6.33415360944603));
#43127=CARTESIAN_POINT('',(26.5,3.97287629488924,6.33415360944603));
#43128=CARTESIAN_POINT('',(26.25,2.88150424459951,6.8798396345909));
#43129=CARTESIAN_POINT('',(26.25,3.97287629488924,6.33415360944603));
#43130=CARTESIAN_POINT('',(26.5,2.88150424459951,6.8798396345909));
#43131=CARTESIAN_POINT('Origin',(26.5,4.11009095900857,6.60858293768471));
#43132=CARTESIAN_POINT('',(26.5,4.11009095900857,6.60858293768471));
#43133=CARTESIAN_POINT('',(26.5,2.37736527557078,3.14313157080911));
#43134=CARTESIAN_POINT('',(26.25,4.11009095900857,6.60858293768471));
#43135=CARTESIAN_POINT('',(26.5,4.11009095900857,6.60858293768471));
#43136=CARTESIAN_POINT('',(26.25,4.11009095900857,6.60858293768471));
#43137=CARTESIAN_POINT('Origin',(26.5,3.01871890871885,7.15426896282957));
#43138=CARTESIAN_POINT('',(26.5,3.01871890871885,7.15426896282957));
#43139=CARTESIAN_POINT('',(26.5,3.24208513779722,7.04258584829038));
#43140=CARTESIAN_POINT('',(26.25,3.01871890871885,7.15426896282957));
#43141=CARTESIAN_POINT('',(26.5,3.01871890871885,7.15426896282957));
#43142=CARTESIAN_POINT('',(26.25,3.01871890871885,7.15426896282957));
#43143=CARTESIAN_POINT('Origin',(26.5,3.37880818337419,7.87444751214026));
#43144=CARTESIAN_POINT('',(26.5,3.37880818337419,7.87444751214026));
#43145=CARTESIAN_POINT('',(26.5,1.46603786260872,4.04890687060932));
#43146=CARTESIAN_POINT('',(26.25,3.37880818337419,7.87444751214026));
#43147=CARTESIAN_POINT('',(26.5,3.37880818337419,7.87444751214026));
#43148=CARTESIAN_POINT('',(26.25,3.37880818337419,7.87444751214026));
#43149=CARTESIAN_POINT('Origin',(26.5,4.63991396077107,7.24389462344182));
#43150=CARTESIAN_POINT('',(26.5,4.63991396077107,7.24389462344182));
#43151=CARTESIAN_POINT('',(26.5,4.23272730115101,7.44748795325186));
#43152=CARTESIAN_POINT('',(26.25,4.63991396077107,7.24389462344182));
#43153=CARTESIAN_POINT('',(26.5,4.63991396077107,7.24389462344182));
#43154=CARTESIAN_POINT('',(26.25,4.63991396077107,7.24389462344182));
#43155=CARTESIAN_POINT('Origin',(26.5,4.7771286248904,7.5183239516805));
#43156=CARTESIAN_POINT('',(26.5,4.7771286248904,7.5183239516805));
#43157=CARTESIAN_POINT('',(26.5,2.79575097206527,3.55556864603021));
#43158=CARTESIAN_POINT('',(26.25,4.7771286248904,7.5183239516805));
#43159=CARTESIAN_POINT('',(26.5,4.7771286248904,7.5183239516805));
#43160=CARTESIAN_POINT('',(26.25,4.7771286248904,7.5183239516805));
#43161=CARTESIAN_POINT('Origin',(26.5,3.20828129010392,8.30274761907374));
#43162=CARTESIAN_POINT('',(26.5,3.20828129010392,8.30274761907374));
#43163=CARTESIAN_POINT('',(26.5,3.5855182978771,8.11412911518715));
#43164=CARTESIAN_POINT('',(26.25,3.20828129010392,8.30274761907374));
#43165=CARTESIAN_POINT('',(26.5,3.20828129010392,8.30274761907374));
#43166=CARTESIAN_POINT('',(26.25,3.20828129010392,8.30274761907374));
#43167=CARTESIAN_POINT('Origin',(26.5,2.04552598445364,5.97723700777318));
#43168=CARTESIAN_POINT('',(26.5,2.04552598445364,5.97723700777318));
#43169=CARTESIAN_POINT('',(26.5,0.64552598445364,3.17723700777318));
#43170=CARTESIAN_POINT('',(26.25,2.04552598445364,5.97723700777318));
#43171=CARTESIAN_POINT('',(26.5,2.04552598445364,5.97723700777318));
#43172=CARTESIAN_POINT('',(26.25,2.04552598445364,5.97723700777318));
#43173=CARTESIAN_POINT('Origin',(26.5,2.35326754184325,5.82336622907838));
#43174=CARTESIAN_POINT('',(26.5,2.35326754184325,5.82336622907838));
#43175=CARTESIAN_POINT('',(26.5,2.57663377092163,5.71168311453919));
#43176=CARTESIAN_POINT('',(26.25,2.35326754184325,5.82336622907838));
#43177=CARTESIAN_POINT('',(26.5,2.35326754184325,5.82336622907838));
#43178=CARTESIAN_POINT('',(26.25,2.35326754184325,5.82336622907838));
#43179=CARTESIAN_POINT('Origin',(26.5,2.88150424459951,6.8798396345909));
#43180=CARTESIAN_POINT('',(26.5,1.21738589322138,3.55160293183464));
#43181=CARTESIAN_POINT('',(26.25,2.88150424459951,6.8798396345909));
#43182=CARTESIAN_POINT('Origin',(26.25,3.41132730467202,7.06305692407606));
#43183=CARTESIAN_POINT('Origin',(26.5,5.95733328624929,5.34192511376601));
#43184=CARTESIAN_POINT('',(26.5,5.95733328624929,5.34192511376601));
#43185=CARTESIAN_POINT('',(26.5,4.86596123595957,5.88761113891087));
#43186=CARTESIAN_POINT('',(26.5,4.64278499450278,5.99919925963926));
#43187=CARTESIAN_POINT('',(26.25,5.95733328624929,5.34192511376601));
#43188=CARTESIAN_POINT('',(26.5,5.95733328624929,5.34192511376601));
#43189=CARTESIAN_POINT('',(26.25,4.86596123595957,5.88761113891087));
#43190=CARTESIAN_POINT('',(26.25,5.95733328624929,5.34192511376601));
#43191=CARTESIAN_POINT('',(26.5,4.86596123595957,5.88761113891087));
#43192=CARTESIAN_POINT('Origin',(26.5,6.09454795036863,5.61635444200468));
#43193=CARTESIAN_POINT('',(26.5,6.09454795036863,5.61635444200468));
#43194=CARTESIAN_POINT('',(26.5,4.36182226693084,2.15090307512908));
#43195=CARTESIAN_POINT('',(26.25,6.09454795036863,5.61635444200468));
#43196=CARTESIAN_POINT('',(26.5,6.09454795036863,5.61635444200468));
#43197=CARTESIAN_POINT('',(26.25,6.09454795036863,5.61635444200468));
#43198=CARTESIAN_POINT('Origin',(26.5,5.0031759000789,6.16204046714954));
#43199=CARTESIAN_POINT('',(26.5,5.0031759000789,6.16204046714954));
#43200=CARTESIAN_POINT('',(26.5,4.23431363347725,6.54647160045037));
#43201=CARTESIAN_POINT('',(26.25,5.0031759000789,6.16204046714954));
#43202=CARTESIAN_POINT('',(26.5,5.0031759000789,6.16204046714954));
#43203=CARTESIAN_POINT('',(26.25,5.0031759000789,6.16204046714954));
#43204=CARTESIAN_POINT('Origin',(26.5,5.36326517473425,6.88221901646023));
#43205=CARTESIAN_POINT('',(26.5,5.36326517473425,6.88221901646023));
#43206=CARTESIAN_POINT('',(26.5,3.45049485396878,3.05667837492929));
#43207=CARTESIAN_POINT('',(26.25,5.36326517473425,6.88221901646023));
#43208=CARTESIAN_POINT('',(26.5,5.36326517473425,6.88221901646023));
#43209=CARTESIAN_POINT('',(26.25,5.36326517473425,6.88221901646023));
#43210=CARTESIAN_POINT('Origin',(26.5,6.62437095213113,6.25166612776179));
#43211=CARTESIAN_POINT('',(26.5,6.62437095213113,6.25166612776179));
#43212=CARTESIAN_POINT('',(26.5,5.22495579683104,6.95137370541184));
#43213=CARTESIAN_POINT('',(26.25,6.62437095213113,6.25166612776179));
#43214=CARTESIAN_POINT('',(26.5,6.62437095213113,6.25166612776179));
#43215=CARTESIAN_POINT('',(26.25,6.62437095213113,6.25166612776179));
#43216=CARTESIAN_POINT('Origin',(26.5,6.76158561625046,6.52609545600047));
#43217=CARTESIAN_POINT('',(26.5,6.76158561625046,6.52609545600047));
#43218=CARTESIAN_POINT('',(26.5,4.78020796342532,2.56334015035019));
#43219=CARTESIAN_POINT('',(26.25,6.76158561625046,6.52609545600047));
#43220=CARTESIAN_POINT('',(26.5,6.76158561625046,6.52609545600047));
#43221=CARTESIAN_POINT('',(26.25,6.76158561625046,6.52609545600047));
#43222=CARTESIAN_POINT('Origin',(26.5,5.19273828146398,7.31051912339371));
#43223=CARTESIAN_POINT('',(26.5,5.19273828146398,7.31051912339371));
#43224=CARTESIAN_POINT('',(26.5,4.57774679355713,7.61801486734714));
#43225=CARTESIAN_POINT('',(26.25,5.19273828146398,7.31051912339371));
#43226=CARTESIAN_POINT('',(26.5,5.19273828146398,7.31051912339371));
#43227=CARTESIAN_POINT('',(26.25,5.19273828146398,7.31051912339371));
#43228=CARTESIAN_POINT('Origin',(26.5,4.0299829758137,4.98500851209315));
#43229=CARTESIAN_POINT('',(26.5,4.0299829758137,4.98500851209315));
#43230=CARTESIAN_POINT('',(26.5,2.6299829758137,2.18500851209315));
#43231=CARTESIAN_POINT('',(26.25,4.0299829758137,4.98500851209315));
#43232=CARTESIAN_POINT('',(26.5,4.0299829758137,4.98500851209315));
#43233=CARTESIAN_POINT('',(26.25,4.0299829758137,4.98500851209315));
#43234=CARTESIAN_POINT('Origin',(26.5,4.33772453320331,4.83113773339835));
#43235=CARTESIAN_POINT('',(26.5,4.33772453320331,4.83113773339835));
#43236=CARTESIAN_POINT('',(26.5,3.56886226660165,5.21556886669917));
#43237=CARTESIAN_POINT('',(26.25,4.33772453320331,4.83113773339835));
#43238=CARTESIAN_POINT('',(26.5,4.33772453320331,4.83113773339835));
#43239=CARTESIAN_POINT('',(26.25,4.33772453320331,4.83113773339835));
#43240=CARTESIAN_POINT('Origin',(26.5,4.86596123595957,5.88761113891087));
#43241=CARTESIAN_POINT('',(26.5,3.20184288458144,2.55937443615461));
#43242=CARTESIAN_POINT('',(26.25,4.86596123595957,5.88761113891087));
#43243=CARTESIAN_POINT('Origin',(26.25,5.39578429603208,6.07082842839603));
#43244=CARTESIAN_POINT('Origin',(26.2,3.6,0.));
#43245=CARTESIAN_POINT('',(26.2,-3.6,-4.40872847693047E-16));
#43246=CARTESIAN_POINT('Origin',(26.2,0.,0.));
#43247=CARTESIAN_POINT('',(26.2,-3.,-3.67394039744206E-16));
#43248=CARTESIAN_POINT('Origin',(26.2,0.,0.));
#43249=CARTESIAN_POINT('Origin',(26.4,0.,0.));
#43250=CARTESIAN_POINT('',(26.5,-3.6,4.40872847693047E-16));
#43251=CARTESIAN_POINT('',(26.4,-3.6,-4.40872847693047E-16));
#43252=CARTESIAN_POINT('Origin',(26.5,0.,0.));
#43253=CARTESIAN_POINT('Origin',(26.4,0.,0.));
#43254=CARTESIAN_POINT('',(26.5,-3.,-3.67394039744206E-16));
#43255=CARTESIAN_POINT('',(26.4,-3.,-3.67394039744206E-16));
#43256=CARTESIAN_POINT('Origin',(26.5,0.,0.));
#43257=CARTESIAN_POINT('Origin',(26.5,0.,0.));
#43258=CARTESIAN_POINT('Origin',(17.3,12.8479908659033,-2.32198852487824));
#43259=CARTESIAN_POINT('',(25.7,12.7818649395498,-2.37148237756648));
#43260=CARTESIAN_POINT('',(17.3,12.7818649395498,-2.37148237756648));
#43261=CARTESIAN_POINT('',(21.5,12.7818649395498,-2.37148237756648));
#43262=CARTESIAN_POINT('',(25.7,12.4224745293193,-2.64047847338555));
#43263=CARTESIAN_POINT('',(25.7,12.8479908659033,-2.32198852487824));
#43264=CARTESIAN_POINT('',(17.3,12.4224745293193,-2.64047847338555));
#43265=CARTESIAN_POINT('',(17.3,12.4224745293193,-2.64047847338555));
#43266=CARTESIAN_POINT('',(17.3,12.8479908659033,-2.32198852487824));
#43267=CARTESIAN_POINT('Origin',(17.3,12.5936503594477,-2.67686301927866));
#43268=CARTESIAN_POINT('',(17.3,12.6413834370917,-3.03239588385542));
#43269=CARTESIAN_POINT('Origin',(17.3,0.,0.));
#43270=CARTESIAN_POINT('',(17.3,12.4224745293193,-2.64047847338555));
#43271=CARTESIAN_POINT('Origin',(17.3,12.4224745293193,-2.64047847338555));
#43272=CARTESIAN_POINT('',(25.7,12.6413834370917,-3.03239588385542));
#43273=CARTESIAN_POINT('',(21.5,12.6413834370917,-3.03239588385542));
#43274=CARTESIAN_POINT('',(25.7,12.4224745293193,-2.64047847338555));
#43275=CARTESIAN_POINT('Origin',(25.7,12.5936503594477,-2.67686301927866));
#43276=CARTESIAN_POINT('Origin',(25.7,0.,0.));
#43277=CARTESIAN_POINT('Origin',(17.3,12.0844628794663,-4.94249500908216));
#43278=CARTESIAN_POINT('',(25.7,12.0094916126598,-4.97715894918518));
#43279=CARTESIAN_POINT('',(17.3,12.0094916126598,-4.97715894918518));
#43280=CARTESIAN_POINT('',(21.5,12.0094916126598,-4.97715894918518));
#43281=CARTESIAN_POINT('',(25.7,11.602027312061,-5.16555536706267));
#43282=CARTESIAN_POINT('',(25.7,12.0844628794663,-4.94249500908216));
#43283=CARTESIAN_POINT('',(17.3,11.602027312061,-5.16555536706267));
#43284=CARTESIAN_POINT('',(17.3,11.602027312061,-5.16555536706267));
#43285=CARTESIAN_POINT('',(17.3,12.0844628794663,-4.94249500908216));
#43286=CARTESIAN_POINT('Origin',(17.3,11.7618977671485,-5.23673427960094));
#43287=CARTESIAN_POINT('',(17.3,11.7346683235061,-5.59442216294961));
#43288=CARTESIAN_POINT('Origin',(17.3,0.,0.));
#43289=CARTESIAN_POINT('',(17.3,11.602027312061,-5.16555536706267));
#43290=CARTESIAN_POINT('Origin',(17.3,11.602027312061,-5.16555536706267));
#43291=CARTESIAN_POINT('',(25.7,11.7346683235061,-5.59442216294961));
#43292=CARTESIAN_POINT('',(21.5,11.7346683235061,-5.59442216294961));
#43293=CARTESIAN_POINT('',(25.7,11.602027312061,-5.16555536706267));
#43294=CARTESIAN_POINT('Origin',(25.7,11.7618977671485,-5.23673427960094));
#43295=CARTESIAN_POINT('Origin',(25.7,0.,0.));
#43296=CARTESIAN_POINT('Origin',(17.3,10.7927858775101,-7.3469907446668));
#43297=CARTESIAN_POINT('',(25.7,10.7122458743621,-7.36530979166607));
#43298=CARTESIAN_POINT('',(17.3,10.7122458743621,-7.36530979166607));
#43299=CARTESIAN_POINT('',(21.5,10.7122458743621,-7.36530979166607));
#43300=CARTESIAN_POINT('',(25.7,10.2745158285618,-7.46487270411441));
#43301=CARTESIAN_POINT('',(25.7,10.7927858775101,-7.3469907446668));
#43302=CARTESIAN_POINT('',(17.3,10.2745158285618,-7.46487270411441));
#43303=CARTESIAN_POINT('',(17.3,10.2745158285618,-7.46487270411441));
#43304=CARTESIAN_POINT('',(17.3,10.7927858775101,-7.3469907446668));
#43305=CARTESIAN_POINT('Origin',(17.3,10.4160938025774,-7.5677351232656));
#43306=CARTESIAN_POINT('',(17.3,10.3150918949973,-7.91194534850694));
#43307=CARTESIAN_POINT('Origin',(17.3,0.,0.));
#43308=CARTESIAN_POINT('',(17.3,10.2745158285618,-7.46487270411441));
#43309=CARTESIAN_POINT('Origin',(17.3,10.2745158285618,-7.46487270411441));
#43310=CARTESIAN_POINT('',(25.7,10.3150918949973,-7.91194534850694));
#43311=CARTESIAN_POINT('',(21.5,10.3150918949973,-7.91194534850694));
#43312=CARTESIAN_POINT('',(25.7,10.2745158285618,-7.46487270411441));
#43313=CARTESIAN_POINT('Origin',(25.7,10.4160938025774,-7.5677351232656));
#43314=CARTESIAN_POINT('Origin',(25.7,0.,0.));
#43315=CARTESIAN_POINT('Origin',(17.3,9.02941234317406,-9.43038772993646));
#43316=CARTESIAN_POINT('',(25.7,8.94682358829601,-9.43156125357357));
#43317=CARTESIAN_POINT('',(17.3,8.94682358829601,-9.43156125357357));
#43318=CARTESIAN_POINT('',(21.5,8.94682358829601,-9.43156125357357));
#43319=CARTESIAN_POINT('',(25.7,8.4979587007575,-9.43793928356291));
#43320=CARTESIAN_POINT('',(25.7,9.02941234317406,-9.43038772993646));
#43321=CARTESIAN_POINT('',(17.3,8.4979587007575,-9.43793928356291));
#43322=CARTESIAN_POINT('',(17.3,8.4979587007575,-9.43793928356291));
#43323=CARTESIAN_POINT('',(17.3,9.02941234317406,-9.43038772993646));
#43324=CARTESIAN_POINT('Origin',(17.3,8.6150565568703,-9.56798962802146));
#43325=CARTESIAN_POINT('',(17.3,8.44469645337457,-9.88367855660852));
#43326=CARTESIAN_POINT('Origin',(17.3,0.,0.));
#43327=CARTESIAN_POINT('',(17.3,8.4979587007575,-9.43793928356291));
#43328=CARTESIAN_POINT('Origin',(17.3,8.4979587007575,-9.43793928356291));
#43329=CARTESIAN_POINT('',(25.7,8.44469645337457,-9.88367855660852));
#43330=CARTESIAN_POINT('',(21.5,8.44469645337457,-9.88367855660852));
#43331=CARTESIAN_POINT('',(25.7,8.4979587007575,-9.43793928356291));
#43332=CARTESIAN_POINT('Origin',(25.7,8.6150565568703,-9.56798962802146));
#43333=CARTESIAN_POINT('Origin',(25.7,0.,0.));
#43334=CARTESIAN_POINT('Origin',(17.3,6.87141016151377,-11.1016315193869));
#43335=CARTESIAN_POINT('',(25.7,6.79038217979861,-11.0856082310477));
#43336=CARTESIAN_POINT('',(17.3,6.79038217979861,-11.0856082310477));
#43337=CARTESIAN_POINT('',(21.5,6.79038217979861,-11.0856082310477));
#43338=CARTESIAN_POINT('',(25.7,6.34999999999999,-10.9985226280624));
#43339=CARTESIAN_POINT('',(25.7,6.87141016151377,-11.1016315193869));
#43340=CARTESIAN_POINT('',(17.3,6.34999999999999,-10.9985226280624));
#43341=CARTESIAN_POINT('',(17.3,6.34999999999999,-10.9985226280624));
#43342=CARTESIAN_POINT('',(17.3,6.87141016151377,-11.1016315193869));
#43343=CARTESIAN_POINT('Origin',(17.3,6.43749999999999,-11.1500770737247));
#43344=CARTESIAN_POINT('',(17.3,6.2052272545899,-11.4234475846346));
#43345=CARTESIAN_POINT('Origin',(17.3,0.,0.));
#43346=CARTESIAN_POINT('',(17.3,6.34999999999999,-10.9985226280624));
#43347=CARTESIAN_POINT('Origin',(17.3,6.34999999999999,-10.9985226280624));
#43348=CARTESIAN_POINT('',(25.7,6.2052272545899,-11.4234475846346));
#43349=CARTESIAN_POINT('',(21.5,6.2052272545899,-11.4234475846346));
#43350=CARTESIAN_POINT('',(25.7,6.34999999999999,-10.9985226280624));
#43351=CARTESIAN_POINT('Origin',(25.7,6.43749999999999,-11.1500770737247));
#43352=CARTESIAN_POINT('Origin',(25.7,0.,0.));
#43353=CARTESIAN_POINT('Origin',(17.3,4.41309438311112,-12.2876807399018));
#43354=CARTESIAN_POINT('',(25.7,4.3371684861752,-12.255160934175));
#43355=CARTESIAN_POINT('',(17.3,4.3371684861752,-12.255160934175));
#43356=CARTESIAN_POINT('',(21.5,4.3371684861752,-12.255160934175));
#43357=CARTESIAN_POINT('',(25.7,3.92451582856183,-12.0784177569485));
#43358=CARTESIAN_POINT('',(25.7,4.41309438311112,-12.2876807399018));
#43359=CARTESIAN_POINT('',(17.3,3.92451582856183,-12.0784177569485));
#43360=CARTESIAN_POINT('',(17.3,3.92451582856183,-12.0784177569485));
#43361=CARTESIAN_POINT('',(17.3,4.41309438311112,-12.2876807399018));
#43362=CARTESIAN_POINT('Origin',(17.3,3.97859380257745,-12.2448526473001));
#43363=CARTESIAN_POINT('',(17.3,3.6945598487957,-12.463957137429));
#43364=CARTESIAN_POINT('Origin',(17.3,0.,0.));
#43365=CARTESIAN_POINT('',(17.3,3.92451582856183,-12.0784177569485));
#43366=CARTESIAN_POINT('Origin',(17.3,3.92451582856183,-12.0784177569485));
#43367=CARTESIAN_POINT('',(25.7,3.6945598487957,-12.463957137429));
#43368=CARTESIAN_POINT('',(21.5,3.6945598487957,-12.463957137429));
#43369=CARTESIAN_POINT('',(25.7,3.92451582856183,-12.0784177569485));
#43370=CARTESIAN_POINT('Origin',(25.7,3.97859380257745,-12.2448526473001));
#43371=CARTESIAN_POINT('Origin',(25.7,0.,0.));
#43372=CARTESIAN_POINT('Origin',(17.3,1.76190520379018,-12.9366993492489));
#43373=CARTESIAN_POINT('',(25.7,1.69439971766246,-12.8891042976921));
#43374=CARTESIAN_POINT('',(17.3,1.69439971766246,-12.8891042976921));
#43375=CARTESIAN_POINT('',(21.5,1.69439971766246,-12.8891042976921));
#43376=CARTESIAN_POINT('',(25.7,1.32751148349919,-12.6304280711771));
#43377=CARTESIAN_POINT('',(25.7,1.76190520379018,-12.9366993492489));
#43378=CARTESIAN_POINT('',(17.3,1.32751148349919,-12.6304280711771));
#43379=CARTESIAN_POINT('',(17.3,1.32751148349919,-12.6304280711771));
#43380=CARTESIAN_POINT('',(17.3,1.76190520379018,-12.9366993492489));
#43381=CARTESIAN_POINT('Origin',(17.3,1.34580396457103,-12.8044694028665));
#43382=CARTESIAN_POINT('',(17.3,1.02242244914403,-12.9597319546157));
#43383=CARTESIAN_POINT('Origin',(17.3,0.,0.));
#43384=CARTESIAN_POINT('',(17.3,1.32751148349919,-12.6304280711771));
#43385=CARTESIAN_POINT('Origin',(17.3,1.32751148349919,-12.6304280711771));
#43386=CARTESIAN_POINT('',(25.7,1.02242244914403,-12.9597319546157));
#43387=CARTESIAN_POINT('',(21.5,1.02242244914403,-12.9597319546157));
#43388=CARTESIAN_POINT('',(25.7,1.32751148349919,-12.6304280711771));
#43389=CARTESIAN_POINT('Origin',(25.7,1.34580396457103,-12.8044694028665));
#43390=CARTESIAN_POINT('Origin',(25.7,0.,0.));
#43391=CARTESIAN_POINT('Origin',(17.3,-0.966287687495578,-13.020322119863));
#43392=CARTESIAN_POINT('',(25.7,-1.02242244914404,-12.9597319546157));
#43393=CARTESIAN_POINT('',(17.3,-1.02242244914404,-12.9597319546157));
#43394=CARTESIAN_POINT('',(21.5,-1.02242244914404,-12.9597319546157));
#43395=CARTESIAN_POINT('',(25.7,-1.32751148349921,-12.6304280711771));
#43396=CARTESIAN_POINT('',(25.7,-0.966287687495578,-13.020322119863));
#43397=CARTESIAN_POINT('',(17.3,-1.32751148349921,-12.6304280711771));
#43398=CARTESIAN_POINT('',(17.3,-1.32751148349921,-12.6304280711771));
#43399=CARTESIAN_POINT('',(17.3,-0.966287687495578,-13.020322119863));
#43400=CARTESIAN_POINT('Origin',(17.3,-1.34580396457105,-12.8044694028665));
#43401=CARTESIAN_POINT('',(17.3,-1.69439971766248,-12.8891042976921));
#43402=CARTESIAN_POINT('Origin',(17.3,0.,0.));
#43403=CARTESIAN_POINT('',(17.3,-1.32751148349921,-12.6304280711771));
#43404=CARTESIAN_POINT('Origin',(17.3,-1.32751148349921,-12.6304280711771));
#43405=CARTESIAN_POINT('',(25.7,-1.69439971766248,-12.8891042976921));
#43406=CARTESIAN_POINT('',(21.5,-1.69439971766248,-12.8891042976921));
#43407=CARTESIAN_POINT('',(25.7,-1.32751148349921,-12.6304280711771));
#43408=CARTESIAN_POINT('Origin',(25.7,-1.34580396457105,-12.8044694028665));
#43409=CARTESIAN_POINT('Origin',(25.7,0.,0.));
#43410=CARTESIAN_POINT('Origin',(17.3,-3.65224917007501,-12.5348943354017));
#43411=CARTESIAN_POINT('',(25.7,-3.69455984879571,-12.463957137429));
#43412=CARTESIAN_POINT('',(17.3,-3.69455984879571,-12.463957137429));
#43413=CARTESIAN_POINT('',(21.5,-3.69455984879571,-12.463957137429));
#43414=CARTESIAN_POINT('',(25.7,-3.92451582856183,-12.0784177569485));
#43415=CARTESIAN_POINT('',(25.7,-3.65224917007501,-12.5348943354017));
#43416=CARTESIAN_POINT('',(17.3,-3.92451582856183,-12.0784177569485));
#43417=CARTESIAN_POINT('',(17.3,-3.92451582856183,-12.0784177569485));
#43418=CARTESIAN_POINT('',(17.3,-3.65224917007501,-12.5348943354017));
#43419=CARTESIAN_POINT('Origin',(17.3,-3.97859380257745,-12.2448526473001));
#43420=CARTESIAN_POINT('',(17.3,-4.3371684861752,-12.255160934175));
#43421=CARTESIAN_POINT('Origin',(17.3,0.,0.));
#43422=CARTESIAN_POINT('',(17.3,-3.92451582856183,-12.0784177569485));
#43423=CARTESIAN_POINT('Origin',(17.3,-3.92451582856183,-12.0784177569485));
#43424=CARTESIAN_POINT('',(25.7,-4.3371684861752,-12.255160934175));
#43425=CARTESIAN_POINT('',(21.5,-4.3371684861752,-12.255160934175));
#43426=CARTESIAN_POINT('',(25.7,-3.92451582856183,-12.0784177569485));
#43427=CARTESIAN_POINT('Origin',(25.7,-3.97859380257745,-12.2448526473001));
#43428=CARTESIAN_POINT('Origin',(25.7,0.,0.));
#43429=CARTESIAN_POINT('Origin',(17.3,-6.17858983848623,-11.5016315193869));
#43430=CARTESIAN_POINT('',(25.7,-6.20522725458991,-11.4234475846346));
#43431=CARTESIAN_POINT('',(17.3,-6.20522725458991,-11.4234475846346));
#43432=CARTESIAN_POINT('',(21.5,-6.20522725458991,-11.4234475846346));
#43433=CARTESIAN_POINT('',(25.7,-6.35000000000001,-10.9985226280624));
#43434=CARTESIAN_POINT('',(25.7,-6.17858983848623,-11.5016315193869));
#43435=CARTESIAN_POINT('',(17.3,-6.35000000000001,-10.9985226280624));
#43436=CARTESIAN_POINT('',(17.3,-6.35000000000001,-10.9985226280624));
#43437=CARTESIAN_POINT('',(17.3,-6.17858983848623,-11.5016315193869));
#43438=CARTESIAN_POINT('Origin',(17.3,-6.43750000000001,-11.1500770737246));
#43439=CARTESIAN_POINT('',(17.3,-6.79038217979862,-11.0856082310477));
#43440=CARTESIAN_POINT('Origin',(17.3,0.,0.));
#43441=CARTESIAN_POINT('',(17.3,-6.35000000000001,-10.9985226280624));
#43442=CARTESIAN_POINT('Origin',(17.3,-6.35000000000001,-10.9985226280624));
#43443=CARTESIAN_POINT('',(25.7,-6.79038217979862,-11.0856082310477));
#43444=CARTESIAN_POINT('',(21.5,-6.79038217979862,-11.0856082310477));
#43445=CARTESIAN_POINT('',(25.7,-6.35000000000001,-10.9985226280624));
#43446=CARTESIAN_POINT('Origin',(25.7,-6.43750000000001,-11.1500770737246));
#43447=CARTESIAN_POINT('Origin',(25.7,0.,0.));
#43448=CARTESIAN_POINT('Origin',(17.3,-8.43489648279215,-9.96569221502354));
#43449=CARTESIAN_POINT('',(25.7,-8.44469645337458,-9.88367855660851));
#43450=CARTESIAN_POINT('',(17.3,-8.44469645337458,-9.88367855660851));
#43451=CARTESIAN_POINT('',(21.5,-8.44469645337458,-9.88367855660851));
#43452=CARTESIAN_POINT('',(25.7,-8.4979587007575,-9.4379392835629));
#43453=CARTESIAN_POINT('',(25.7,-8.43489648279215,-9.96569221502354));
#43454=CARTESIAN_POINT('',(17.3,-8.4979587007575,-9.4379392835629));
#43455=CARTESIAN_POINT('',(17.3,-8.4979587007575,-9.4379392835629));
#43456=CARTESIAN_POINT('',(17.3,-8.43489648279215,-9.96569221502354));
#43457=CARTESIAN_POINT('Origin',(17.3,-8.6150565568703,-9.56798962802145));
#43458=CARTESIAN_POINT('',(17.3,-8.94682358829601,-9.43156125357356));
#43459=CARTESIAN_POINT('Origin',(17.3,0.,0.));
#43460=CARTESIAN_POINT('',(17.3,-8.4979587007575,-9.4379392835629));
#43461=CARTESIAN_POINT('Origin',(17.3,-8.4979587007575,-9.4379392835629));
#43462=CARTESIAN_POINT('',(25.7,-8.94682358829601,-9.43156125357356));
#43463=CARTESIAN_POINT('',(21.5,-8.94682358829601,-9.43156125357356));
#43464=CARTESIAN_POINT('',(25.7,-8.4979587007575,-9.4379392835629));
#43465=CARTESIAN_POINT('Origin',(25.7,-8.6150565568703,-9.56798962802145));
#43466=CARTESIAN_POINT('Origin',(25.7,0.,0.));
#43467=CARTESIAN_POINT('Origin',(17.3,-10.3225576756761,-7.99420434016675));
#43468=CARTESIAN_POINT('',(25.7,-10.3150918949973,-7.91194534850694));
#43469=CARTESIAN_POINT('',(17.3,-10.3150918949973,-7.91194534850694));
#43470=CARTESIAN_POINT('',(21.5,-10.3150918949973,-7.91194534850694));
#43471=CARTESIAN_POINT('',(25.7,-10.2745158285618,-7.46487270411441));
#43472=CARTESIAN_POINT('',(25.7,-10.3225576756761,-7.99420434016675));
#43473=CARTESIAN_POINT('',(17.3,-10.2745158285618,-7.46487270411441));
#43474=CARTESIAN_POINT('',(17.3,-10.2745158285618,-7.46487270411441));
#43475=CARTESIAN_POINT('',(17.3,-10.3225576756761,-7.99420434016675));
#43476=CARTESIAN_POINT('Origin',(17.3,-10.4160938025774,-7.56773512326559));
#43477=CARTESIAN_POINT('',(17.3,-10.7122458743621,-7.36530979166607));
#43478=CARTESIAN_POINT('Origin',(17.3,0.,0.));
#43479=CARTESIAN_POINT('',(17.3,-10.2745158285618,-7.46487270411441));
#43480=CARTESIAN_POINT('Origin',(17.3,-10.2745158285618,-7.46487270411441));
#43481=CARTESIAN_POINT('',(25.7,-10.7122458743621,-7.36530979166607));
#43482=CARTESIAN_POINT('',(21.5,-10.7122458743621,-7.36530979166607));
#43483=CARTESIAN_POINT('',(25.7,-10.2745158285618,-7.46487270411441));
#43484=CARTESIAN_POINT('Origin',(25.7,-10.4160938025774,-7.56773512326559));
#43485=CARTESIAN_POINT('Origin',(25.7,0.,0.));
#43486=CARTESIAN_POINT('Origin',(17.3,-11.7590735650056,-5.67333137519623));
#43487=CARTESIAN_POINT('',(25.7,-11.7346683235061,-5.59442216294959));
#43488=CARTESIAN_POINT('',(17.3,-11.7346683235061,-5.59442216294959));
#43489=CARTESIAN_POINT('',(21.5,-11.7346683235061,-5.59442216294959));
#43490=CARTESIAN_POINT('',(25.7,-11.602027312061,-5.16555536706266));
#43491=CARTESIAN_POINT('',(25.7,-11.7590735650056,-5.67333137519623));
#43492=CARTESIAN_POINT('',(17.3,-11.602027312061,-5.16555536706266));
#43493=CARTESIAN_POINT('',(17.3,-11.602027312061,-5.16555536706266));
#43494=CARTESIAN_POINT('',(17.3,-11.7590735650056,-5.67333137519623));
#43495=CARTESIAN_POINT('Origin',(17.3,-11.7618977671485,-5.23673427960092));
#43496=CARTESIAN_POINT('',(17.3,-12.0094916126598,-4.97715894918517));
#43497=CARTESIAN_POINT('Origin',(17.3,0.,0.));
#43498=CARTESIAN_POINT('',(17.3,-11.602027312061,-5.16555536706266));
#43499=CARTESIAN_POINT('Origin',(17.3,-11.602027312061,-5.16555536706266));
#43500=CARTESIAN_POINT('',(25.7,-12.0094916126598,-4.97715894918517));
#43501=CARTESIAN_POINT('',(21.5,-12.0094916126598,-4.97715894918517));
#43502=CARTESIAN_POINT('',(25.7,-11.602027312061,-5.16555536706266));
#43503=CARTESIAN_POINT('Origin',(25.7,-11.7618977671485,-5.23673427960092));
#43504=CARTESIAN_POINT('Origin',(25.7,0.,0.));
#43505=CARTESIAN_POINT('Origin',(17.3,-12.6816615132491,-3.10450660546528));
#43506=CARTESIAN_POINT('',(25.7,-12.6413834370917,-3.03239588385541));
#43507=CARTESIAN_POINT('',(17.3,-12.6413834370917,-3.03239588385541));
#43508=CARTESIAN_POINT('',(21.5,-12.6413834370917,-3.03239588385541));
#43509=CARTESIAN_POINT('',(25.7,-12.4224745293193,-2.64047847338554));
#43510=CARTESIAN_POINT('',(25.7,-12.6816615132491,-3.10450660546528));
#43511=CARTESIAN_POINT('',(17.3,-12.4224745293193,-2.64047847338554));
#43512=CARTESIAN_POINT('',(17.3,-12.4224745293193,-2.64047847338554));
#43513=CARTESIAN_POINT('',(17.3,-12.6816615132491,-3.10450660546528));
#43514=CARTESIAN_POINT('Origin',(17.3,-12.5936503594478,-2.67686301927865));
#43515=CARTESIAN_POINT('',(17.3,-12.7818649395498,-2.37148237756647));
#43516=CARTESIAN_POINT('Origin',(17.3,0.,0.));
#43517=CARTESIAN_POINT('',(17.3,-12.4224745293193,-2.64047847338554));
#43518=CARTESIAN_POINT('Origin',(17.3,-12.4224745293193,-2.64047847338554));
#43519=CARTESIAN_POINT('',(25.7,-12.7818649395498,-2.37148237756647));
#43520=CARTESIAN_POINT('',(21.5,-12.7818649395498,-2.37148237756647));
#43521=CARTESIAN_POINT('',(25.7,-12.4224745293193,-2.64047847338554));
#43522=CARTESIAN_POINT('Origin',(25.7,-12.5936503594478,-2.67686301927865));
#43523=CARTESIAN_POINT('Origin',(25.7,0.,0.));
#43524=CARTESIAN_POINT('Origin',(17.3,-13.05,-0.399999999999998));
#43525=CARTESIAN_POINT('',(25.7,-12.9956094343885,-0.337839353586883));
#43526=CARTESIAN_POINT('',(17.3,-12.9956094343885,-0.337839353586883));
#43527=CARTESIAN_POINT('',(21.5,-12.9956094343885,-0.337839353586883));
#43528=CARTESIAN_POINT('',(25.7,-12.7,1.55530143491714E-15));
#43529=CARTESIAN_POINT('',(25.7,-13.05,-0.399999999999998));
#43530=CARTESIAN_POINT('',(17.3,-12.7,1.55530143491714E-15));
#43531=CARTESIAN_POINT('',(17.3,-12.7,1.55530143491714E-15));
#43532=CARTESIAN_POINT('',(17.3,-13.05,-0.399999999999998));
#43533=CARTESIAN_POINT('Origin',(17.3,-12.875,1.57673275390222E-15));
#43534=CARTESIAN_POINT('',(17.3,-13.,-1.59204083889156E-15));
#43535=CARTESIAN_POINT('Origin',(17.3,0.,0.));
#43536=CARTESIAN_POINT('',(17.3,-12.9956094343885,0.337839353586885));
#43537=CARTESIAN_POINT('',(17.3,-12.7,1.55530143491714E-15));
#43538=CARTESIAN_POINT('Origin',(17.3,0.,0.));
#43539=CARTESIAN_POINT('Origin',(17.3,-12.7,1.55530143491714E-15));
#43540=CARTESIAN_POINT('',(25.7,-12.9956094343885,0.337839353586885));
#43541=CARTESIAN_POINT('',(21.5,-12.9956094343885,0.337839353586885));
#43542=CARTESIAN_POINT('',(25.7,-12.7,1.55530143491714E-15));
#43543=CARTESIAN_POINT('Origin',(25.7,-12.875,1.57673275390222E-15));
#43544=CARTESIAN_POINT('',(25.7,-13.,-1.59204083889156E-15));
#43545=CARTESIAN_POINT('Origin',(25.7,0.,0.));
#43546=CARTESIAN_POINT('Origin',(25.7,0.,0.));
#43547=CARTESIAN_POINT('Origin',(17.3,-12.8479908659033,2.32198852487824));
#43548=CARTESIAN_POINT('',(25.7,-12.7818649395498,2.37148237756648));
#43549=CARTESIAN_POINT('',(17.3,-12.7818649395498,2.37148237756648));
#43550=CARTESIAN_POINT('',(21.5,-12.7818649395498,2.37148237756648));
#43551=CARTESIAN_POINT('',(25.7,-12.4224745293193,2.64047847338555));
#43552=CARTESIAN_POINT('',(25.7,-12.8479908659033,2.32198852487824));
#43553=CARTESIAN_POINT('',(17.3,-12.4224745293193,2.64047847338555));
#43554=CARTESIAN_POINT('',(17.3,-12.4224745293193,2.64047847338555));
#43555=CARTESIAN_POINT('',(17.3,-12.8479908659033,2.32198852487824));
#43556=CARTESIAN_POINT('Origin',(17.3,-12.5936503594477,2.67686301927866));
#43557=CARTESIAN_POINT('',(17.3,-12.6413834370917,3.03239588385542));
#43558=CARTESIAN_POINT('Origin',(17.3,0.,0.));
#43559=CARTESIAN_POINT('',(17.3,-12.4224745293193,2.64047847338555));
#43560=CARTESIAN_POINT('Origin',(17.3,-12.4224745293193,2.64047847338555));
#43561=CARTESIAN_POINT('',(25.7,-12.6413834370917,3.03239588385542));
#43562=CARTESIAN_POINT('',(21.5,-12.6413834370917,3.03239588385542));
#43563=CARTESIAN_POINT('',(25.7,-12.4224745293193,2.64047847338555));
#43564=CARTESIAN_POINT('Origin',(25.7,-12.5936503594477,2.67686301927866));
#43565=CARTESIAN_POINT('Origin',(25.7,0.,0.));
#43566=CARTESIAN_POINT('Origin',(17.3,-12.0844628794663,4.94249500908216));
#43567=CARTESIAN_POINT('',(25.7,-12.0094916126598,4.97715894918518));
#43568=CARTESIAN_POINT('',(17.3,-12.0094916126598,4.97715894918518));
#43569=CARTESIAN_POINT('',(21.5,-12.0094916126598,4.97715894918518));
#43570=CARTESIAN_POINT('',(25.7,-11.602027312061,5.16555536706267));
#43571=CARTESIAN_POINT('',(25.7,-12.0844628794663,4.94249500908216));
#43572=CARTESIAN_POINT('',(17.3,-11.602027312061,5.16555536706267));
#43573=CARTESIAN_POINT('',(17.3,-11.602027312061,5.16555536706267));
#43574=CARTESIAN_POINT('',(17.3,-12.0844628794663,4.94249500908216));
#43575=CARTESIAN_POINT('Origin',(17.3,-11.7618977671485,5.23673427960093));
#43576=CARTESIAN_POINT('',(17.3,-11.7346683235061,5.5944221629496));
#43577=CARTESIAN_POINT('Origin',(17.3,0.,0.));
#43578=CARTESIAN_POINT('',(17.3,-11.602027312061,5.16555536706267));
#43579=CARTESIAN_POINT('Origin',(17.3,-11.602027312061,5.16555536706267));
#43580=CARTESIAN_POINT('',(25.7,-11.7346683235061,5.5944221629496));
#43581=CARTESIAN_POINT('',(21.5,-11.7346683235061,5.5944221629496));
#43582=CARTESIAN_POINT('',(25.7,-11.602027312061,5.16555536706267));
#43583=CARTESIAN_POINT('Origin',(25.7,-11.7618977671485,5.23673427960093));
#43584=CARTESIAN_POINT('Origin',(25.7,0.,0.));
#43585=CARTESIAN_POINT('Origin',(17.3,-10.7927858775101,7.3469907446668));
#43586=CARTESIAN_POINT('',(25.7,-10.7122458743621,7.36530979166607));
#43587=CARTESIAN_POINT('',(17.3,-10.7122458743621,7.36530979166607));
#43588=CARTESIAN_POINT('',(21.5,-10.7122458743621,7.36530979166607));
#43589=CARTESIAN_POINT('',(25.7,-10.2745158285618,7.46487270411441));
#43590=CARTESIAN_POINT('',(25.7,-10.7927858775101,7.3469907446668));
#43591=CARTESIAN_POINT('',(17.3,-10.2745158285618,7.46487270411441));
#43592=CARTESIAN_POINT('',(17.3,-10.2745158285618,7.46487270411441));
#43593=CARTESIAN_POINT('',(17.3,-10.7927858775101,7.3469907446668));
#43594=CARTESIAN_POINT('Origin',(17.3,-10.4160938025774,7.56773512326559));
#43595=CARTESIAN_POINT('',(17.3,-10.3150918949973,7.91194534850694));
#43596=CARTESIAN_POINT('Origin',(17.3,0.,0.));
#43597=CARTESIAN_POINT('',(17.3,-10.2745158285618,7.46487270411441));
#43598=CARTESIAN_POINT('Origin',(17.3,-10.2745158285618,7.46487270411441));
#43599=CARTESIAN_POINT('',(25.7,-10.3150918949973,7.91194534850694));
#43600=CARTESIAN_POINT('',(21.5,-10.3150918949973,7.91194534850694));
#43601=CARTESIAN_POINT('',(25.7,-10.2745158285618,7.46487270411441));
#43602=CARTESIAN_POINT('Origin',(25.7,-10.4160938025774,7.56773512326559));
#43603=CARTESIAN_POINT('Origin',(25.7,0.,0.));
#43604=CARTESIAN_POINT('Origin',(17.3,-9.02941234317406,9.43038772993646));
#43605=CARTESIAN_POINT('',(25.7,-8.94682358829601,9.43156125357357));
#43606=CARTESIAN_POINT('',(17.3,-8.94682358829601,9.43156125357357));
#43607=CARTESIAN_POINT('',(21.5,-8.94682358829601,9.43156125357357));
#43608=CARTESIAN_POINT('',(25.7,-8.4979587007575,9.43793928356291));
#43609=CARTESIAN_POINT('',(25.7,-9.02941234317406,9.43038772993646));
#43610=CARTESIAN_POINT('',(17.3,-8.4979587007575,9.43793928356291));
#43611=CARTESIAN_POINT('',(17.3,-8.4979587007575,9.43793928356291));
#43612=CARTESIAN_POINT('',(17.3,-9.02941234317406,9.43038772993646));
#43613=CARTESIAN_POINT('Origin',(17.3,-8.6150565568703,9.56798962802145));
#43614=CARTESIAN_POINT('',(17.3,-8.44469645337457,9.88367855660852));
#43615=CARTESIAN_POINT('Origin',(17.3,0.,0.));
#43616=CARTESIAN_POINT('',(17.3,-8.4979587007575,9.43793928356291));
#43617=CARTESIAN_POINT('Origin',(17.3,-8.4979587007575,9.43793928356291));
#43618=CARTESIAN_POINT('',(25.7,-8.44469645337457,9.88367855660852));
#43619=CARTESIAN_POINT('',(21.5,-8.44469645337457,9.88367855660852));
#43620=CARTESIAN_POINT('',(25.7,-8.4979587007575,9.43793928356291));
#43621=CARTESIAN_POINT('Origin',(25.7,-8.6150565568703,9.56798962802145));
#43622=CARTESIAN_POINT('Origin',(25.7,0.,0.));
#43623=CARTESIAN_POINT('Origin',(17.3,-6.87141016151377,11.1016315193869));
#43624=CARTESIAN_POINT('',(25.7,-6.79038217979861,11.0856082310477));
#43625=CARTESIAN_POINT('',(17.3,-6.79038217979861,11.0856082310477));
#43626=CARTESIAN_POINT('',(21.5,-6.79038217979861,11.0856082310477));
#43627=CARTESIAN_POINT('',(25.7,-6.35,10.9985226280624));
#43628=CARTESIAN_POINT('',(25.7,-6.87141016151377,11.1016315193869));
#43629=CARTESIAN_POINT('',(17.3,-6.35,10.9985226280624));
#43630=CARTESIAN_POINT('',(17.3,-6.35,10.9985226280624));
#43631=CARTESIAN_POINT('',(17.3,-6.87141016151377,11.1016315193869));
#43632=CARTESIAN_POINT('Origin',(17.3,-6.4375,11.1500770737247));
#43633=CARTESIAN_POINT('',(17.3,-6.2052272545899,11.4234475846346));
#43634=CARTESIAN_POINT('Origin',(17.3,0.,0.));
#43635=CARTESIAN_POINT('',(17.3,-6.35,10.9985226280624));
#43636=CARTESIAN_POINT('Origin',(17.3,-6.35,10.9985226280624));
#43637=CARTESIAN_POINT('',(25.7,-6.2052272545899,11.4234475846346));
#43638=CARTESIAN_POINT('',(21.5,-6.2052272545899,11.4234475846346));
#43639=CARTESIAN_POINT('',(25.7,-6.35,10.9985226280624));
#43640=CARTESIAN_POINT('Origin',(25.7,-6.4375,11.1500770737247));
#43641=CARTESIAN_POINT('Origin',(25.7,0.,0.));
#43642=CARTESIAN_POINT('Origin',(17.3,-4.41309438311112,12.2876807399018));
#43643=CARTESIAN_POINT('',(25.7,-4.3371684861752,12.255160934175));
#43644=CARTESIAN_POINT('',(17.3,-4.3371684861752,12.255160934175));
#43645=CARTESIAN_POINT('',(21.5,-4.3371684861752,12.255160934175));
#43646=CARTESIAN_POINT('',(25.7,-3.92451582856183,12.0784177569485));
#43647=CARTESIAN_POINT('',(25.7,-4.41309438311112,12.2876807399018));
#43648=CARTESIAN_POINT('',(17.3,-3.92451582856183,12.0784177569485));
#43649=CARTESIAN_POINT('',(17.3,-3.92451582856183,12.0784177569485));
#43650=CARTESIAN_POINT('',(17.3,-4.41309438311112,12.2876807399018));
#43651=CARTESIAN_POINT('Origin',(17.3,-3.97859380257745,12.2448526473001));
#43652=CARTESIAN_POINT('',(17.3,-3.6945598487957,12.463957137429));
#43653=CARTESIAN_POINT('Origin',(17.3,0.,0.));
#43654=CARTESIAN_POINT('',(17.3,-3.92451582856183,12.0784177569485));
#43655=CARTESIAN_POINT('Origin',(17.3,-3.92451582856183,12.0784177569485));
#43656=CARTESIAN_POINT('',(25.7,-3.6945598487957,12.463957137429));
#43657=CARTESIAN_POINT('',(21.5,-3.6945598487957,12.463957137429));
#43658=CARTESIAN_POINT('',(25.7,-3.92451582856183,12.0784177569485));
#43659=CARTESIAN_POINT('Origin',(25.7,-3.97859380257745,12.2448526473001));
#43660=CARTESIAN_POINT('Origin',(25.7,0.,0.));
#43661=CARTESIAN_POINT('Origin',(17.3,-1.76190520379019,12.9366993492489));
#43662=CARTESIAN_POINT('',(25.7,-1.69439971766247,12.8891042976921));
#43663=CARTESIAN_POINT('',(17.3,-1.69439971766247,12.8891042976921));
#43664=CARTESIAN_POINT('',(21.5,-1.69439971766247,12.8891042976921));
#43665=CARTESIAN_POINT('',(25.7,-1.3275114834992,12.6304280711771));
#43666=CARTESIAN_POINT('',(25.7,-1.76190520379019,12.9366993492489));
#43667=CARTESIAN_POINT('',(17.3,-1.3275114834992,12.6304280711771));
#43668=CARTESIAN_POINT('',(17.3,-1.3275114834992,12.6304280711771));
#43669=CARTESIAN_POINT('',(17.3,-1.76190520379019,12.9366993492489));
#43670=CARTESIAN_POINT('Origin',(17.3,-1.34580396457104,12.8044694028665));
#43671=CARTESIAN_POINT('',(17.3,-1.02242244914403,12.9597319546157));
#43672=CARTESIAN_POINT('Origin',(17.3,0.,0.));
#43673=CARTESIAN_POINT('',(17.3,-1.3275114834992,12.6304280711771));
#43674=CARTESIAN_POINT('Origin',(17.3,-1.3275114834992,12.6304280711771));
#43675=CARTESIAN_POINT('',(25.7,-1.02242244914403,12.9597319546157));
#43676=CARTESIAN_POINT('',(21.5,-1.02242244914403,12.9597319546157));
#43677=CARTESIAN_POINT('',(25.7,-1.3275114834992,12.6304280711771));
#43678=CARTESIAN_POINT('Origin',(25.7,-1.34580396457104,12.8044694028665));
#43679=CARTESIAN_POINT('Origin',(25.7,0.,0.));
#43680=CARTESIAN_POINT('Origin',(17.3,0.966287687495571,13.020322119863));
#43681=CARTESIAN_POINT('',(25.7,1.02242244914404,12.9597319546157));
#43682=CARTESIAN_POINT('',(17.3,1.02242244914404,12.9597319546157));
#43683=CARTESIAN_POINT('',(21.5,1.02242244914404,12.9597319546157));
#43684=CARTESIAN_POINT('',(25.7,1.3275114834992,12.6304280711771));
#43685=CARTESIAN_POINT('',(25.7,0.966287687495571,13.020322119863));
#43686=CARTESIAN_POINT('',(17.3,1.3275114834992,12.6304280711771));
#43687=CARTESIAN_POINT('',(17.3,1.3275114834992,12.6304280711771));
#43688=CARTESIAN_POINT('',(17.3,0.966287687495571,13.020322119863));
#43689=CARTESIAN_POINT('Origin',(17.3,1.34580396457104,12.8044694028665));
#43690=CARTESIAN_POINT('',(17.3,1.69439971766247,12.8891042976921));
#43691=CARTESIAN_POINT('Origin',(17.3,0.,0.));
#43692=CARTESIAN_POINT('',(17.3,1.3275114834992,12.6304280711771));
#43693=CARTESIAN_POINT('Origin',(17.3,1.3275114834992,12.6304280711771));
#43694=CARTESIAN_POINT('',(25.7,1.69439971766247,12.8891042976921));
#43695=CARTESIAN_POINT('',(21.5,1.69439971766247,12.8891042976921));
#43696=CARTESIAN_POINT('',(25.7,1.3275114834992,12.6304280711771));
#43697=CARTESIAN_POINT('Origin',(25.7,1.34580396457104,12.8044694028665));
#43698=CARTESIAN_POINT('Origin',(25.7,0.,0.));
#43699=CARTESIAN_POINT('Origin',(17.3,3.652249170075,12.5348943354017));
#43700=CARTESIAN_POINT('',(25.7,3.69455984879571,12.463957137429));
#43701=CARTESIAN_POINT('',(17.3,3.69455984879571,12.463957137429));
#43702=CARTESIAN_POINT('',(21.5,3.69455984879571,12.463957137429));
#43703=CARTESIAN_POINT('',(25.7,3.92451582856183,12.0784177569485));
#43704=CARTESIAN_POINT('',(25.7,3.652249170075,12.5348943354017));
#43705=CARTESIAN_POINT('',(17.3,3.92451582856183,12.0784177569485));
#43706=CARTESIAN_POINT('',(17.3,3.92451582856183,12.0784177569485));
#43707=CARTESIAN_POINT('',(17.3,3.652249170075,12.5348943354017));
#43708=CARTESIAN_POINT('Origin',(17.3,3.97859380257745,12.2448526473001));
#43709=CARTESIAN_POINT('',(17.3,4.3371684861752,12.255160934175));
#43710=CARTESIAN_POINT('Origin',(17.3,0.,0.));
#43711=CARTESIAN_POINT('',(17.3,3.92451582856183,12.0784177569485));
#43712=CARTESIAN_POINT('Origin',(17.3,3.92451582856183,12.0784177569485));
#43713=CARTESIAN_POINT('',(25.7,4.3371684861752,12.255160934175));
#43714=CARTESIAN_POINT('',(21.5,4.3371684861752,12.255160934175));
#43715=CARTESIAN_POINT('',(25.7,3.92451582856183,12.0784177569485));
#43716=CARTESIAN_POINT('Origin',(25.7,3.97859380257745,12.2448526473001));
#43717=CARTESIAN_POINT('Origin',(25.7,0.,0.));
#43718=CARTESIAN_POINT('Origin',(17.3,6.17858983848623,11.5016315193869));
#43719=CARTESIAN_POINT('',(25.7,6.20522725458991,11.4234475846346));
#43720=CARTESIAN_POINT('',(17.3,6.20522725458991,11.4234475846346));
#43721=CARTESIAN_POINT('',(21.5,6.20522725458991,11.4234475846346));
#43722=CARTESIAN_POINT('',(25.7,6.35,10.9985226280624));
#43723=CARTESIAN_POINT('',(25.7,6.17858983848623,11.5016315193869));
#43724=CARTESIAN_POINT('',(17.3,6.35,10.9985226280624));
#43725=CARTESIAN_POINT('',(17.3,6.35,10.9985226280624));
#43726=CARTESIAN_POINT('',(17.3,6.17858983848623,11.5016315193869));
#43727=CARTESIAN_POINT('Origin',(17.3,6.4375,11.1500770737246));
#43728=CARTESIAN_POINT('',(17.3,6.79038217979862,11.0856082310477));
#43729=CARTESIAN_POINT('Origin',(17.3,0.,0.));
#43730=CARTESIAN_POINT('',(17.3,6.35,10.9985226280624));
#43731=CARTESIAN_POINT('Origin',(17.3,6.35,10.9985226280624));
#43732=CARTESIAN_POINT('',(25.7,6.79038217979862,11.0856082310477));
#43733=CARTESIAN_POINT('',(21.5,6.79038217979862,11.0856082310477));
#43734=CARTESIAN_POINT('',(25.7,6.35,10.9985226280624));
#43735=CARTESIAN_POINT('Origin',(25.7,6.4375,11.1500770737246));
#43736=CARTESIAN_POINT('Origin',(25.7,0.,0.));
#43737=CARTESIAN_POINT('Origin',(17.3,8.43489648279215,9.96569221502354));
#43738=CARTESIAN_POINT('',(25.7,8.44469645337458,9.88367855660851));
#43739=CARTESIAN_POINT('',(17.3,8.44469645337458,9.88367855660851));
#43740=CARTESIAN_POINT('',(21.5,8.44469645337458,9.88367855660851));
#43741=CARTESIAN_POINT('',(25.7,8.4979587007575,9.43793928356291));
#43742=CARTESIAN_POINT('',(25.7,8.43489648279215,9.96569221502354));
#43743=CARTESIAN_POINT('',(17.3,8.4979587007575,9.43793928356291));
#43744=CARTESIAN_POINT('',(17.3,8.4979587007575,9.43793928356291));
#43745=CARTESIAN_POINT('',(17.3,8.43489648279215,9.96569221502354));
#43746=CARTESIAN_POINT('Origin',(17.3,8.6150565568703,9.56798962802145));
#43747=CARTESIAN_POINT('',(17.3,8.94682358829601,9.43156125357356));
#43748=CARTESIAN_POINT('Origin',(17.3,0.,0.));
#43749=CARTESIAN_POINT('',(17.3,8.4979587007575,9.43793928356291));
#43750=CARTESIAN_POINT('Origin',(17.3,8.4979587007575,9.43793928356291));
#43751=CARTESIAN_POINT('',(25.7,8.94682358829601,9.43156125357356));
#43752=CARTESIAN_POINT('',(21.5,8.94682358829601,9.43156125357356));
#43753=CARTESIAN_POINT('',(25.7,8.4979587007575,9.43793928356291));
#43754=CARTESIAN_POINT('Origin',(25.7,8.6150565568703,9.56798962802145));
#43755=CARTESIAN_POINT('Origin',(25.7,0.,0.));
#43756=CARTESIAN_POINT('Origin',(17.3,10.3225576756761,7.99420434016675));
#43757=CARTESIAN_POINT('',(25.7,10.3150918949973,7.91194534850694));
#43758=CARTESIAN_POINT('',(17.3,10.3150918949973,7.91194534850694));
#43759=CARTESIAN_POINT('',(21.5,10.3150918949973,7.91194534850694));
#43760=CARTESIAN_POINT('',(25.7,10.2745158285618,7.46487270411441));
#43761=CARTESIAN_POINT('',(25.7,10.3225576756761,7.99420434016675));
#43762=CARTESIAN_POINT('',(17.3,10.2745158285618,7.46487270411441));
#43763=CARTESIAN_POINT('',(17.3,10.2745158285618,7.46487270411441));
#43764=CARTESIAN_POINT('',(17.3,10.3225576756761,7.99420434016675));
#43765=CARTESIAN_POINT('Origin',(17.3,10.4160938025774,7.56773512326559));
#43766=CARTESIAN_POINT('',(17.3,10.7122458743621,7.36530979166607));
#43767=CARTESIAN_POINT('Origin',(17.3,0.,0.));
#43768=CARTESIAN_POINT('',(17.3,10.2745158285618,7.46487270411441));
#43769=CARTESIAN_POINT('Origin',(17.3,10.2745158285618,7.46487270411441));
#43770=CARTESIAN_POINT('',(25.7,10.7122458743621,7.36530979166607));
#43771=CARTESIAN_POINT('',(21.5,10.7122458743621,7.36530979166607));
#43772=CARTESIAN_POINT('',(25.7,10.2745158285618,7.46487270411441));
#43773=CARTESIAN_POINT('Origin',(25.7,10.4160938025774,7.56773512326559));
#43774=CARTESIAN_POINT('Origin',(25.7,0.,0.));
#43775=CARTESIAN_POINT('Origin',(17.3,11.7590735650056,5.67333137519623));
#43776=CARTESIAN_POINT('',(25.7,11.7346683235061,5.59442216294959));
#43777=CARTESIAN_POINT('',(17.3,11.7346683235061,5.59442216294959));
#43778=CARTESIAN_POINT('',(21.5,11.7346683235061,5.59442216294959));
#43779=CARTESIAN_POINT('',(25.7,11.602027312061,5.16555536706266));
#43780=CARTESIAN_POINT('',(25.7,11.7590735650056,5.67333137519623));
#43781=CARTESIAN_POINT('',(17.3,11.602027312061,5.16555536706266));
#43782=CARTESIAN_POINT('',(17.3,11.602027312061,5.16555536706266));
#43783=CARTESIAN_POINT('',(17.3,11.7590735650056,5.67333137519623));
#43784=CARTESIAN_POINT('Origin',(17.3,11.7618977671485,5.23673427960093));
#43785=CARTESIAN_POINT('',(17.3,12.0094916126598,4.97715894918518));
#43786=CARTESIAN_POINT('Origin',(17.3,0.,0.));
#43787=CARTESIAN_POINT('',(17.3,11.602027312061,5.16555536706266));
#43788=CARTESIAN_POINT('Origin',(17.3,11.602027312061,5.16555536706266));
#43789=CARTESIAN_POINT('',(25.7,12.0094916126598,4.97715894918518));
#43790=CARTESIAN_POINT('',(21.5,12.0094916126598,4.97715894918518));
#43791=CARTESIAN_POINT('',(25.7,11.602027312061,5.16555536706266));
#43792=CARTESIAN_POINT('Origin',(25.7,11.7618977671485,5.23673427960093));
#43793=CARTESIAN_POINT('Origin',(25.7,0.,0.));
#43794=CARTESIAN_POINT('Origin',(17.3,12.6816615132491,3.10450660546528));
#43795=CARTESIAN_POINT('',(25.7,12.6413834370917,3.03239588385541));
#43796=CARTESIAN_POINT('',(17.3,12.6413834370917,3.03239588385541));
#43797=CARTESIAN_POINT('',(21.5,12.6413834370917,3.03239588385541));
#43798=CARTESIAN_POINT('',(25.7,12.4224745293193,2.64047847338554));
#43799=CARTESIAN_POINT('',(25.7,12.6816615132491,3.10450660546528));
#43800=CARTESIAN_POINT('',(17.3,12.4224745293193,2.64047847338554));
#43801=CARTESIAN_POINT('',(17.3,12.4224745293193,2.64047847338554));
#43802=CARTESIAN_POINT('',(17.3,12.6816615132491,3.10450660546528));
#43803=CARTESIAN_POINT('Origin',(17.3,12.5936503594478,2.67686301927865));
#43804=CARTESIAN_POINT('',(17.3,12.7818649395498,2.37148237756647));
#43805=CARTESIAN_POINT('Origin',(17.3,0.,0.));
#43806=CARTESIAN_POINT('',(17.3,12.4224745293193,2.64047847338554));
#43807=CARTESIAN_POINT('Origin',(17.3,12.4224745293193,2.64047847338554));
#43808=CARTESIAN_POINT('',(25.7,12.7818649395498,2.37148237756647));
#43809=CARTESIAN_POINT('',(21.5,12.7818649395498,2.37148237756647));
#43810=CARTESIAN_POINT('',(25.7,12.4224745293193,2.64047847338554));
#43811=CARTESIAN_POINT('Origin',(25.7,12.5936503594478,2.67686301927865));
#43812=CARTESIAN_POINT('Origin',(25.7,0.,0.));
#43813=CARTESIAN_POINT('Origin',(17.3,13.05,0.4));
#43814=CARTESIAN_POINT('',(25.7,12.9956094343885,0.337839353586883));
#43815=CARTESIAN_POINT('',(17.3,12.9956094343885,0.337839353586883));
#43816=CARTESIAN_POINT('',(21.5,12.9956094343885,0.337839353586883));
#43817=CARTESIAN_POINT('',(25.7,12.7,0.));
#43818=CARTESIAN_POINT('',(25.7,13.05,0.4));
#43819=CARTESIAN_POINT('',(17.3,12.7,0.));
#43820=CARTESIAN_POINT('',(17.3,12.7,0.));
#43821=CARTESIAN_POINT('',(17.3,13.05,0.4));
#43822=CARTESIAN_POINT('Origin',(17.3,12.875,0.));
#43823=CARTESIAN_POINT('',(17.3,12.9956094343885,-0.337839353586884));
#43824=CARTESIAN_POINT('Origin',(17.3,0.,0.));
#43825=CARTESIAN_POINT('',(17.3,12.7,0.));
#43826=CARTESIAN_POINT('Origin',(17.3,12.7,0.));
#43827=CARTESIAN_POINT('',(25.7,12.9956094343885,-0.337839353586884));
#43828=CARTESIAN_POINT('',(21.5,12.9956094343885,-0.337839353586884));
#43829=CARTESIAN_POINT('',(25.7,12.7,0.));
#43830=CARTESIAN_POINT('Origin',(25.7,12.875,0.));
#43831=CARTESIAN_POINT('Origin',(25.7,0.,0.));
#43832=CARTESIAN_POINT('Origin',(0.,1.5,0.));
#43833=CARTESIAN_POINT('',(2.77555756156289E-16,-1.5,-1.83697019872103E-16));
#43834=CARTESIAN_POINT('Origin',(0.,0.,0.));
#43835=CARTESIAN_POINT('Origin',(1.,0.,0.));
#43836=CARTESIAN_POINT('',(2.,-4.5,-5.51091059616309E-16));
#43837=CARTESIAN_POINT('Origin',(2.,0.,0.));
#43838=CARTESIAN_POINT('',(1.,-3.,-3.67394039744206E-16));
#43839=CARTESIAN_POINT('Origin',(2.25,0.,0.));
#43840=CARTESIAN_POINT('',(2.25,-4.75,-5.81707229594993E-16));
#43841=CARTESIAN_POINT('Origin',(8.75,0.,0.));
#43842=CARTESIAN_POINT('Origin',(15.75,0.,0.));
#43843=CARTESIAN_POINT('',(16.5,-4.,-4.89858719658941E-16));
#43844=CARTESIAN_POINT('Origin',(16.5,0.,0.));
#43845=CARTESIAN_POINT('',(15.75,-4.,-4.89858719658941E-16));
#43846=CARTESIAN_POINT('Origin',(16.5,12.4,0.));
#43847=CARTESIAN_POINT('',(16.5,-12.4,-1.51856203094272E-15));
#43848=CARTESIAN_POINT('Origin',(16.5,0.,0.));
#43849=CARTESIAN_POINT('Origin',(16.8,0.,0.));
#43850=CARTESIAN_POINT('',(17.1,-13.,-1.59204083889156E-15));
#43851=CARTESIAN_POINT('Origin',(17.1,0.,0.));
#43852=CARTESIAN_POINT('',(16.8,-12.7,-1.55530143491714E-15));
#43853=CARTESIAN_POINT('Origin',(21.5,0.,0.));
#43854=CARTESIAN_POINT('',(25.9,-13.,-1.59204083889156E-15));
#43855=CARTESIAN_POINT('Origin',(25.9,0.,0.));
#43856=CARTESIAN_POINT('',(21.5,-13.,-1.59204083889156E-15));
#43857=CARTESIAN_POINT('',(21.5,-13.,-1.59204083889156E-15));
#43858=CARTESIAN_POINT('Origin',(26.2,0.,0.));
#43859=CARTESIAN_POINT('',(26.5,-12.4,-1.51856203094272E-15));
#43860=CARTESIAN_POINT('Origin',(26.5,0.,0.));
#43861=CARTESIAN_POINT('',(26.2,-12.7,-1.55530143491714E-15));
#43862=CARTESIAN_POINT('Origin',(26.5,0.,0.));
#43863=CARTESIAN_POINT('',(0.,0.,0.));
#43864=CARTESIAN_POINT('Origin',(0.249999999999999,-12.,6.75));
#43865=CARTESIAN_POINT('',(0.499999999999998,-8.1,6.5));
#43866=CARTESIAN_POINT('',(0.,-8.1,7.));
#43867=CARTESIAN_POINT('',(7.62499999999997,-8.1,-0.625000000000007));
#43868=CARTESIAN_POINT('',(0.,8.1,7.));
#43869=CARTESIAN_POINT('',(0.,-12.,7.));
#43870=CARTESIAN_POINT('',(0.499999999999998,8.1,6.5));
#43871=CARTESIAN_POINT('',(7.62499999999997,8.1,-0.625000000000007));
#43872=CARTESIAN_POINT('',(0.499999999999998,-12.,6.5));
#43873=CARTESIAN_POINT('Origin',(0.,-12.,6.5));
#43874=CARTESIAN_POINT('',(0.,-8.1,8.5));
#43875=CARTESIAN_POINT('',(0.,-8.1,3.25));
#43876=CARTESIAN_POINT('',(0.,8.1,8.5));
#43877=CARTESIAN_POINT('',(0.,-1.95,8.5));
#43878=CARTESIAN_POINT('',(0.,8.1,3.25));
#43879=CARTESIAN_POINT('Origin',(45.25,-12.,-6.75));
#43880=CARTESIAN_POINT('',(45.5,-8.1,-7.));
#43881=CARTESIAN_POINT('',(45.,-8.1,-6.5));
#43882=CARTESIAN_POINT('',(38.,-8.1,0.500000000000009));
#43883=CARTESIAN_POINT('',(45.,8.1,-6.5));
#43884=CARTESIAN_POINT('',(45.,-12.,-6.5));
#43885=CARTESIAN_POINT('',(45.5,8.1,-7.));
#43886=CARTESIAN_POINT('',(38.,8.1,0.500000000000009));
#43887=CARTESIAN_POINT('',(45.5,-12.,-7.));
#43888=CARTESIAN_POINT('Origin',(45.,-12.,-7.));
#43889=CARTESIAN_POINT('',(45.,-8.1,6.5));
#43890=CARTESIAN_POINT('',(45.,-8.1,-3.5));
#43891=CARTESIAN_POINT('',(45.,8.1,6.5));
#43892=CARTESIAN_POINT('',(45.,-12.,6.5));
#43893=CARTESIAN_POINT('',(45.,8.1,-3.5));
#43894=CARTESIAN_POINT('Origin',(26.8600318979269,-8.35,-9.00039872408616));
#43895=CARTESIAN_POINT('',(29.9800318980078,-8.1,-8.5));
#43896=CARTESIAN_POINT('',(48.7300318980078,-8.1,-7.));
#43897=CARTESIAN_POINT('',(26.8400955923562,-8.1,-8.75119490445213));
#43898=CARTESIAN_POINT('',(54.5384025518406,-8.56318980889132,-7.));
#43899=CARTESIAN_POINT('',(41.1437308530539,-7.49502873686523,-7.));
#43900=CARTESIAN_POINT('',(54.5015923607319,-8.6,-7.03987261114144));
#43901=CARTESIAN_POINT('',(51.2914447078965,-11.8101476528355,-10.5170881651225));
#43902=CARTESIAN_POINT('',(30.,-8.6,-9.));
#43903=CARTESIAN_POINT('',(26.8799682034976,-8.6,-9.24960254372019));
#43904=CARTESIAN_POINT('',(30.,-8.6,-9.));
#43905=CARTESIAN_POINT('Origin',(11.5,-8.35,-8.75));
#43906=CARTESIAN_POINT('',(0.,-8.6,-9.));
#43907=CARTESIAN_POINT('',(11.5,-8.6,-9.));
#43908=CARTESIAN_POINT('',(0.,-8.1,-8.5));
#43909=CARTESIAN_POINT('',(0.,-8.6,-9.));
#43910=CARTESIAN_POINT('',(11.5,-8.1,-8.5));
#43911=CARTESIAN_POINT('Origin',(0.,-8.35,0.));
#43912=CARTESIAN_POINT('',(0.,-8.6,9.));
#43913=CARTESIAN_POINT('',(0.,-8.6,9.));
#43914=CARTESIAN_POINT('Origin',(0.,-8.1,0.));
#43915=CARTESIAN_POINT('Origin',(0.,-8.6,0.));
#43916=CARTESIAN_POINT('Origin',(11.5,-8.35,8.75));
#43917=CARTESIAN_POINT('',(0.499999999999998,-8.6,9.));
#43918=CARTESIAN_POINT('',(1.05833333333333,-9.15833333333333,9.55833333333333));
#43919=CARTESIAN_POINT('',(11.5,-8.6,9.));
#43920=CARTESIAN_POINT('Origin',(23.,-8.1,0.));
#43921=CARTESIAN_POINT('',(34.,-8.1,6.5));
#43922=CARTESIAN_POINT('',(39.,-8.1,-7.));
#43923=CARTESIAN_POINT('',(12.95,-8.1,-2.));
#43924=CARTESIAN_POINT('Origin',(16.,-8.1,-2.));
#43925=CARTESIAN_POINT('',(-3.05,-8.1,-3.73517273739943E-16));
#43926=CARTESIAN_POINT('Origin',(0.,-8.1,0.));
#43927=CARTESIAN_POINT('Origin',(39.3600318979269,8.35,-8.00039872408616));
#43928=CARTESIAN_POINT('',(30.,8.6,-9.));
#43929=CARTESIAN_POINT('',(54.5015923607319,8.6,-7.03987261114144));
#43930=CARTESIAN_POINT('',(39.3799682034976,8.6,-8.24960254372019));
#43931=CARTESIAN_POINT('',(54.5384025518406,8.56318980889132,-7.));
#43932=CARTESIAN_POINT('',(52.1553995139966,10.9461928467353,-9.58125672850473));
#43933=CARTESIAN_POINT('',(48.7300318980078,8.1,-7.));
#43934=CARTESIAN_POINT('',(46.4033407459587,7.91445749689621,-7.));
#43935=CARTESIAN_POINT('',(29.9800318980078,8.1,-8.5));
#43936=CARTESIAN_POINT('',(39.3400955923562,8.1,-7.75119490445213));
#43937=CARTESIAN_POINT('',(29.9800318980078,8.1,-8.5));
#43938=CARTESIAN_POINT('Origin',(11.5,8.35,8.75));
#43939=CARTESIAN_POINT('',(0.499999999999998,8.6,9.));
#43940=CARTESIAN_POINT('',(0.408333333333332,8.50833333333333,8.90833333333333));
#43941=CARTESIAN_POINT('',(0.,8.6,9.));
#43942=CARTESIAN_POINT('',(11.5,8.6,9.));
#43943=CARTESIAN_POINT('',(0.,8.6,9.));
#43944=CARTESIAN_POINT('Origin',(0.,8.35,0.));
#43945=CARTESIAN_POINT('',(0.,8.6,-9.));
#43946=CARTESIAN_POINT('Origin',(0.,8.6,0.));
#43947=CARTESIAN_POINT('',(0.,8.1,-8.5));
#43948=CARTESIAN_POINT('',(0.,8.6,-9.));
#43949=CARTESIAN_POINT('Origin',(0.,8.1,0.));
#43950=CARTESIAN_POINT('Origin',(26.5,8.35,-8.75));
#43951=CARTESIAN_POINT('',(26.5,8.1,-8.5));
#43952=CARTESIAN_POINT('',(26.5,8.6,-9.));
#43953=CARTESIAN_POINT('Origin',(54.750796180366,8.1,-6.76993630557072));
#43954=CARTESIAN_POINT('',(54.5384025518406,3.87298334620742,-7.));
#43955=CARTESIAN_POINT('',(54.5384025518406,-1.95,-7.));
#43956=CARTESIAN_POINT('',(54.5015923607319,11.,-7.03987261114144));
#43957=CARTESIAN_POINT('',(54.5015923607319,8.1,-7.03987261114144));
#43958=CARTESIAN_POINT('',(55.,11.,-6.5));
#43959=CARTESIAN_POINT('',(55.,11.,-6.5));
#43960=CARTESIAN_POINT('',(55.,4.66368952654441,-6.5));
#43961=CARTESIAN_POINT('',(55.,8.1,-6.5));
#43962=CARTESIAN_POINT('Origin',(61.0007668260719,0.,0.));
#43963=CARTESIAN_POINT('Origin',(55.,8.1,-7.));
#43964=CARTESIAN_POINT('',(30.,11.,-9.));
#43965=CARTESIAN_POINT('',(30.,8.1,-9.));
#43966=CARTESIAN_POINT('',(39.3799682034976,11.,-8.24960254372019));
#43967=CARTESIAN_POINT('Origin',(30.,8.1,-9.));
#43968=CARTESIAN_POINT('',(0.,11.,-9.));
#43969=CARTESIAN_POINT('',(0.,8.1,-9.));
#43970=CARTESIAN_POINT('',(26.5,11.,-9.));
#43971=CARTESIAN_POINT('Origin',(0.,8.1,0.));
#43972=CARTESIAN_POINT('',(0.,11.,9.));
#43973=CARTESIAN_POINT('',(0.,8.1,9.));
#43974=CARTESIAN_POINT('Origin',(0.,11.,0.));
#43975=CARTESIAN_POINT('Origin',(0.,8.1,9.));
#43976=CARTESIAN_POINT('',(0.,-11.,9.));
#43977=CARTESIAN_POINT('',(0.,-8.1,9.));
#43978=CARTESIAN_POINT('',(54.5,-11.,9.));
#43979=CARTESIAN_POINT('',(11.5,-11.,9.));
#43980=CARTESIAN_POINT('',(54.5,11.,9.));
#43981=CARTESIAN_POINT('',(54.5,8.1,9.));
#43982=CARTESIAN_POINT('',(11.5,11.,9.));
#43983=CARTESIAN_POINT('',(0.5,3.075,9.));
#43984=CARTESIAN_POINT('Origin',(0.25,-1.95,8.75));
#43985=CARTESIAN_POINT('Ctrl Pts',(53.3994258036423,-11.9970763379733,-6.20150705299425));
#43986=CARTESIAN_POINT('Ctrl Pts',(53.3983950128377,-11.9971576476841,-6.20052513988951));
#43987=CARTESIAN_POINT('Ctrl Pts',(53.3943370172609,-11.9975342948482,-6.19665654944087));
#43988=CARTESIAN_POINT('Ctrl Pts',(53.3727107131384,-11.9989014878572,-6.1758928909015));
#43989=CARTESIAN_POINT('Ctrl Pts',(53.3526536192614,-11.99969335768,-6.15650865342772));
#43990=CARTESIAN_POINT('Ctrl Pts',(53.3311081853195,-12.0000565840971,-6.13563358306537));
#43991=CARTESIAN_POINT('Ctrl Pts',(53.3270617506464,-12.,-6.1317145494215));
#43992=CARTESIAN_POINT('Ctrl Pts',(53.3260375416529,-12.,-6.13072210034901));
#43993=CARTESIAN_POINT('Ctrl Pts',(53.6250878309457,-11.9970763379733,-5.95707109672624));
#43994=CARTESIAN_POINT('Ctrl Pts',(53.624046974867,-11.9971576476841,-5.95610008627501));
#43995=CARTESIAN_POINT('Ctrl Pts',(53.6199123835538,-11.9975342948482,-5.95231446393721));
#43996=CARTESIAN_POINT('Ctrl Pts',(53.5980500288147,-11.9989014878572,-5.9318064942209));
#43997=CARTESIAN_POINT('Ctrl Pts',(53.5776596596804,-11.99969335768,-5.91278325880497));
#43998=CARTESIAN_POINT('Ctrl Pts',(53.5558687126325,-12.0000565840971,-5.89217412698611));
#43999=CARTESIAN_POINT('Ctrl Pts',(53.5517314884884,-12.,-5.88835343603374));
#44000=CARTESIAN_POINT('Ctrl Pts',(53.5506916944353,-12.,-5.88737786861835));
#44001=CARTESIAN_POINT('Ctrl Pts',(53.8507498582491,-11.9970763379733,-5.71263514045823));
#44002=CARTESIAN_POINT('Ctrl Pts',(53.8496989368963,-11.9971576476841,-5.71167503266051));
#44003=CARTESIAN_POINT('Ctrl Pts',(53.8455849036831,-11.9980545985291,-5.7078554941638));
#44004=CARTESIAN_POINT('Ctrl Pts',(53.8231265400383,-11.9984560506594,-5.68769817753873));
#44005=CARTESIAN_POINT('Ctrl Pts',(53.8026126104705,-12.0001633022127,-5.66888975818738));
#44006=CARTESIAN_POINT('Ctrl Pts',(53.7804492566119,-11.9995402969754,-5.64881168903421));
#44007=CARTESIAN_POINT('Ctrl Pts',(53.7764012263304,-12.,-5.64499232264598));
#44008=CARTESIAN_POINT('Ctrl Pts',(53.7753458472176,-12.,-5.64403363688769));
#44009=CARTESIAN_POINT('Ctrl Pts',(54.0764118855525,-11.9970763379733,-5.46819918419022));
#44010=CARTESIAN_POINT('Ctrl Pts',(54.0753508989257,-11.9971576476841,-5.46724997904601));
#44011=CARTESIAN_POINT('Ctrl Pts',(54.0711710231008,-11.9975342948482,-5.46351340866015));
#44012=CARTESIAN_POINT('Ctrl Pts',(54.048748896601,-11.9989014878572,-5.44361178085813));
#44013=CARTESIAN_POINT('Ctrl Pts',(54.0278269351149,-11.99969335768,-5.42516436356463));
#44014=CARTESIAN_POINT('Ctrl Pts',(54.0053002006183,-12.0000565840971,-5.40535223295494));
#44015=CARTESIAN_POINT('Ctrl Pts',(54.0010709641725,-12.,-5.40163120925822));
#44016=CARTESIAN_POINT('Ctrl Pts',(54.,-12.,-5.40068940515703));
#44017=CARTESIAN_POINT('',(53.3260375416529,-12.,-6.13072210034901));
#44018=CARTESIAN_POINT('',(53.3994258036423,-11.9970763379733,-6.20150705299425));
#44019=CARTESIAN_POINT('Ctrl Pts',(53.3260375416529,-12.,-6.13072210034901));
#44020=CARTESIAN_POINT('Ctrl Pts',(53.3263653917992,-12.,-6.13103978411836));
#44021=CARTESIAN_POINT('Ctrl Pts',(53.3266965241738,-11.9999998537887,-6.13136064571203));
#44022=CARTESIAN_POINT('Ctrl Pts',(53.3271049857568,-11.9999993771298,-6.1317563979681));
#44023=CARTESIAN_POINT('Ctrl Pts',(53.3275337985376,-11.9999988767218,-6.13217186819225));
#44024=CARTESIAN_POINT('Ctrl Pts',(53.3280476274129,-11.9999980172876,-6.1326696741755));
#44025=CARTESIAN_POINT('Ctrl Pts',(53.3286904259905,-11.9999961533972,-6.13329239134349));
#44026=CARTESIAN_POINT('Ctrl Pts',(53.3293756063502,-11.9999941666144,-6.13395616626162));
#44027=CARTESIAN_POINT('Ctrl Pts',(53.3302070341195,-11.9999910328059,-6.13476158745548));
#44028=CARTESIAN_POINT('Ctrl Pts',(53.3311954446607,-11.9999854611243,-6.13571905555109));
#44029=CARTESIAN_POINT('Ctrl Pts',(53.3322884658049,-11.9999792997515,-6.13677785938784));
#44030=CARTESIAN_POINT('Ctrl Pts',(53.3335730356946,-11.9999701116392,-6.13802219121803));
#44031=CARTESIAN_POINT('Ctrl Pts',(53.3350185362129,-11.9999559246679,-6.13942237194384));
#44032=CARTESIAN_POINT('Ctrl Pts',(53.3368471635251,-11.9999379774705,-6.14119366755035));
#44033=CARTESIAN_POINT('Ctrl Pts',(53.3389323869447,-11.9999118325716,-6.14321346237318));
#44034=CARTESIAN_POINT('Ctrl Pts',(53.3411513308822,-11.9998751862731,-6.14536258368008));
#44035=CARTESIAN_POINT('Ctrl Pts',(53.3434411556436,-11.9998373693639,-6.14758035543208));
#44036=CARTESIAN_POINT('Ctrl Pts',(53.345868635647,-11.9997883276492,-6.14993125395063));
#44037=CARTESIAN_POINT('Ctrl Pts',(53.3482907512442,-11.9997294435353,-6.15227641841813));
#44038=CARTESIAN_POINT('Ctrl Pts',(53.3501500681357,-11.9996842416351,-6.15407666441501));
#44039=CARTESIAN_POINT('Ctrl Pts',(53.352005417499,-11.9996333964815,-6.1558727486431));
#44040=CARTESIAN_POINT('Ctrl Pts',(53.3538165595412,-11.9995784557113,-6.15762546358553));
#44041=CARTESIAN_POINT('Ctrl Pts',(53.3554526522043,-11.9995288250425,-6.15920877620872));
#44042=CARTESIAN_POINT('Ctrl Pts',(53.3570522619671,-11.9994759318124,-6.16075630398688));
#44043=CARTESIAN_POINT('Ctrl Pts',(53.3586155616919,-11.9994203574747,-6.16226796467035));
#44044=CARTESIAN_POINT('Ctrl Pts',(53.3601422105451,-11.9993660860529,-6.16374418513686));
#44045=CARTESIAN_POINT('Ctrl Pts',(53.3616336692583,-11.9993093376916,-6.16518565842691));
#44046=CARTESIAN_POINT('Ctrl Pts',(53.3631274578893,-11.9992489493601,-6.16662838182109));
#44047=CARTESIAN_POINT('Ctrl Pts',(53.3646060851576,-11.9991891739463,-6.16805646214439));
#44048=CARTESIAN_POINT('Ctrl Pts',(53.3660934825782,-11.9991255575139,-6.16949201650793));
#44049=CARTESIAN_POINT('Ctrl Pts',(53.367618365977,-11.9990565477853,-6.17096264966601));
#44050=CARTESIAN_POINT('Ctrl Pts',(53.3692606175906,-11.9989822264713,-6.17254647547123));
#44051=CARTESIAN_POINT('Ctrl Pts',(53.3709459816506,-11.9989015996314,-6.17417063363568));
#44052=CARTESIAN_POINT('Ctrl Pts',(53.3726668563583,-11.9988143988634,-6.17582784143697));
#44053=CARTESIAN_POINT('Ctrl Pts',(53.3746429322081,-11.9987142664533,-6.17773080874758));
#44054=CARTESIAN_POINT('Ctrl Pts',(53.3766652694672,-11.9986053804691,-6.1796768086172));
#44055=CARTESIAN_POINT('Ctrl Pts',(53.378673640783,-11.9984906809933,-6.18160807869434));
#44056=CARTESIAN_POINT('Ctrl Pts',(53.381387426409,-11.9983356948179,-6.18421768227407));
#44057=CARTESIAN_POINT('Ctrl Pts',(53.3840724615807,-11.998169946725,-6.18679724506432));
#44058=CARTESIAN_POINT('Ctrl Pts',(53.3865204335424,-11.9980095903933,-6.18914727674629));
#44059=CARTESIAN_POINT('Ctrl Pts',(53.3883564125136,-11.9978893231445,-6.19090980050777));
#44060=CARTESIAN_POINT('Ctrl Pts',(53.390056605587,-11.9977724646069,-6.19254088692898));
#44061=CARTESIAN_POINT('Ctrl Pts',(53.3915493621279,-11.9976666880185,-6.19397211154302));
#44062=CARTESIAN_POINT('Ctrl Pts',(53.3928168047706,-11.9975768771518,-6.19518730977343));
#44063=CARTESIAN_POINT('Ctrl Pts',(53.3939342984045,-11.9974951565352,-6.19625804170453));
#44064=CARTESIAN_POINT('Ctrl Pts',(53.3948846855004,-11.9974244749302,-6.19716807146619));
#44065=CARTESIAN_POINT('Ctrl Pts',(53.3957785612314,-11.9973579961538,-6.19802398956728));
#44066=CARTESIAN_POINT('Ctrl Pts',(53.3965241938291,-11.9973013412632,-6.19873734940401));
#44067=CARTESIAN_POINT('Ctrl Pts',(53.397138735667,-11.9972542202014,-6.19932477155095));
#44068=CARTESIAN_POINT('Ctrl Pts',(53.3977120757812,-11.9972102583533,-6.1998728102035));
#44069=CARTESIAN_POINT('Ctrl Pts',(53.3981711596242,-11.9971746073626,-6.20031108454769));
#44070=CARTESIAN_POINT('Ctrl Pts',(53.3985618556972,-11.9971441165173,-6.20068369529959));
#44071=CARTESIAN_POINT('Ctrl Pts',(53.3988803378796,-11.9971192614149,-6.20098743494198));
#44072=CARTESIAN_POINT('Ctrl Pts',(53.3991538396393,-11.9970977907398,-6.20124798489108));
#44073=CARTESIAN_POINT('Ctrl Pts',(53.3994258036423,-11.9970763379733,-6.20150705299425));
#44074=CARTESIAN_POINT('',(54.0764118855525,-11.9970763379733,-5.46819918419022));
#44075=CARTESIAN_POINT('Ctrl Pts',(54.0764118855525,-11.9970763379733,-5.46819918419022));
#44076=CARTESIAN_POINT('Ctrl Pts',(53.8507498582491,-11.9970763379733,-5.71263514045823));
#44077=CARTESIAN_POINT('Ctrl Pts',(53.6250878309457,-11.9970763379733,-5.95707109672624));
#44078=CARTESIAN_POINT('Ctrl Pts',(53.3994258036423,-11.9970763379733,-6.20150705299425));
#44079=CARTESIAN_POINT('',(54.,-12.,-5.40068940515703));
#44080=CARTESIAN_POINT('Ctrl Pts',(54.0764118855525,-11.9970763379733,-5.46819918419022));
#44081=CARTESIAN_POINT('Ctrl Pts',(54.0760722127604,-11.9971023691181,-5.46789529802103));
#44082=CARTESIAN_POINT('Ctrl Pts',(54.0757291197379,-11.9971285176846,-5.46758838194082));
#44083=CARTESIAN_POINT('Ctrl Pts',(54.0753056420862,-11.9971604987513,-5.46721012598462));
#44084=CARTESIAN_POINT('Ctrl Pts',(54.0748610599743,-11.9971940736286,-5.46681301923949));
#44085=CARTESIAN_POINT('Ctrl Pts',(54.0743281004805,-11.9972340652564,-5.46633747933918));
#44086=CARTESIAN_POINT('Ctrl Pts',(54.0736610164599,-11.9972833371987,-5.46574298228709));
#44087=CARTESIAN_POINT('Ctrl Pts',(54.0729499354457,-11.9973358588325,-5.46510927565687));
#44088=CARTESIAN_POINT('Ctrl Pts',(54.0720867541943,-11.9973988966663,-5.46434067032571));
#44089=CARTESIAN_POINT('Ctrl Pts',(54.0710601807953,-11.9974720300366,-5.46342731950875));
#44090=CARTESIAN_POINT('Ctrl Pts',(54.0699248858634,-11.9975529087587,-5.46241723824755));
#44091=CARTESIAN_POINT('Ctrl Pts',(54.0685901907654,-11.997646056145,-5.46123051783103));
#44092=CARTESIAN_POINT('Ctrl Pts',(54.0670877245001,-11.9977470807882,-5.45989552018864));
#44093=CARTESIAN_POINT('Ctrl Pts',(54.0651863733471,-11.9978749261358,-5.45820609835923));
#44094=CARTESIAN_POINT('Ctrl Pts',(54.0630173124452,-11.9980151152307,-5.4562800918209));
#44095=CARTESIAN_POINT('Ctrl Pts',(54.0607081627339,-11.9981555585065,-5.45423127183505));
#44096=CARTESIAN_POINT('Ctrl Pts',(54.0583277577051,-11.9983003355552,-5.45211922973853));
#44097=CARTESIAN_POINT('Ctrl Pts',(54.0558034072171,-11.9984449647778,-5.44988105183916));
#44098=CARTESIAN_POINT('Ctrl Pts',(54.0532835128464,-11.9985794246122,-5.44764872916434));
#44099=CARTESIAN_POINT('Ctrl Pts',(54.0513482481033,-11.9986826890108,-5.44593431787072));
#44100=CARTESIAN_POINT('Ctrl Pts',(54.0494164611994,-11.9987800458046,-5.44422410507438));
#44101=CARTESIAN_POINT('Ctrl Pts',(54.0475300683954,-11.9988698076318,-5.44255532992866));
#44102=CARTESIAN_POINT('Ctrl Pts',(54.0458259206903,-11.9989508975359,-5.4410477757603));
#44103=CARTESIAN_POINT('Ctrl Pts',(54.0441592479608,-11.9990258356104,-5.4395744161984));
#44104=CARTESIAN_POINT('Ctrl Pts',(54.0425299575421,-11.999095192017,-5.43813518392925));
#44105=CARTESIAN_POINT('Ctrl Pts',(54.0409373737401,-11.9991629858789,-5.43672837641793));
#44106=CARTESIAN_POINT('Ctrl Pts',(54.039381101088,-11.9992254815385,-5.43535470102763));
#44107=CARTESIAN_POINT('Ctrl Pts',(54.0378220639733,-11.9992844897609,-5.43397951691513));
#44108=CARTESIAN_POINT('Ctrl Pts',(54.0362803384762,-11.9993428427535,-5.43261960290821));
#44109=CARTESIAN_POINT('Ctrl Pts',(54.0347291700889,-11.9993980271028,-5.43125225130619));
#44110=CARTESIAN_POINT('Ctrl Pts',(54.03313887087,-11.9994507567847,-5.42985104760384));
#44111=CARTESIAN_POINT('Ctrl Pts',(54.0314260532856,-11.9995075488181,-5.42834189365842));
#44112=CARTESIAN_POINT('Ctrl Pts',(54.0296682220344,-11.9995614139067,-5.42679380614295));
#44113=CARTESIAN_POINT('Ctrl Pts',(54.0278734893913,-11.9996114588124,-5.42521367241687));
#44114=CARTESIAN_POINT('Ctrl Pts',(54.0258122123109,-11.9996689361296,-5.42339886537801));
#44115=CARTESIAN_POINT('Ctrl Pts',(54.0237028433572,-11.9997212431699,-5.42154230191065));
#44116=CARTESIAN_POINT('Ctrl Pts',(54.0216083794328,-11.9997665117108,-5.41969914921859));
#44117=CARTESIAN_POINT('Ctrl Pts',(54.0187800293293,-11.9998276420462,-5.41721016812596));
#44118=CARTESIAN_POINT('Ctrl Pts',(54.0159822587379,-11.9998755281407,-5.41474862664469));
#44119=CARTESIAN_POINT('Ctrl Pts',(54.0134321223697,-11.9999097849749,-5.41250509703313));
#44120=CARTESIAN_POINT('Ctrl Pts',(54.0115195200935,-11.9999354776006,-5.41082244982447));
#44121=CARTESIAN_POINT('Ctrl Pts',(54.0097487440424,-11.9999536880558,-5.40926466739841));
#44122=CARTESIAN_POINT('Ctrl Pts',(54.0081943616607,-11.9999664256549,-5.40789727780843));
#44123=CARTESIAN_POINT('Ctrl Pts',(54.0068744527208,-11.9999772418292,-5.406736154416));
#44124=CARTESIAN_POINT('Ctrl Pts',(54.0057109990572,-11.9999841813838,-5.40571268935998));
#44125=CARTESIAN_POINT('Ctrl Pts',(54.0047218043466,-11.9999888522197,-5.40484253492563));
#44126=CARTESIAN_POINT('Ctrl Pts',(54.0037913926568,-11.9999932454907,-5.4040240895286));
#44127=CARTESIAN_POINT('Ctrl Pts',(54.0030155797099,-11.9999956573955,-5.40334165912276));
#44128=CARTESIAN_POINT('Ctrl Pts',(54.002376417312,-11.9999971763164,-5.40277945700749));
#44129=CARTESIAN_POINT('Ctrl Pts',(54.0017800846694,-11.9999985934556,-5.40225492760136));
#44130=CARTESIAN_POINT('Ctrl Pts',(54.0013028624762,-11.999999233682,-5.40183519503762));
#44131=CARTESIAN_POINT('Ctrl Pts',(54.0008968882916,-11.9999995977956,-5.40147815247162));
#44132=CARTESIAN_POINT('Ctrl Pts',(54.0005662011516,-11.9999998943852,-5.40118732268617));
#44133=CARTESIAN_POINT('Ctrl Pts',(54.0002823024135,-12.,-5.40093766142703));
#44134=CARTESIAN_POINT('Ctrl Pts',(54.,-12.,-5.40068940515703));
#44135=CARTESIAN_POINT('',(53.6630187708265,-12.,-5.76570575275302));
#44136=CARTESIAN_POINT('Ctrl Pts',(54.0764118855525,-11.9970763379733,-5.46819918419022));
#44137=CARTESIAN_POINT('Ctrl Pts',(54.3504972331451,-11.9760715488571,-5.71340795054702));
#44138=CARTESIAN_POINT('Ctrl Pts',(54.7498941157113,-11.7487468298691,-6.13435950914876));
#44139=CARTESIAN_POINT('Ctrl Pts',(54.9796857837848,-11.2917992749461,-6.46017864830904));
#44140=CARTESIAN_POINT('Ctrl Pts',(55.,-11.0939065095575,-6.5));
#44141=CARTESIAN_POINT('Ctrl Pts',(55.,-11.,-6.5));
#44142=CARTESIAN_POINT('Ctrl Pts',(53.8507498582491,-11.9970763379733,-5.71263514045823));
#44143=CARTESIAN_POINT('Ctrl Pts',(54.122235037212,-11.9760715488571,-5.96066039620419));
#44144=CARTESIAN_POINT('Ctrl Pts',(54.5389866050285,-11.748746829869,-6.36281344831557));
#44145=CARTESIAN_POINT('Ctrl Pts',(54.8065498116121,-11.2917992749461,-6.64771864973562));
#44146=CARTESIAN_POINT('Ctrl Pts',(54.833864120244,-11.0939065095575,-6.67995753704715));
#44147=CARTESIAN_POINT('Ctrl Pts',(54.833864120244,-11.,-6.67995753704715));
#44148=CARTESIAN_POINT('Ctrl Pts',(53.6250878309457,-11.9970763379733,-5.95707109672624));
#44149=CARTESIAN_POINT('Ctrl Pts',(53.893972841279,-11.9760715488571,-6.20791284186136));
#44150=CARTESIAN_POINT('Ctrl Pts',(54.3280790943458,-11.748746829869,-6.59126738748238));
#44151=CARTESIAN_POINT('Ctrl Pts',(54.6334138394395,-11.2917992749461,-6.83525865116221));
#44152=CARTESIAN_POINT('Ctrl Pts',(54.667728240488,-11.0939065095575,-6.8599150740943));
#44153=CARTESIAN_POINT('Ctrl Pts',(54.667728240488,-11.,-6.8599150740943));
#44154=CARTESIAN_POINT('Ctrl Pts',(53.3994258036423,-11.9970763379733,-6.20150705299425));
#44155=CARTESIAN_POINT('Ctrl Pts',(53.665710645346,-11.9760715488571,-6.45516528751854));
#44156=CARTESIAN_POINT('Ctrl Pts',(54.1171715836631,-11.748746829869,-6.81972132664919));
#44157=CARTESIAN_POINT('Ctrl Pts',(54.4602778672668,-11.2917992749461,-7.0227986525888));
#44158=CARTESIAN_POINT('Ctrl Pts',(54.5015923607319,-11.0939065095575,-7.03987261114145));
#44159=CARTESIAN_POINT('Ctrl Pts',(54.5015923607319,-11.,-7.03987261114145));
#44160=CARTESIAN_POINT('',(54.5015923607319,-11.,-7.03987261114145));
#44161=CARTESIAN_POINT('Ctrl Pts',(53.3994258036423,-11.9970763379733,-6.20150705299425));
#44162=CARTESIAN_POINT('Ctrl Pts',(53.665710645346,-11.9760715488571,-6.45516528751854));
#44163=CARTESIAN_POINT('Ctrl Pts',(54.1171715836631,-11.748746829869,-6.81972132664919));
#44164=CARTESIAN_POINT('Ctrl Pts',(54.4602778672668,-11.2917992749461,-7.0227986525888));
#44165=CARTESIAN_POINT('Ctrl Pts',(54.5015923607319,-11.0939065095575,-7.03987261114145));
#44166=CARTESIAN_POINT('Ctrl Pts',(54.5015923607319,-11.,-7.03987261114145));
#44167=CARTESIAN_POINT('',(55.,-11.,-6.5));
#44168=CARTESIAN_POINT('',(54.5015923607319,-11.,-7.03987261114145));
#44169=CARTESIAN_POINT('Ctrl Pts',(55.,-11.,-6.5));
#44170=CARTESIAN_POINT('Ctrl Pts',(55.,-11.0939065095575,-6.5));
#44171=CARTESIAN_POINT('Ctrl Pts',(54.9796857837848,-11.2917992749461,-6.46017864830904));
#44172=CARTESIAN_POINT('Ctrl Pts',(54.7498941157113,-11.7487468298691,-6.13435950914876));
#44173=CARTESIAN_POINT('Ctrl Pts',(54.3504972331451,-11.9760715488571,-5.71340795054702));
#44174=CARTESIAN_POINT('Ctrl Pts',(54.0764118855525,-11.9970763379733,-5.46819918419022));
#44175=CARTESIAN_POINT('Origin',(54.750796180366,0.,-6.76993630557072));
#44176=CARTESIAN_POINT('',(54.5384025518406,-3.87298334620742,-7.));
#44177=CARTESIAN_POINT('',(54.5384025518406,-6.,-7.));
#44178=CARTESIAN_POINT('',(55.,-4.66368952654441,-6.5));
#44179=CARTESIAN_POINT('Origin',(61.0007668260719,0.,0.));
#44180=CARTESIAN_POINT('',(55.,0.,-6.5));
#44181=CARTESIAN_POINT('',(54.5015923607319,0.,-7.03987261114144));
#44182=CARTESIAN_POINT('Origin',(23.,-12.,0.));
#44183=CARTESIAN_POINT('',(54.,-12.,7.29826682694392));
#44184=CARTESIAN_POINT('',(54.,-12.,4.5));
#44185=CARTESIAN_POINT('',(53.2982668269439,-12.,8.));
#44186=CARTESIAN_POINT('',(53.649133413472,-12.,7.64913341347196));
#44187=CARTESIAN_POINT('',(0.,-12.,8.));
#44188=CARTESIAN_POINT('',(11.5,-12.,8.));
#44189=CARTESIAN_POINT('',(0.,-12.,-8.));
#44190=CARTESIAN_POINT('Origin',(0.,-12.,0.));
#44191=CARTESIAN_POINT('',(29.9600637960156,-12.,-8.));
#44192=CARTESIAN_POINT('',(11.5,-12.,-8.));
#44193=CARTESIAN_POINT('',(26.8002229812147,-12.,-8.25278726518407));
#44194=CARTESIAN_POINT('',(12.95,-12.,-2.));
#44195=CARTESIAN_POINT('Origin',(16.,-12.,-2.));
#44196=CARTESIAN_POINT('',(-3.05,-12.,3.73517273739943E-16));
#44197=CARTESIAN_POINT('Origin',(0.,-12.,0.));
#44198=CARTESIAN_POINT('Origin',(54.,-11.,4.5));
#44199=CARTESIAN_POINT('',(55.,-11.,8.5));
#44200=CARTESIAN_POINT('',(55.,-11.,4.5));
#44201=CARTESIAN_POINT('',(54.0739345923054,-11.9972630926995,7.36867780326845));
#44202=CARTESIAN_POINT('Ctrl Pts',(54.0739345923054,-11.9972630926995,7.36867780326845));
#44203=CARTESIAN_POINT('Ctrl Pts',(54.3510337690789,-11.9767196525453,7.63593113286991));
#44204=CARTESIAN_POINT('Ctrl Pts',(54.7553166986942,-11.7446620906573,8.09873418111303));
#44205=CARTESIAN_POINT('Ctrl Pts',(54.9514928044654,-11.3451725484552,8.40875696033662));
#44206=CARTESIAN_POINT('Ctrl Pts',(54.9944234105006,-11.1325383755072,8.488654852558));
#44207=CARTESIAN_POINT('Ctrl Pts',(55.,-11.0439996496616,8.5));
#44208=CARTESIAN_POINT('Ctrl Pts',(55.,-11.,8.5));
#44209=CARTESIAN_POINT('Ctrl Pts',(54.,-12.,7.29826682694392));
#44210=CARTESIAN_POINT('Ctrl Pts',(54.0003314977971,-12.,7.29858113228725));
#44211=CARTESIAN_POINT('Ctrl Pts',(54.0006663098912,-11.9999998632791,7.29889858217632));
#44212=CARTESIAN_POINT('Ctrl Pts',(54.0010792590121,-11.9999994175998,7.29929014342446));
#44213=CARTESIAN_POINT('Ctrl Pts',(54.0015127758868,-11.9999989497226,7.29970120716084));
#44214=CARTESIAN_POINT('Ctrl Pts',(54.0020321949842,-11.9999981461834,7.30019374676313));
#44215=CARTESIAN_POINT('Ctrl Pts',(54.0026819516524,-11.9999964035612,7.30080989895442));
#44216=CARTESIAN_POINT('Ctrl Pts',(54.0033745293584,-11.9999945460946,7.30146665754134));
#44217=CARTESIAN_POINT('Ctrl Pts',(54.0042148986562,-11.9999916163369,7.3022635810719));
#44218=CARTESIAN_POINT('Ctrl Pts',(54.0052139420484,-11.9999864073118,7.30321098451133));
#44219=CARTESIAN_POINT('Ctrl Pts',(54.0063186100511,-11.9999806475585,7.30425855288863));
#44220=CARTESIAN_POINT('Ctrl Pts',(54.0076168538779,-11.9999720586087,7.30548969855211));
#44221=CARTESIAN_POINT('Ctrl Pts',(54.0090777731715,-11.9999587961682,7.30687513396345));
#44222=CARTESIAN_POINT('Ctrl Pts',(54.0109250805974,-11.9999420260395,7.30862699331299));
#44223=CARTESIAN_POINT('Ctrl Pts',(54.0130315429888,-11.9999175989922,7.31062464255686));
#44224=CARTESIAN_POINT('Ctrl Pts',(54.0152731305057,-11.9998833589397,7.31275060112912));
#44225=CARTESIAN_POINT('Ctrl Pts',(54.0175900257341,-11.9998479685685,7.31494798277705));
#44226=CARTESIAN_POINT('Ctrl Pts',(54.0200464787717,-11.9998020541947,7.31727788628092));
#44227=CARTESIAN_POINT('Ctrl Pts',(54.0224971606944,-11.9997469068523,7.31960281446228));
#44228=CARTESIAN_POINT('Ctrl Pts',(54.0243769090201,-11.9997046071464,7.32138610580481));
#44229=CARTESIAN_POINT('Ctrl Pts',(54.0262524447249,-11.9996570221597,7.3231656968352));
#44230=CARTESIAN_POINT('Ctrl Pts',(54.0280827898051,-11.999605600683,7.32490295874137));
#44231=CARTESIAN_POINT('Ctrl Pts',(54.0297361262051,-11.9995591520651,7.32647221383799));
#44232=CARTESIAN_POINT('Ctrl Pts',(54.0313521786804,-11.9995096475949,7.32800653980115));
#44233=CARTESIAN_POINT('Ctrl Pts',(54.032930797643,-11.999457634203,7.32950604809328));
#44234=CARTESIAN_POINT('Ctrl Pts',(54.0344384154927,-11.9994079602032,7.33093811341151));
#44235=CARTESIAN_POINT('Ctrl Pts',(54.0359114872389,-11.9993560618632,7.33233803713807));
#44236=CARTESIAN_POINT('Ctrl Pts',(54.037384667835,-11.9993009489693,7.33373900926913));
#44237=CARTESIAN_POINT('Ctrl Pts',(54.0388731910723,-11.9992452620945,7.33515457201643));
#44238=CARTESIAN_POINT('Ctrl Pts',(54.0403683295817,-11.9991860424168,7.33657740804058));
#44239=CARTESIAN_POINT('Ctrl Pts',(54.0418997567846,-11.9991218195903,7.33803587655173));
#44240=CARTESIAN_POINT('Ctrl Pts',(54.0435473954296,-11.9990527232527,7.33960502007804));
#44241=CARTESIAN_POINT('Ctrl Pts',(54.0452366728309,-11.9989777892673,7.34121506113945));
#44242=CARTESIAN_POINT('Ctrl Pts',(54.0469610411776,-11.9988967216942,7.34285972054902));
#44243=CARTESIAN_POINT('Ctrl Pts',(54.0489358739595,-11.9988038790594,7.34474326667384));
#44244=CARTESIAN_POINT('Ctrl Pts',(54.050956174741,-11.9987029134817,7.34667169080142));
#44245=CARTESIAN_POINT('Ctrl Pts',(54.0529636122053,-11.9985964429048,7.34858912507421));
#44246=CARTESIAN_POINT('Ctrl Pts',(54.0557063045387,-11.9984509758403,7.35120884916192));
#44247=CARTESIAN_POINT('Ctrl Pts',(54.0584218496309,-11.9982950689308,7.35380508415633));
#44248=CARTESIAN_POINT('Ctrl Pts',(54.0608986078143,-11.998143957336,7.3561748403444));
#44249=CARTESIAN_POINT('Ctrl Pts',(54.0627561764518,-11.9980306236398,7.35795215748545));
#44250=CARTESIAN_POINT('Ctrl Pts',(54.0644768750634,-11.9979203495853,7.35959962417965));
#44251=CARTESIAN_POINT('Ctrl Pts',(54.0659873571994,-11.9978204591458,7.36104670175641));
#44252=CARTESIAN_POINT('Ctrl Pts',(54.0672641265468,-11.997736024482,7.36226987695943));
#44253=CARTESIAN_POINT('Ctrl Pts',(54.0683903006567,-11.9976591045265,7.36334949002639));
#44254=CARTESIAN_POINT('Ctrl Pts',(54.069348232894,-11.9975925133011,7.36426842264621));
#44255=CARTESIAN_POINT('Ctrl Pts',(54.0702488889839,-11.997529903661,7.36513241096188));
#44256=CARTESIAN_POINT('Ctrl Pts',(54.0710004010606,-11.99747648006,7.36585395496795));
#44257=CARTESIAN_POINT('Ctrl Pts',(54.0716194711387,-11.9974320284379,7.36644887928455));
#44258=CARTESIAN_POINT('Ctrl Pts',(54.0721967381906,-11.9973905784345,7.3670036310299));
#44259=CARTESIAN_POINT('Ctrl Pts',(54.0726586923053,-11.9973569415986,7.36744813846609));
#44260=CARTESIAN_POINT('Ctrl Pts',(54.0730507354953,-11.9973282258332,7.36782577118979));
#44261=CARTESIAN_POINT('Ctrl Pts',(54.0733781629767,-11.997304242938,7.36814116330667));
#44262=CARTESIAN_POINT('Ctrl Pts',(54.0736572293399,-11.9972836556963,7.36841029552303));
#44263=CARTESIAN_POINT('Ctrl Pts',(54.0739345923054,-11.9972630926995,7.36867780326845));
#44264=CARTESIAN_POINT('Origin',(55.,8.1,9.));
#44265=CARTESIAN_POINT('',(55.,-9.79717439317883E-16,8.));
#44266=CARTESIAN_POINT('Origin',(55.,0.,0.));
#44267=CARTESIAN_POINT('Origin',(55.,0.,0.));
#44268=CARTESIAN_POINT('',(55.,11.,8.5));
#44269=CARTESIAN_POINT('',(55.,11.,4.5));
#44270=CARTESIAN_POINT('',(55.,8.1,8.5));
#44271=CARTESIAN_POINT('Ctrl Pts',(54.0764118855525,11.9970763379733,-5.46819918419023));
#44272=CARTESIAN_POINT('Ctrl Pts',(54.0753508989257,11.9971576476841,-5.46724997904602));
#44273=CARTESIAN_POINT('Ctrl Pts',(54.0711710231008,11.9975342948482,-5.46351340866014));
#44274=CARTESIAN_POINT('Ctrl Pts',(54.048748896601,11.9989014878572,-5.44361178085813));
#44275=CARTESIAN_POINT('Ctrl Pts',(54.0278269351149,11.99969335768,-5.42516436356463));
#44276=CARTESIAN_POINT('Ctrl Pts',(54.0053002006183,12.0000565840971,-5.40535223295495));
#44277=CARTESIAN_POINT('Ctrl Pts',(54.0010709641725,12.,-5.40163120925821));
#44278=CARTESIAN_POINT('Ctrl Pts',(54.,12.,-5.40068940515702));
#44279=CARTESIAN_POINT('Ctrl Pts',(53.8507498582491,11.9970763379733,-5.71263514045823));
#44280=CARTESIAN_POINT('Ctrl Pts',(53.8496989368964,11.9971576476841,-5.71167503266052));
#44281=CARTESIAN_POINT('Ctrl Pts',(53.8455956568079,11.9975342948482,-5.7078554941638));
#44282=CARTESIAN_POINT('Ctrl Pts',(53.8234095809246,11.9989014878572,-5.68769817753873));
#44283=CARTESIAN_POINT('Ctrl Pts',(53.8028208946958,11.99969335768,-5.66888975818739));
#44284=CARTESIAN_POINT('Ctrl Pts',(53.7805396733053,12.0000565840971,-5.64881168903421));
#44285=CARTESIAN_POINT('Ctrl Pts',(53.7764012263304,12.,-5.64499232264597));
#44286=CARTESIAN_POINT('Ctrl Pts',(53.7753458472177,12.,-5.64403363688768));
#44287=CARTESIAN_POINT('Ctrl Pts',(53.6250878309457,11.9970763379733,-5.95707109672624));
#44288=CARTESIAN_POINT('Ctrl Pts',(53.624046974867,11.9971576476841,-5.95610008627502));
#44289=CARTESIAN_POINT('Ctrl Pts',(53.6199115260435,11.9980545985291,-5.9523037450581));
#44290=CARTESIAN_POINT('Ctrl Pts',(53.5980274576563,11.9984560506594,-5.93152435474098));
#44291=CARTESIAN_POINT('Ctrl Pts',(53.5776430500085,12.0001633022127,-5.91257563790681));
#44292=CARTESIAN_POINT('Ctrl Pts',(53.5558615023331,11.9995402969754,-5.8920839982447));
#44293=CARTESIAN_POINT('Ctrl Pts',(53.5517314884884,12.,-5.88835343603373));
#44294=CARTESIAN_POINT('Ctrl Pts',(53.5506916944353,12.,-5.88737786861835));
#44295=CARTESIAN_POINT('Ctrl Pts',(53.3994258036423,11.9970763379733,-6.20150705299425));
#44296=CARTESIAN_POINT('Ctrl Pts',(53.3983950128377,11.9971576476841,-6.20052513988952));
#44297=CARTESIAN_POINT('Ctrl Pts',(53.3943370172609,11.9975342948482,-6.19665654944088));
#44298=CARTESIAN_POINT('Ctrl Pts',(53.3727107131384,11.9989014878572,-6.17589289090149));
#44299=CARTESIAN_POINT('Ctrl Pts',(53.3526536192614,11.99969335768,-6.15650865342773));
#44300=CARTESIAN_POINT('Ctrl Pts',(53.3311081853195,12.0000565840971,-6.13563358306537));
#44301=CARTESIAN_POINT('Ctrl Pts',(53.3270617506464,12.,-6.13171454942149));
#44302=CARTESIAN_POINT('Ctrl Pts',(53.3260375416529,12.,-6.13072210034901));
#44303=CARTESIAN_POINT('',(54.,12.,-5.40068940515702));
#44304=CARTESIAN_POINT('',(54.0764118855525,11.9970763379733,-5.46819918419023));
#44305=CARTESIAN_POINT('Ctrl Pts',(54.,12.,-5.40068940515702));
#44306=CARTESIAN_POINT('Ctrl Pts',(54.0003428165178,12.,-5.40099087742915));
#44307=CARTESIAN_POINT('Ctrl Pts',(54.0006890624815,11.9999998537887,-5.40129536806019));
#44308=CARTESIAN_POINT('Ctrl Pts',(54.0011161272366,11.9999993771298,-5.40167096945517));
#44309=CARTESIAN_POINT('Ctrl Pts',(54.0015644700743,11.9999988767218,-5.40206528482136));
#44310=CARTESIAN_POINT('Ctrl Pts',(54.0021016660821,11.9999980172876,-5.40253777964602));
#44311=CARTESIAN_POINT('Ctrl Pts',(54.0027736601848,11.9999961533972,-5.4031288723702));
#44312=CARTESIAN_POINT('Ctrl Pts',(54.0034899610248,11.9999941666144,-5.40375893774298));
#44313=CARTESIAN_POINT('Ctrl Pts',(54.0043591195687,11.9999910328059,-5.40452348915422));
#44314=CARTESIAN_POINT('Ctrl Pts',(54.0053923594135,11.9999854611243,-5.40543239837707));
#44315=CARTESIAN_POINT('Ctrl Pts',(54.006534954469,11.9999792997515,-5.40643750400599));
#44316=CARTESIAN_POINT('Ctrl Pts',(54.0078777617603,11.9999701116392,-5.40761875337999));
#44317=CARTESIAN_POINT('Ctrl Pts',(54.0093887550606,11.9999559246679,-5.40894799265849));
#44318=CARTESIAN_POINT('Ctrl Pts',(54.0113002338754,11.9999379774705,-5.41062954394014));
#44319=CARTESIAN_POINT('Ctrl Pts',(54.0134798828194,11.9999118325716,-5.41254705751686));
#44320=CARTESIAN_POINT('Ctrl Pts',(54.015799109951,11.9998751862731,-5.41458755257959));
#44321=CARTESIAN_POINT('Ctrl Pts',(54.0181924213024,11.9998373693639,-5.41669322818569));
#44322=CARTESIAN_POINT('Ctrl Pts',(54.0207294127965,11.9997883276492,-5.41892550441653));
#44323=CARTESIAN_POINT('Ctrl Pts',(54.0232602607152,11.9997294435353,-5.42115289058855));
#44324=CARTESIAN_POINT('Ctrl Pts',(54.0252030450688,11.9996842416351,-5.42286272505649));
#44325=CARTESIAN_POINT('Ctrl Pts',(54.0271413645163,11.9996333964815,-5.42456893651285));
#44326=CARTESIAN_POINT('Ctrl Pts',(54.0290329274746,11.9995784557113,-5.42623453992945));
#44327=CARTESIAN_POINT('Ctrl Pts',(54.0307416682612,11.9995288250425,-5.42773916047606));
#44328=CARTESIAN_POINT('Ctrl Pts',(54.0324118288305,11.9994759318124,-5.42921026798065));
#44329=CARTESIAN_POINT('Ctrl Pts',(54.0340433409798,11.9994203574747,-5.43064804131396));
#44330=CARTESIAN_POINT('Ctrl Pts',(54.0356366030475,11.9993660860529,-5.43205210668668));
#44331=CARTESIAN_POINT('Ctrl Pts',(54.0371924223533,11.9993093376916,-5.4334238649114));
#44332=CARTESIAN_POINT('Ctrl Pts',(54.0387496735818,11.9992489493601,-5.43479784594404));
#44333=CARTESIAN_POINT('Ctrl Pts',(54.0402911193272,11.9991891739463,-5.43615788161346));
#44334=CARTESIAN_POINT('Ctrl Pts',(54.0418407146879,11.9991255575138,-5.43752606348578));
#44335=CARTESIAN_POINT('Ctrl Pts',(54.0434282664545,11.9990565477853,-5.43892881458755));
#44336=CARTESIAN_POINT('Ctrl Pts',(54.0451380099357,11.9989822264713,-5.44043953354628));
#44337=CARTESIAN_POINT('Ctrl Pts',(54.0468913953403,11.9989015996314,-5.44199001133725));
#44338=CARTESIAN_POINT('Ctrl Pts',(54.0486805569323,11.9988143988633,-5.44357325113376));
#44339=CARTESIAN_POINT('Ctrl Pts',(54.05073504643,11.9987142664533,-5.44539128118125));
#44340=CARTESIAN_POINT('Ctrl Pts',(54.0528361205663,11.9986053804691,-5.44725199366727));
#44341=CARTESIAN_POINT('Ctrl Pts',(54.0549213981032,11.9984906809933,-5.44909995931825));
#44342=CARTESIAN_POINT('Ctrl Pts',(54.0577391022603,11.9983356948179,-5.45159699887533));
#44343=CARTESIAN_POINT('Ctrl Pts',(54.0605245685882,11.998169946725,-5.45406777514985));
#44344=CARTESIAN_POINT('Ctrl Pts',(54.0630623301421,11.9980095903933,-5.45632054720379));
#44345=CARTESIAN_POINT('Ctrl Pts',(54.0649656513074,11.9978893231445,-5.45801012624424));
#44346=CARTESIAN_POINT('Ctrl Pts',(54.0667271254473,11.9977724646069,-5.45957483332706));
#44347=CARTESIAN_POINT('Ctrl Pts',(54.0682728322117,11.9976666880185,-5.4609487025292));
#44348=CARTESIAN_POINT('Ctrl Pts',(54.0695852328695,11.9975768771518,-5.46211520246701));
#44349=CARTESIAN_POINT('Ctrl Pts',(54.0707416695959,11.9974951565352,-5.46314375143915));
#44350=CARTESIAN_POINT('Ctrl Pts',(54.0717245899964,11.9974244749302,-5.46401854129122));
#44351=CARTESIAN_POINT('Ctrl Pts',(54.0726490645556,11.9973579961537,-5.46484131489773));
#44352=CARTESIAN_POINT('Ctrl Pts',(54.0734196131772,11.9973013412632,-5.46552768582455));
#44353=CARTESIAN_POINT('Ctrl Pts',(54.0740541713237,11.9972542202014,-5.46609342640823));
#44354=CARTESIAN_POINT('Ctrl Pts',(54.0746461857607,11.9972102583533,-5.46662123712968));
#44355=CARTESIAN_POINT('Ctrl Pts',(54.0751196740662,11.9971746073626,-5.46704390863355));
#44356=CARTESIAN_POINT('Ctrl Pts',(54.0755222543019,11.9971441165173,-5.46740364652107));
#44357=CARTESIAN_POINT('Ctrl Pts',(54.0758504240505,11.9971192614149,-5.46769689264119));
#44358=CARTESIAN_POINT('Ctrl Pts',(54.0761319546792,11.9970977907398,-5.46794874576034));
#44359=CARTESIAN_POINT('Ctrl Pts',(54.0764118855525,11.9970763379733,-5.46819918419023));
#44360=CARTESIAN_POINT('',(53.3994258036423,11.9970763379733,-6.20150705299425));
#44361=CARTESIAN_POINT('Ctrl Pts',(53.3994258036423,11.9970763379733,-6.20150705299425));
#44362=CARTESIAN_POINT('Ctrl Pts',(53.6250878309457,11.9970763379733,-5.95707109672624));
#44363=CARTESIAN_POINT('Ctrl Pts',(53.8507498582491,11.9970763379733,-5.71263514045823));
#44364=CARTESIAN_POINT('Ctrl Pts',(54.0764118855525,11.9970763379733,-5.46819918419023));
#44365=CARTESIAN_POINT('',(53.3260375416529,12.,-6.13072210034901));
#44366=CARTESIAN_POINT('Ctrl Pts',(53.3994258036423,11.9970763379733,-6.20150705299425));
#44367=CARTESIAN_POINT('Ctrl Pts',(53.3990957979836,11.9971023691181,-6.20119269543551));
#44368=CARTESIAN_POINT('Ctrl Pts',(53.3987624993162,11.9971285176846,-6.20087517015968));
#44369=CARTESIAN_POINT('Ctrl Pts',(53.3983516776804,11.9971604987513,-6.20048320527172));
#44370=CARTESIAN_POINT('Ctrl Pts',(53.3979203823103,11.9971940736286,-6.2000717063956));
#44371=CARTESIAN_POINT('Ctrl Pts',(53.3974038558988,11.9972340652564,-6.19957836626438));
#44372=CARTESIAN_POINT('Ctrl Pts',(53.3967580553908,11.9972833371987,-6.19896081502021));
#44373=CARTESIAN_POINT('Ctrl Pts',(53.3960696616261,11.9973358588325,-6.19830253367709));
#44374=CARTESIAN_POINT('Ctrl Pts',(53.3952346695081,11.9973988966663,-6.19750339402051));
#44375=CARTESIAN_POINT('Ctrl Pts',(53.3942423631352,11.9974720300366,-6.19655292533578));
#44376=CARTESIAN_POINT('Ctrl Pts',(53.3931449643548,11.9975529087587,-6.19550179515672));
#44377=CARTESIAN_POINT('Ctrl Pts',(53.391855587755,11.997646056145,-6.19426598597423));
#44378=CARTESIAN_POINT('Ctrl Pts',(53.390405027202,11.9977470807882,-6.19287476432927));
#44379=CARTESIAN_POINT('Ctrl Pts',(53.3885693620402,11.9978749261358,-6.19111419176947));
#44380=CARTESIAN_POINT('Ctrl Pts',(53.3864765170525,11.9980151152307,-6.18910562854187));
#44381=CARTESIAN_POINT('Ctrl Pts',(53.3842500783306,11.9981555585065,-6.18696721643439));
#44382=CARTESIAN_POINT('Ctrl Pts',(53.3819549365717,11.9983003355552,-6.18476281759905));
#44383=CARTESIAN_POINT('Ctrl Pts',(53.3795225817548,11.9984449647777,-6.18242499045831));
#44384=CARTESIAN_POINT('Ctrl Pts',(53.3770964188692,11.9985794246121,-6.18009113831728));
#44385=CARTESIAN_POINT('Ctrl Pts',(53.3752331393809,11.9986826890108,-6.17829875296305));
#44386=CARTESIAN_POINT('Ctrl Pts',(53.3733743223599,11.9987800458046,-6.17650949956189));
#44387=CARTESIAN_POINT('Ctrl Pts',(53.3715604309847,11.9988698076318,-6.17476219123845));
#44388=CARTESIAN_POINT('Ctrl Pts',(53.3699217803189,11.9989508975359,-6.1731836910114));
#44389=CARTESIAN_POINT('Ctrl Pts',(53.3683202038096,11.9990258356104,-6.17163981955613));
#44390=CARTESIAN_POINT('Ctrl Pts',(53.3667556269677,11.999095192017,-6.17013048987079));
#44391=CARTESIAN_POINT('Ctrl Pts',(53.3652262987972,11.9991629858789,-6.16865516418234));
#44392=CARTESIAN_POINT('Ctrl Pts',(53.3637328928719,11.9992254815385,-6.16721339187455));
#44393=CARTESIAN_POINT('Ctrl Pts',(53.3622377625765,11.9992844897609,-6.1657689842216));
#44394=CARTESIAN_POINT('Ctrl Pts',(53.3607592342745,11.9993428427535,-6.16434061533548));
#44395=CARTESIAN_POINT('Ctrl Pts',(53.3592725390386,11.9993980271028,-6.16290342674496));
#44396=CARTESIAN_POINT('Ctrl Pts',(53.3577489790151,11.9994507567847,-6.1614299314868));
#44397=CARTESIAN_POINT('Ctrl Pts',(53.3561080422857,11.9995075488181,-6.15984291656622));
#44398=CARTESIAN_POINT('Ctrl Pts',(53.3544247063539,11.9995614139066,-6.15821413610097));
#44399=CARTESIAN_POINT('Ctrl Pts',(53.3527064835601,11.9996114588124,-6.15655112729673));
#44400=CARTESIAN_POINT('Ctrl Pts',(53.3507330791772,11.9996689361296,-6.15464113700044));
#44401=CARTESIAN_POINT('Ctrl Pts',(53.3487142162513,11.9997212431699,-6.15268653786576));
#44402=CARTESIAN_POINT('Ctrl Pts',(53.346709909996,11.9997665117107,-6.15074572684662));
#44403=CARTESIAN_POINT('Ctrl Pts',(53.3440033082071,11.9998276420462,-6.14812486860091));
#44404=CARTESIAN_POINT('Ctrl Pts',(53.3413264972121,11.9998755281407,-6.14553230430206));
#44405=CARTESIAN_POINT('Ctrl Pts',(53.3388867514259,11.9999097849749,-6.14316920017543));
#44406=CARTESIAN_POINT('Ctrl Pts',(53.3370569420862,11.9999354776006,-6.14139687208045));
#44407=CARTESIAN_POINT('Ctrl Pts',(53.3353629098334,11.9999536880558,-6.1397559611636));
#44408=CARTESIAN_POINT('Ctrl Pts',(53.3338759204298,11.9999664256549,-6.13831557184363));
#44409=CARTESIAN_POINT('Ctrl Pts',(53.3326132384602,11.9999772418292,-6.13709246048908));
#44410=CARTESIAN_POINT('Ctrl Pts',(53.3315002529843,11.9999841813838,-6.13601432854974));
#44411=CARTESIAN_POINT('Ctrl Pts',(53.3305539861973,11.9999888522197,-6.1350976748075));
#44412=CARTESIAN_POINT('Ctrl Pts',(53.3296639514339,11.9999932454907,-6.13423549332984));
#44413=CARTESIAN_POINT('Ctrl Pts',(53.3289218270029,11.9999956573955,-6.13351657169551));
#44414=CARTESIAN_POINT('Ctrl Pts',(53.3283104451973,11.9999971763164,-6.13292427778441));
#44415=CARTESIAN_POINT('Ctrl Pts',(53.327740031592,11.9999985934556,-6.13237167300935));
#44416=CARTESIAN_POINT('Ctrl Pts',(53.3272835795697,11.999999233682,-6.13192944230248));
#44417=CARTESIAN_POINT('Ctrl Pts',(53.3268952995833,11.9999995977956,-6.13155323347136));
#44418=CARTESIAN_POINT('Ctrl Pts',(53.3265790252902,11.9999998943852,-6.13124679176368));
#44419=CARTESIAN_POINT('Ctrl Pts',(53.3263075195646,12.,-6.13098370645648));
#44420=CARTESIAN_POINT('Ctrl Pts',(53.3260375416529,12.,-6.13072210034901));
#44421=CARTESIAN_POINT('',(53.6630187708265,12.,-5.76570575275302));
#44422=CARTESIAN_POINT('Ctrl Pts',(53.3994258036423,11.9970763379733,-6.20150705299425));
#44423=CARTESIAN_POINT('Ctrl Pts',(53.665710645346,11.9760715488571,-6.45516528751854));
#44424=CARTESIAN_POINT('Ctrl Pts',(54.1171715836631,11.748746829869,-6.8197213266492));
#44425=CARTESIAN_POINT('Ctrl Pts',(54.4602778672668,11.2917992749461,-7.0227986525888));
#44426=CARTESIAN_POINT('Ctrl Pts',(54.5015923607319,11.0939065095575,-7.03987261114144));
#44427=CARTESIAN_POINT('Ctrl Pts',(54.5015923607319,11.,-7.03987261114144));
#44428=CARTESIAN_POINT('Ctrl Pts',(53.6250878309457,11.9970763379733,-5.95707109672624));
#44429=CARTESIAN_POINT('Ctrl Pts',(53.893972841279,11.9760715488571,-6.20791284186137));
#44430=CARTESIAN_POINT('Ctrl Pts',(54.3280790943459,11.748746829869,-6.59126738748239));
#44431=CARTESIAN_POINT('Ctrl Pts',(54.6334138394395,11.2917992749461,-6.83525865116221));
#44432=CARTESIAN_POINT('Ctrl Pts',(54.667728240488,11.0939065095575,-6.8599150740943));
#44433=CARTESIAN_POINT('Ctrl Pts',(54.667728240488,11.,-6.8599150740943));
#44434=CARTESIAN_POINT('Ctrl Pts',(53.8507498582491,11.9970763379733,-5.71263514045823));
#44435=CARTESIAN_POINT('Ctrl Pts',(54.122235037212,11.9760715488571,-5.9606603962042));
#44436=CARTESIAN_POINT('Ctrl Pts',(54.5389866050285,11.748746829869,-6.36281344831557));
#44437=CARTESIAN_POINT('Ctrl Pts',(54.8065498116121,11.2917992749461,-6.64771864973562));
#44438=CARTESIAN_POINT('Ctrl Pts',(54.833864120244,11.0939065095575,-6.67995753704715));
#44439=CARTESIAN_POINT('Ctrl Pts',(54.833864120244,11.,-6.67995753704715));
#44440=CARTESIAN_POINT('Ctrl Pts',(54.0764118855525,11.9970763379733,-5.46819918419023));
#44441=CARTESIAN_POINT('Ctrl Pts',(54.3504972331451,11.9760715488571,-5.71340795054702));
#44442=CARTESIAN_POINT('Ctrl Pts',(54.7498941157113,11.748746829869,-6.13435950914877));
#44443=CARTESIAN_POINT('Ctrl Pts',(54.9796857837848,11.2917992749461,-6.46017864830904));
#44444=CARTESIAN_POINT('Ctrl Pts',(55.,11.0939065095575,-6.5));
#44445=CARTESIAN_POINT('Ctrl Pts',(55.,11.,-6.5));
#44446=CARTESIAN_POINT('Ctrl Pts',(54.0764118855525,11.9970763379733,-5.46819918419023));
#44447=CARTESIAN_POINT('Ctrl Pts',(54.3504972331451,11.9760715488571,-5.71340795054702));
#44448=CARTESIAN_POINT('Ctrl Pts',(54.7498941157113,11.748746829869,-6.13435950914877));
#44449=CARTESIAN_POINT('Ctrl Pts',(54.9796857837848,11.2917992749461,-6.46017864830904));
#44450=CARTESIAN_POINT('Ctrl Pts',(55.,11.0939065095575,-6.5));
#44451=CARTESIAN_POINT('Ctrl Pts',(55.,11.,-6.5));
#44452=CARTESIAN_POINT('Ctrl Pts',(54.5015923607319,11.,-7.03987261114144));
#44453=CARTESIAN_POINT('Ctrl Pts',(54.5015923607319,11.0939065095575,-7.03987261114144));
#44454=CARTESIAN_POINT('Ctrl Pts',(54.4602778672668,11.2917992749461,-7.0227986525888));
#44455=CARTESIAN_POINT('Ctrl Pts',(54.1171715836631,11.748746829869,-6.8197213266492));
#44456=CARTESIAN_POINT('Ctrl Pts',(53.665710645346,11.9760715488571,-6.45516528751854));
#44457=CARTESIAN_POINT('Ctrl Pts',(53.3994258036423,11.9970763379733,-6.20150705299425));
#44458=CARTESIAN_POINT('Origin',(39.3002229812147,11.,-7.25278726518407));
#44459=CARTESIAN_POINT('',(29.9600637960156,12.,-8.));
#44460=CARTESIAN_POINT('Origin',(29.9600637960156,11.,-8.));
#44461=CARTESIAN_POINT('',(39.3002229812147,12.,-7.25278726518407));
#44462=CARTESIAN_POINT('Origin',(23.,8.1,0.));
#44463=CARTESIAN_POINT('',(39.,8.1,-7.));
#44464=CARTESIAN_POINT('',(34.,8.1,6.5));
#44465=CARTESIAN_POINT('',(12.95,8.1,-2.));
#44466=CARTESIAN_POINT('Origin',(16.,8.1,-2.));
#44467=CARTESIAN_POINT('',(-3.05,8.1,3.73517273739943E-16));
#44468=CARTESIAN_POINT('Origin',(0.,8.1,0.));
#44469=CARTESIAN_POINT('Origin',(55.,-12.,-7.));
#44470=CARTESIAN_POINT('',(50.,3.87298334620742,-7.));
#44471=CARTESIAN_POINT('',(50.,3.87298334620742,-7.));
#44472=CARTESIAN_POINT('',(50.,-3.87298334620742,-7.));
#44473=CARTESIAN_POINT('',(50.,-6.,-7.));
#44474=CARTESIAN_POINT('',(50.,-3.87298334620742,-7.));
#44475=CARTESIAN_POINT('Ctrl Pts',(54.0739345923054,-11.9972630926995,7.36867780326845));
#44476=CARTESIAN_POINT('Ctrl Pts',(54.0729086719546,-11.9973391518693,7.36768833576852));
#44477=CARTESIAN_POINT('Ctrl Pts',(54.0688659711553,-11.9976915991107,7.36379269873525));
#44478=CARTESIAN_POINT('Ctrl Pts',(54.0471711411876,-11.9989714998638,7.34303721500929));
#44479=CARTESIAN_POINT('Ctrl Pts',(54.0269258214969,-11.9997129437195,7.32379656765431));
#44480=CARTESIAN_POINT('Ctrl Pts',(54.0051272255687,-12.0000530049878,7.30313001690389));
#44481=CARTESIAN_POINT('Ctrl Pts',(54.0010359532624,-12.,7.29924905261381));
#44482=CARTESIAN_POINT('Ctrl Pts',(54.,-12.,7.29826682694392));
#44483=CARTESIAN_POINT('Ctrl Pts',(53.8388489959598,-11.9972630926995,7.6037633996141));
#44484=CARTESIAN_POINT('Ctrl Pts',(53.8378352265592,-11.9973391518693,7.60276178116386));
#44485=CARTESIAN_POINT('Ctrl Pts',(53.8338827986705,-11.9976915991107,7.59877587122005));
#44486=CARTESIAN_POINT('Ctrl Pts',(53.8124635143653,-11.9989714998638,7.57774484183155));
#44487=CARTESIAN_POINT('Ctrl Pts',(53.7926063578387,-11.9997129437195,7.5581160313125));
#44488=CARTESIAN_POINT('Ctrl Pts',(53.771093178854,-12.0000530049878,7.53716406361864));
#44489=CARTESIAN_POINT('Ctrl Pts',(53.7671069863795,-12.,7.53317801949668));
#44490=CARTESIAN_POINT('Ctrl Pts',(53.7660889423146,-12.,7.53217788462928));
#44491=CARTESIAN_POINT('Ctrl Pts',(53.6037633996141,-11.9972630926995,7.83884899595975));
#44492=CARTESIAN_POINT('Ctrl Pts',(53.6027617811639,-11.9973391518693,7.8378352265592));
#44493=CARTESIAN_POINT('Ctrl Pts',(53.59877587122,-11.9982153918639,7.83387226013102));
#44494=CARTESIAN_POINT('Ctrl Pts',(53.5777448418315,-11.9985200268038,7.81218733844659));
#44495=CARTESIAN_POINT('Ctrl Pts',(53.5581160313125,-12.0001842955338,7.79240311946324));
#44496=CARTESIAN_POINT('Ctrl Pts',(53.5371640636186,-11.999532009425,7.77100498101964));
#44497=CARTESIAN_POINT('Ctrl Pts',(53.5331780194967,-12.,7.76710698637954));
#44498=CARTESIAN_POINT('Ctrl Pts',(53.5321778846293,-12.,7.76608894231464));
#44499=CARTESIAN_POINT('Ctrl Pts',(53.3686778032684,-11.9972630926995,8.0739345923054));
#44500=CARTESIAN_POINT('Ctrl Pts',(53.3676883357685,-11.9973391518693,8.07290867195454));
#44501=CARTESIAN_POINT('Ctrl Pts',(53.3637926987352,-11.9976915991107,8.0688659711553));
#44502=CARTESIAN_POINT('Ctrl Pts',(53.3430372150093,-11.9989714998638,8.04717114118757));
#44503=CARTESIAN_POINT('Ctrl Pts',(53.3237965676543,-11.9997129437195,8.02692582149689));
#44504=CARTESIAN_POINT('Ctrl Pts',(53.3031300169039,-12.0000530049878,8.00512722556869));
#44505=CARTESIAN_POINT('Ctrl Pts',(53.2992490526138,-12.,8.00103595326241));
#44506=CARTESIAN_POINT('Ctrl Pts',(53.2982668269439,-12.,8.));
#44507=CARTESIAN_POINT('',(53.3686778032684,-11.9972630926995,8.0739345923054));
#44508=CARTESIAN_POINT('Ctrl Pts',(53.3686778032684,-11.9972630926995,8.0739345923054));
#44509=CARTESIAN_POINT('Ctrl Pts',(53.6037633996141,-11.9972630926995,7.83884899595975));
#44510=CARTESIAN_POINT('Ctrl Pts',(53.8388489959598,-11.9972630926995,7.6037633996141));
#44511=CARTESIAN_POINT('Ctrl Pts',(54.0739345923054,-11.9972630926995,7.36867780326845));
#44512=CARTESIAN_POINT('Ctrl Pts',(53.3686778032684,-11.9972630926995,8.0739345923054));
#44513=CARTESIAN_POINT('Ctrl Pts',(53.3683611391569,-11.9972874342867,8.07360626201012));
#44514=CARTESIAN_POINT('Ctrl Pts',(53.3680413192552,-11.9973118857529,8.0732746272395));
#44515=CARTESIAN_POINT('Ctrl Pts',(53.3676471644628,-11.9973417925779,8.0728652782713));
#44516=CARTESIAN_POINT('Ctrl Pts',(53.3672333737902,-11.9973731892917,8.07243553648429));
#44517=CARTESIAN_POINT('Ctrl Pts',(53.3667378598292,-11.9974105876503,8.07192035603661));
#44518=CARTESIAN_POINT('Ctrl Pts',(53.3661183826235,-11.9974566676542,8.07127549475271));
#44519=CARTESIAN_POINT('Ctrl Pts',(53.3654580683611,-11.9975057853351,8.07058812304793));
#44520=CARTESIAN_POINT('Ctrl Pts',(53.3646571866552,-11.9975647402856,8.06975369898109));
#44521=CARTESIAN_POINT('Ctrl Pts',(53.3637054463746,-11.9976331424649,8.06876127584374));
#44522=CARTESIAN_POINT('Ctrl Pts',(53.362653023559,-11.997708780762,8.06766386642043));
#44523=CARTESIAN_POINT('Ctrl Pts',(53.3614165408252,-11.9977958975481,8.0663736798044));
#44524=CARTESIAN_POINT('Ctrl Pts',(53.3600254874228,-11.9978903916136,8.06492123169862));
#44525=CARTESIAN_POINT('Ctrl Pts',(53.3582659835748,-11.9980099144669,8.06308407143828));
#44526=CARTESIAN_POINT('Ctrl Pts',(53.3562600906717,-11.9981409874224,8.06098824295537));
#44527=CARTESIAN_POINT('Ctrl Pts',(53.3541260503937,-11.998272326323,8.05875680809654));
#44528=CARTESIAN_POINT('Ctrl Pts',(53.3519223757936,-11.998407950848,8.05645256090358));
#44529=CARTESIAN_POINT('Ctrl Pts',(53.3495866187313,-11.998543466039,8.05400847853294));
#44530=CARTESIAN_POINT('Ctrl Pts',(53.347256780727,-11.9986694592396,8.0515685095969));
#44531=CARTESIAN_POINT('Ctrl Pts',(53.3454689924396,-11.9987661394242,8.04969621294899));
#44532=CARTESIAN_POINT('Ctrl Pts',(53.3436854660617,-11.998857297748,8.04782715956495));
#44533=CARTESIAN_POINT('Ctrl Pts',(53.3419450818544,-11.9989413499516,8.04600194948922));
#44534=CARTESIAN_POINT('Ctrl Pts',(53.3403729432991,-11.9990172766978,8.04435318531431));
#44535=CARTESIAN_POINT('Ctrl Pts',(53.3388364015668,-11.9990874483239,8.04274061126351));
#44536=CARTESIAN_POINT('Ctrl Pts',(53.3373354567718,-11.9991523945683,8.04116421295797));
#44537=CARTESIAN_POINT('Ctrl Pts',(53.3359014880526,-11.9992144427416,8.03965815766076));
#44538=CARTESIAN_POINT('Ctrl Pts',(53.3345003990797,-11.999271755233,8.03818553003495));
#44539=CARTESIAN_POINT('Ctrl Pts',(53.3330989620326,-11.9993259033641,8.0367115631036));
#44540=CARTESIAN_POINT('Ctrl Pts',(53.3316835335098,-11.9993805920919,8.03522288058259));
#44541=CARTESIAN_POINT('Ctrl Pts',(53.3302615515418,-11.9994322838975,8.03372633218491));
#44542=CARTESIAN_POINT('Ctrl Pts',(53.328804648363,-11.9994816923651,8.03219233801592));
#44543=CARTESIAN_POINT('Ctrl Pts',(53.3272371261908,-11.9995348522934,8.03054187152845));
#44544=CARTESIAN_POINT('Ctrl Pts',(53.3256295253259,-11.9995852953059,8.02884842046903));
#44545=CARTESIAN_POINT('Ctrl Pts',(53.3239879980521,-11.999632219018,8.02711875183636));
#44546=CARTESIAN_POINT('Ctrl Pts',(53.3221078268019,-11.9996859644633,8.02513762530408));
#44547=CARTESIAN_POINT('Ctrl Pts',(53.3201836730757,-11.9997349728798,8.02310953786485));
#44548=CARTESIAN_POINT('Ctrl Pts',(53.3182711113751,-11.999777510105,8.02109337071663));
#44549=CARTESIAN_POINT('Ctrl Pts',(53.315658940947,-11.9998356073061,8.01833969631172));
#44550=CARTESIAN_POINT('Ctrl Pts',(53.3130713611079,-11.9998812347755,8.01561139406509));
#44551=CARTESIAN_POINT('Ctrl Pts',(53.3107102640878,-11.9999139058313,8.01312177294044));
#44552=CARTESIAN_POINT('Ctrl Pts',(53.3089394413228,-11.9999384091233,8.01125455709695));
#44553=CARTESIAN_POINT('Ctrl Pts',(53.3072984621054,-11.9999557986327,8.00952417278428));
#44554=CARTESIAN_POINT('Ctrl Pts',(53.3058574649829,-11.9999679622468,8.00800465364294));
#44555=CARTESIAN_POINT('Ctrl Pts',(53.3046394106088,-11.9999782439768,8.006720225723));
#44556=CARTESIAN_POINT('Ctrl Pts',(53.3035646306533,-11.9999848583685,8.00558686693279));
#44557=CARTESIAN_POINT('Ctrl Pts',(53.3026501024977,-11.9999893162497,8.0046224870448));
#44558=CARTESIAN_POINT('Ctrl Pts',(53.3017902315958,-11.9999935077033,8.00371574382527));
#44559=CARTESIAN_POINT('Ctrl Pts',(53.3010724325772,-11.9999958172979,8.00295880824015));
#44560=CARTESIAN_POINT('Ctrl Pts',(53.3004808769946,-11.9999972739225,8.00233498342449));
#44561=CARTESIAN_POINT('Ctrl Pts',(53.2999292531747,-11.9999986322206,8.00175326864076));
#44562=CARTESIAN_POINT('Ctrl Pts',(53.2994875514495,-11.999999249454,8.00128745462601));
#44563=CARTESIAN_POINT('Ctrl Pts',(53.299112508452,-11.9999996022395,8.00089191980187));
#44564=CARTESIAN_POINT('Ctrl Pts',(53.2987993493698,-11.9999998968136,8.00056165014393));
#44565=CARTESIAN_POINT('Ctrl Pts',(53.2985322795654,-12.,8.00027997283885));
#44566=CARTESIAN_POINT('Ctrl Pts',(53.2982668269439,-12.,8.));
#44567=CARTESIAN_POINT('Ctrl Pts',(53.3686778032684,11.9972630926995,8.07393459230539));
#44568=CARTESIAN_POINT('Ctrl Pts',(53.3676883357685,11.9973391518693,8.07290867195453));
#44569=CARTESIAN_POINT('Ctrl Pts',(53.3637926987353,11.9976915991107,8.0688659711553));
#44570=CARTESIAN_POINT('Ctrl Pts',(53.3430372150093,11.9989714998638,8.04717114118756));
#44571=CARTESIAN_POINT('Ctrl Pts',(53.3237965676543,11.9997129437196,8.02692582149689));
#44572=CARTESIAN_POINT('Ctrl Pts',(53.3031300169039,12.0000530049878,8.00512722556869));
#44573=CARTESIAN_POINT('Ctrl Pts',(53.2992490526138,12.,8.00103595326241));
#44574=CARTESIAN_POINT('Ctrl Pts',(53.2982668269439,12.,8.));
#44575=CARTESIAN_POINT('Ctrl Pts',(53.6037633996141,11.9972630926995,7.83884899595974));
#44576=CARTESIAN_POINT('Ctrl Pts',(53.6027617811638,11.9973391518693,7.83783522655919));
#44577=CARTESIAN_POINT('Ctrl Pts',(53.5987758712201,11.9976915991107,7.83388279867049));
#44578=CARTESIAN_POINT('Ctrl Pts',(53.5777448418316,11.9989714998638,7.81246351436529));
#44579=CARTESIAN_POINT('Ctrl Pts',(53.5581160313125,11.9997129437196,7.7926063578387));
#44580=CARTESIAN_POINT('Ctrl Pts',(53.5371640636187,12.0000530049878,7.77109317885394));
#44581=CARTESIAN_POINT('Ctrl Pts',(53.5331780194967,12.,7.76710698637954));
#44582=CARTESIAN_POINT('Ctrl Pts',(53.5321778846293,12.,7.76608894231464));
#44583=CARTESIAN_POINT('Ctrl Pts',(53.8388489959597,11.9972630926995,7.60376339961409));
#44584=CARTESIAN_POINT('Ctrl Pts',(53.8378352265592,11.9973391518693,7.60276178116385));
#44585=CARTESIAN_POINT('Ctrl Pts',(53.833872260131,11.9982153918639,7.59877587122005));
#44586=CARTESIAN_POINT('Ctrl Pts',(53.8121873384466,11.9985200268038,7.57774484183155));
#44587=CARTESIAN_POINT('Ctrl Pts',(53.7924031194632,12.0001842955338,7.55811603131252));
#44588=CARTESIAN_POINT('Ctrl Pts',(53.7710049810197,11.999532009425,7.53716406361864));
#44589=CARTESIAN_POINT('Ctrl Pts',(53.7671069863795,12.,7.53317801949667));
#44590=CARTESIAN_POINT('Ctrl Pts',(53.7660889423146,12.,7.53217788462927));
#44591=CARTESIAN_POINT('Ctrl Pts',(54.0739345923054,11.9972630926995,7.36867780326844));
#44592=CARTESIAN_POINT('Ctrl Pts',(54.0729086719545,11.9973391518693,7.36768833576851));
#44593=CARTESIAN_POINT('Ctrl Pts',(54.0688659711553,11.9976915991107,7.36379269873524));
#44594=CARTESIAN_POINT('Ctrl Pts',(54.0471711411876,11.9989714998638,7.34303721500928));
#44595=CARTESIAN_POINT('Ctrl Pts',(54.0269258214969,11.9997129437196,7.32379656765433));
#44596=CARTESIAN_POINT('Ctrl Pts',(54.0051272255687,12.0000530049878,7.30313001690389));
#44597=CARTESIAN_POINT('Ctrl Pts',(54.0010359532624,12.,7.2992490526138));
#44598=CARTESIAN_POINT('Ctrl Pts',(54.,12.,7.29826682694391));
#44599=CARTESIAN_POINT('',(53.2982668269439,12.,8.));
#44600=CARTESIAN_POINT('',(53.3686778032684,11.9972630926995,8.07393459230539));
#44601=CARTESIAN_POINT('Ctrl Pts',(53.2982668269439,12.,8.));
#44602=CARTESIAN_POINT('Ctrl Pts',(53.2985811322872,12.,8.00033149779709));
#44603=CARTESIAN_POINT('Ctrl Pts',(53.2988985821763,11.9999998632791,8.00066630989117));
#44604=CARTESIAN_POINT('Ctrl Pts',(53.2992901434245,11.9999994175998,8.00107925901207));
#44605=CARTESIAN_POINT('Ctrl Pts',(53.2997012071609,11.9999989497226,8.00151277588685));
#44606=CARTESIAN_POINT('Ctrl Pts',(53.3001937467632,11.9999981461834,8.00203219498426));
#44607=CARTESIAN_POINT('Ctrl Pts',(53.3008098989545,11.9999964035612,8.00268195165242));
#44608=CARTESIAN_POINT('Ctrl Pts',(53.3014666575414,11.9999945460946,8.00337452935848));
#44609=CARTESIAN_POINT('Ctrl Pts',(53.302263581072,11.9999916163369,8.00421489865621));
#44610=CARTESIAN_POINT('Ctrl Pts',(53.3032109845114,11.9999864073118,8.00521394204844));
#44611=CARTESIAN_POINT('Ctrl Pts',(53.3042585528888,11.9999806475585,8.00631861005127));
#44612=CARTESIAN_POINT('Ctrl Pts',(53.3054896985523,11.9999720586087,8.00761685387812));
#44613=CARTESIAN_POINT('Ctrl Pts',(53.3068751339638,11.9999587961682,8.00907777317183));
#44614=CARTESIAN_POINT('Ctrl Pts',(53.3086269933134,11.9999420260395,8.0109250805978));
#44615=CARTESIAN_POINT('Ctrl Pts',(53.3106246425574,11.9999175989922,8.01303154298942));
#44616=CARTESIAN_POINT('Ctrl Pts',(53.3127506011298,11.9998833589397,8.01527313050642));
#44617=CARTESIAN_POINT('Ctrl Pts',(53.3149479827775,11.9998479685685,8.01759002573457));
#44618=CARTESIAN_POINT('Ctrl Pts',(53.3172778862811,11.9998020541947,8.02004647877186));
#44619=CARTESIAN_POINT('Ctrl Pts',(53.3196028144622,11.9997469068523,8.0224971606943));
#44620=CARTESIAN_POINT('Ctrl Pts',(53.3213861058047,11.9997046071464,8.02437690901994));
#44621=CARTESIAN_POINT('Ctrl Pts',(53.3231656968351,11.9996570221597,8.0262524447248));
#44622=CARTESIAN_POINT('Ctrl Pts',(53.3249029587413,11.999605600683,8.02808278980505));
#44623=CARTESIAN_POINT('Ctrl Pts',(53.326472213838,11.9995591520651,8.02973612620502));
#44624=CARTESIAN_POINT('Ctrl Pts',(53.3280065398011,11.9995096475949,8.03135217868033));
#44625=CARTESIAN_POINT('Ctrl Pts',(53.3295060480933,11.999457634203,8.03293079764295));
#44626=CARTESIAN_POINT('Ctrl Pts',(53.3309381134142,11.9994079602031,8.03443841549555));
#44627=CARTESIAN_POINT('Ctrl Pts',(53.3323380371434,11.999356061863,8.03591148724446));
#44628=CARTESIAN_POINT('Ctrl Pts',(53.3337390092771,11.9993009489689,8.03738466784339));
#44629=CARTESIAN_POINT('Ctrl Pts',(53.3351545720245,11.9992452620942,8.03887319108083));
#44630=CARTESIAN_POINT('Ctrl Pts',(53.3365774080489,11.9991860424165,8.04036832959046));
#44631=CARTESIAN_POINT('Ctrl Pts',(53.3380358765603,11.9991218195899,8.04189975679361));
#44632=CARTESIAN_POINT('Ctrl Pts',(53.339605020087,11.9990527232523,8.043547395439));
#44633=CARTESIAN_POINT('Ctrl Pts',(53.3412150611489,11.9989777892668,8.04523667284072));
#44634=CARTESIAN_POINT('Ctrl Pts',(53.3428597205588,11.9988967216938,8.04696104118784));
#44635=CARTESIAN_POINT('Ctrl Pts',(53.3447432666844,11.9988038790588,8.04893587397064));
#44636=CARTESIAN_POINT('Ctrl Pts',(53.3466716908128,11.9987029134811,8.05095617475291));
#44637=CARTESIAN_POINT('Ctrl Pts',(53.3485891250862,11.9985964429042,8.05296361221781));
#44638=CARTESIAN_POINT('Ctrl Pts',(53.3512088491728,11.9984509758397,8.05570630455006));
#44639=CARTESIAN_POINT('Ctrl Pts',(53.3538050841659,11.9982950689302,8.05842184964093));
#44640=CARTESIAN_POINT('Ctrl Pts',(53.3561748403525,11.9981439573354,8.06089860782276));
#44641=CARTESIAN_POINT('Ctrl Pts',(53.3579521574925,11.9980306236394,8.06275617645914));
#44642=CARTESIAN_POINT('Ctrl Pts',(53.3595996241856,11.9979203495849,8.06447687506964));
#44643=CARTESIAN_POINT('Ctrl Pts',(53.3610467017614,11.9978204591454,8.06598735720454));
#44644=CARTESIAN_POINT('Ctrl Pts',(53.3622698769639,11.9977360244816,8.06726412655143));
#44645=CARTESIAN_POINT('Ctrl Pts',(53.3633494900304,11.9976591045262,8.06839030066085));
#44646=CARTESIAN_POINT('Ctrl Pts',(53.3642684226497,11.9975925133009,8.06934823289768));
#44647=CARTESIAN_POINT('Ctrl Pts',(53.3651324109649,11.9975299036608,8.07024888898712));
#44648=CARTESIAN_POINT('Ctrl Pts',(53.3658539549706,11.9974764800598,8.0710004010633));
#44649=CARTESIAN_POINT('Ctrl Pts',(53.3664488792868,11.9974320284378,8.07161947114109));
#44650=CARTESIAN_POINT('Ctrl Pts',(53.3670036310318,11.9973905784344,8.07219673819267));
#44651=CARTESIAN_POINT('Ctrl Pts',(53.3674481384678,11.9973569415985,8.07265869230704));
#44652=CARTESIAN_POINT('Ctrl Pts',(53.3678257711913,11.9973282258331,8.07305073549685));
#44653=CARTESIAN_POINT('Ctrl Pts',(53.3681411633075,11.9973042429379,8.07337816297755));
#44654=CARTESIAN_POINT('Ctrl Pts',(53.3684102955234,11.9972836556963,8.07365722934034));
#44655=CARTESIAN_POINT('Ctrl Pts',(53.3686778032684,11.9972630926995,8.07393459230539));
#44656=CARTESIAN_POINT('',(54.0739345923054,11.9972630926995,7.36867780326844));
#44657=CARTESIAN_POINT('Ctrl Pts',(54.0739345923054,11.9972630926995,7.36867780326844));
#44658=CARTESIAN_POINT('Ctrl Pts',(53.8388489959597,11.9972630926995,7.60376339961409));
#44659=CARTESIAN_POINT('Ctrl Pts',(53.6037633996141,11.9972630926995,7.83884899595974));
#44660=CARTESIAN_POINT('Ctrl Pts',(53.3686778032684,11.9972630926995,8.07393459230539));
#44661=CARTESIAN_POINT('',(54.,12.,7.29826682694391));
#44662=CARTESIAN_POINT('Ctrl Pts',(54.0739345923054,11.9972630926995,7.36867780326844));
#44663=CARTESIAN_POINT('Ctrl Pts',(54.0736062620101,11.9972874342867,7.3683611391569));
#44664=CARTESIAN_POINT('Ctrl Pts',(54.0732746272395,11.9973118857528,7.36804131925523));
#44665=CARTESIAN_POINT('Ctrl Pts',(54.0728652782713,11.9973417925779,7.36764716446279));
#44666=CARTESIAN_POINT('Ctrl Pts',(54.0724355364843,11.9973731892917,7.36723337379024));
#44667=CARTESIAN_POINT('Ctrl Pts',(54.0719203560366,11.9974105876503,7.36673785982923));
#44668=CARTESIAN_POINT('Ctrl Pts',(54.0712754947527,11.9974566676542,7.36611838262348));
#44669=CARTESIAN_POINT('Ctrl Pts',(54.0705881230479,11.9975057853351,7.36545806836115));
#44670=CARTESIAN_POINT('Ctrl Pts',(54.0697536989811,11.9975647402856,7.36465718665516));
#44671=CARTESIAN_POINT('Ctrl Pts',(54.0687612758438,11.9976331424649,7.3637054463746));
#44672=CARTESIAN_POINT('Ctrl Pts',(54.0676638664205,11.997708780762,7.36265302355903));
#44673=CARTESIAN_POINT('Ctrl Pts',(54.0663736798044,11.9977958975481,7.36141654082529));
#44674=CARTESIAN_POINT('Ctrl Pts',(54.0649212316987,11.9978903916136,7.36002548742284));
#44675=CARTESIAN_POINT('Ctrl Pts',(54.0630840714383,11.9980099144669,7.35826598357491));
#44676=CARTESIAN_POINT('Ctrl Pts',(54.0609882429554,11.9981409874224,7.3562600906717));
#44677=CARTESIAN_POINT('Ctrl Pts',(54.0587568080966,11.998272326323,7.35412605039371));
#44678=CARTESIAN_POINT('Ctrl Pts',(54.0564525609036,11.998407950848,7.35192237579359));
#44679=CARTESIAN_POINT('Ctrl Pts',(54.0540084785329,11.998543466039,7.34958661873129));
#44680=CARTESIAN_POINT('Ctrl Pts',(54.0515685095969,11.9986694592396,7.34725678072702));
#44681=CARTESIAN_POINT('Ctrl Pts',(54.049696212949,11.9987661394242,7.34546899243955));
#44682=CARTESIAN_POINT('Ctrl Pts',(54.0478271595649,11.9988572977481,7.34368546606171));
#44683=CARTESIAN_POINT('Ctrl Pts',(54.0460019494891,11.9989413499516,7.34194508185438));
#44684=CARTESIAN_POINT('Ctrl Pts',(54.0443531853142,11.9990172766978,7.34037294329907));
#44685=CARTESIAN_POINT('Ctrl Pts',(54.0427406112634,11.9990874483239,7.33883640156666));
#44686=CARTESIAN_POINT('Ctrl Pts',(54.0411642129578,11.9991523945683,7.33733545677172));
#44687=CARTESIAN_POINT('Ctrl Pts',(54.0396581576594,11.9992144427417,7.33590148805134));
#44688=CARTESIAN_POINT('Ctrl Pts',(54.0381855300325,11.9992717552331,7.33450039907735));
#44689=CARTESIAN_POINT('Ctrl Pts',(54.0367115631,11.9993259033642,7.33309896202914));
#44690=CARTESIAN_POINT('Ctrl Pts',(54.0352228805789,11.999380592092,7.33168353350629));
#44691=CARTESIAN_POINT('Ctrl Pts',(54.0337263321811,11.9994322838977,7.33026155153822));
#44692=CARTESIAN_POINT('Ctrl Pts',(54.0321923380121,11.9994816923653,7.32880464835936));
#44693=CARTESIAN_POINT('Ctrl Pts',(54.0305418715244,11.9995348522935,7.32723712618688));
#44694=CARTESIAN_POINT('Ctrl Pts',(54.0288484204647,11.9995852953061,7.32562952532175));
#44695=CARTESIAN_POINT('Ctrl Pts',(54.0271187518318,11.9996322190181,7.32398799804776));
#44696=CARTESIAN_POINT('Ctrl Pts',(54.0251376252991,11.9996859644635,7.32210782679718));
#44697=CARTESIAN_POINT('Ctrl Pts',(54.0231095378595,11.99973497288,7.32018367307067));
#44698=CARTESIAN_POINT('Ctrl Pts',(54.021093370711,11.9997775101051,7.31827111136975));
#44699=CARTESIAN_POINT('Ctrl Pts',(54.0183396963066,11.9998356073062,7.31565894094208));
#44700=CARTESIAN_POINT('Ctrl Pts',(54.0156113940606,11.9998812347755,7.31307136110358));
#44701=CARTESIAN_POINT('Ctrl Pts',(54.0131217729366,11.9999139058314,7.31071026408421));
#44702=CARTESIAN_POINT('Ctrl Pts',(54.0112545570936,11.9999384091233,7.30893944131968));
#44703=CARTESIAN_POINT('Ctrl Pts',(54.0095241727815,11.9999557986327,7.30729846210273));
#44704=CARTESIAN_POINT('Ctrl Pts',(54.0080046536406,11.9999679622468,7.30585746498073));
#44705=CARTESIAN_POINT('Ctrl Pts',(54.0067202257209,11.9999782439769,7.30463941060684));
#44706=CARTESIAN_POINT('Ctrl Pts',(54.0055868669309,11.9999848583685,7.30356463065154));
#44707=CARTESIAN_POINT('Ctrl Pts',(54.0046224870432,11.9999893162497,7.30265010249617));
#44708=CARTESIAN_POINT('Ctrl Pts',(54.0037157438238,11.9999935077033,7.30179023159441));
#44709=CARTESIAN_POINT('Ctrl Pts',(54.0029588082389,11.9999958172979,7.30107243257607));
#44710=CARTESIAN_POINT('Ctrl Pts',(54.0023349834234,11.9999972739225,7.30048087699363));
#44711=CARTESIAN_POINT('Ctrl Pts',(54.0017532686398,11.9999986322206,7.29992925317381));
#44712=CARTESIAN_POINT('Ctrl Pts',(54.0012874546252,11.999999249454,7.29948755144875));
#44713=CARTESIAN_POINT('Ctrl Pts',(54.0008919198012,11.9999996022395,7.29911250845132));
#44714=CARTESIAN_POINT('Ctrl Pts',(54.0005616501435,11.9999998968136,7.29879934936943));
#44715=CARTESIAN_POINT('Ctrl Pts',(54.0002799728386,12.,7.29853227956515));
#44716=CARTESIAN_POINT('Ctrl Pts',(54.,12.,7.29826682694391));
#44717=CARTESIAN_POINT('',(53.649133413472,12.,7.64913341347195));
#44718=CARTESIAN_POINT('Ctrl Pts',(54.0739345923054,11.9972630926995,7.36867780326844));
#44719=CARTESIAN_POINT('Ctrl Pts',(54.3510337690789,11.9767196525453,7.6359311328699));
#44720=CARTESIAN_POINT('Ctrl Pts',(54.7553166986943,11.7446620906573,8.09873418111303));
#44721=CARTESIAN_POINT('Ctrl Pts',(54.9514928044654,11.3451725484551,8.40875696033662));
#44722=CARTESIAN_POINT('Ctrl Pts',(54.9944234105006,11.1325383755072,8.488654852558));
#44723=CARTESIAN_POINT('Ctrl Pts',(55.,11.0439996496616,8.5));
#44724=CARTESIAN_POINT('Ctrl Pts',(55.,11.,8.5));
#44725=CARTESIAN_POINT('Ctrl Pts',(53.8388489959597,11.9972630926995,7.60376339961409));
#44726=CARTESIAN_POINT('Ctrl Pts',(54.1126662236759,11.9767196525453,7.87429867827289));
#44727=CARTESIAN_POINT('Ctrl Pts',(54.5364558595005,11.7446620906573,8.31759502030676));
#44728=CARTESIAN_POINT('Ctrl Pts',(54.7705808564225,11.3451725484551,8.58966890837954));
#44729=CARTESIAN_POINT('Ctrl Pts',(54.8258338911864,11.1325383755072,8.65724437187221));
#44730=CARTESIAN_POINT('Ctrl Pts',(54.8333333333333,11.0439996496616,8.66666666666667));
#44731=CARTESIAN_POINT('Ctrl Pts',(54.8333333333333,11.,8.66666666666667));
#44732=CARTESIAN_POINT('Ctrl Pts',(53.6037633996141,11.9972630926995,7.83884899595974));
#44733=CARTESIAN_POINT('Ctrl Pts',(53.8742986782729,11.9767196525453,8.11266622367587));
#44734=CARTESIAN_POINT('Ctrl Pts',(54.3175950203068,11.7446620906573,8.5364558595005));
#44735=CARTESIAN_POINT('Ctrl Pts',(54.5896689083795,11.3451725484551,8.77058085642246));
#44736=CARTESIAN_POINT('Ctrl Pts',(54.6572443718722,11.1325383755072,8.82583389118641));
#44737=CARTESIAN_POINT('Ctrl Pts',(54.6666666666667,11.0439996496616,8.83333333333333));
#44738=CARTESIAN_POINT('Ctrl Pts',(54.6666666666667,11.,8.83333333333333));
#44739=CARTESIAN_POINT('Ctrl Pts',(53.3686778032684,11.9972630926995,8.07393459230539));
#44740=CARTESIAN_POINT('Ctrl Pts',(53.6359311328699,11.9767196525453,8.35103376907885));
#44741=CARTESIAN_POINT('Ctrl Pts',(54.098734181113,11.7446620906573,8.75531669869423));
#44742=CARTESIAN_POINT('Ctrl Pts',(54.4087569603366,11.3451725484551,8.95149280446538));
#44743=CARTESIAN_POINT('Ctrl Pts',(54.488654852558,11.1325383755072,8.99442341050062));
#44744=CARTESIAN_POINT('Ctrl Pts',(54.5,11.0439996496616,9.));
#44745=CARTESIAN_POINT('Ctrl Pts',(54.5,11.,9.));
#44746=CARTESIAN_POINT('Ctrl Pts',(53.3686778032684,11.9972630926995,8.07393459230539));
#44747=CARTESIAN_POINT('Ctrl Pts',(53.6359311328699,11.9767196525453,8.35103376907885));
#44748=CARTESIAN_POINT('Ctrl Pts',(54.098734181113,11.7446620906573,8.75531669869423));
#44749=CARTESIAN_POINT('Ctrl Pts',(54.4087569603366,11.3451725484551,8.95149280446538));
#44750=CARTESIAN_POINT('Ctrl Pts',(54.488654852558,11.1325383755072,8.99442341050062));
#44751=CARTESIAN_POINT('Ctrl Pts',(54.5,11.0439996496616,9.));
#44752=CARTESIAN_POINT('Ctrl Pts',(54.5,11.,9.));
#44753=CARTESIAN_POINT('',(54.5,11.,9.));
#44754=CARTESIAN_POINT('Ctrl Pts',(55.,11.,8.5));
#44755=CARTESIAN_POINT('Ctrl Pts',(55.,11.0439996496616,8.5));
#44756=CARTESIAN_POINT('Ctrl Pts',(54.9944234105006,11.1325383755072,8.488654852558));
#44757=CARTESIAN_POINT('Ctrl Pts',(54.9514928044654,11.3451725484551,8.40875696033662));
#44758=CARTESIAN_POINT('Ctrl Pts',(54.7553166986943,11.7446620906573,8.09873418111303));
#44759=CARTESIAN_POINT('Ctrl Pts',(54.3510337690789,11.9767196525453,7.6359311328699));
#44760=CARTESIAN_POINT('Ctrl Pts',(54.0739345923054,11.9972630926995,7.36867780326844));
#44761=CARTESIAN_POINT('Origin',(54.75,8.1,8.75));
#44762=CARTESIAN_POINT('',(54.5,-11.,9.));
#44763=CARTESIAN_POINT('Ctrl Pts',(53.3686778032684,-11.9972630926995,8.0739345923054));
#44764=CARTESIAN_POINT('Ctrl Pts',(53.6359311328699,-11.9767196525453,8.35103376907886));
#44765=CARTESIAN_POINT('Ctrl Pts',(54.098734181113,-11.7446620906573,8.75531669869423));
#44766=CARTESIAN_POINT('Ctrl Pts',(54.4087569603366,-11.3451725484551,8.95149280446538));
#44767=CARTESIAN_POINT('Ctrl Pts',(54.488654852558,-11.1325383755072,8.99442341050062));
#44768=CARTESIAN_POINT('Ctrl Pts',(54.5,-11.0439996496616,9.));
#44769=CARTESIAN_POINT('Ctrl Pts',(54.5,-11.,9.));
#44770=CARTESIAN_POINT('Ctrl Pts',(53.6037633996141,-11.9972630926995,7.83884899595975));
#44771=CARTESIAN_POINT('Ctrl Pts',(53.8742986782729,-11.9767196525453,8.11266622367588));
#44772=CARTESIAN_POINT('Ctrl Pts',(54.3175950203067,-11.7446620906573,8.53645585950049));
#44773=CARTESIAN_POINT('Ctrl Pts',(54.5896689083795,-11.3451725484551,8.77058085642246));
#44774=CARTESIAN_POINT('Ctrl Pts',(54.6572443718722,-11.1325383755072,8.82583389118641));
#44775=CARTESIAN_POINT('Ctrl Pts',(54.6666666666667,-11.0439996496616,8.83333333333333));
#44776=CARTESIAN_POINT('Ctrl Pts',(54.6666666666667,-11.,8.83333333333333));
#44777=CARTESIAN_POINT('Ctrl Pts',(53.8388489959598,-11.9972630926995,7.6037633996141));
#44778=CARTESIAN_POINT('Ctrl Pts',(54.1126662236759,-11.9767196525453,7.87429867827289));
#44779=CARTESIAN_POINT('Ctrl Pts',(54.5364558595005,-11.7446620906573,8.31759502030676));
#44780=CARTESIAN_POINT('Ctrl Pts',(54.7705808564224,-11.3451725484551,8.58966890837954));
#44781=CARTESIAN_POINT('Ctrl Pts',(54.8258338911864,-11.1325383755072,8.6572443718722));
#44782=CARTESIAN_POINT('Ctrl Pts',(54.8333333333333,-11.0439996496616,8.66666666666667));
#44783=CARTESIAN_POINT('Ctrl Pts',(54.8333333333333,-11.,8.66666666666667));
#44784=CARTESIAN_POINT('Ctrl Pts',(54.0739345923054,-11.9972630926995,7.36867780326845));
#44785=CARTESIAN_POINT('Ctrl Pts',(54.3510337690789,-11.9767196525453,7.63593113286991));
#44786=CARTESIAN_POINT('Ctrl Pts',(54.7553166986942,-11.7446620906573,8.09873418111303));
#44787=CARTESIAN_POINT('Ctrl Pts',(54.9514928044654,-11.3451725484552,8.40875696033662));
#44788=CARTESIAN_POINT('Ctrl Pts',(54.9944234105006,-11.1325383755072,8.488654852558));
#44789=CARTESIAN_POINT('Ctrl Pts',(55.,-11.0439996496616,8.5));
#44790=CARTESIAN_POINT('Ctrl Pts',(55.,-11.,8.5));
#44791=CARTESIAN_POINT('Ctrl Pts',(54.5,-11.,9.));
#44792=CARTESIAN_POINT('Ctrl Pts',(54.5,-11.0439996496616,9.));
#44793=CARTESIAN_POINT('Ctrl Pts',(54.488654852558,-11.1325383755072,8.99442341050062));
#44794=CARTESIAN_POINT('Ctrl Pts',(54.4087569603366,-11.3451725484551,8.95149280446538));
#44795=CARTESIAN_POINT('Ctrl Pts',(54.098734181113,-11.7446620906573,8.75531669869423));
#44796=CARTESIAN_POINT('Ctrl Pts',(53.6359311328699,-11.9767196525453,8.35103376907886));
#44797=CARTESIAN_POINT('Ctrl Pts',(53.3686778032684,-11.9972630926995,8.0739345923054));
#44798=CARTESIAN_POINT('Origin',(11.5,-11.,8.));
#44799=CARTESIAN_POINT('Origin',(0.,-11.,8.));
#44800=CARTESIAN_POINT('Origin',(11.5,11.,8.));
#44801=CARTESIAN_POINT('',(7.96639400082368E-16,12.,8.));
#44802=CARTESIAN_POINT('',(11.5,12.,8.));
#44803=CARTESIAN_POINT('Origin',(7.96639400082368E-16,11.,8.));
#44804=CARTESIAN_POINT('Origin',(54.,11.,4.5));
#44805=CARTESIAN_POINT('',(54.,12.,4.5));
#44806=CARTESIAN_POINT('Origin',(26.5,11.,-8.));
#44807=CARTESIAN_POINT('',(0.,12.,-8.));
#44808=CARTESIAN_POINT('Origin',(0.,11.,-8.));
#44809=CARTESIAN_POINT('',(26.5,12.,-8.));
#44810=CARTESIAN_POINT('Origin',(0.,11.,0.));
#44811=CARTESIAN_POINT('Origin',(0.,12.,0.));
#44812=CARTESIAN_POINT('Origin',(23.,12.,0.));
#44813=CARTESIAN_POINT('',(12.95,12.,-2.));
#44814=CARTESIAN_POINT('Origin',(16.,12.,-2.));
#44815=CARTESIAN_POINT('',(-3.05,12.,-3.73517273739943E-16));
#44816=CARTESIAN_POINT('Origin',(0.,12.,0.));
#44817=CARTESIAN_POINT('Origin',(26.8002229812147,-11.,-8.25278726518407));
#44818=CARTESIAN_POINT('',(30.,-11.,-9.));
#44819=CARTESIAN_POINT('Origin',(29.9600637960156,-11.,-8.));
#44820=CARTESIAN_POINT('',(26.8799682034976,-11.,-9.24960254372019));
#44821=CARTESIAN_POINT('Origin',(0.,-11.,0.));
#44822=CARTESIAN_POINT('',(0.,-11.,-9.));
#44823=CARTESIAN_POINT('Origin',(0.,-11.,-8.));
#44824=CARTESIAN_POINT('Origin',(0.,-11.,0.));
#44825=CARTESIAN_POINT('Origin',(11.5,-11.,-8.));
#44826=CARTESIAN_POINT('',(11.5,-11.,-9.));
#44827=CARTESIAN_POINT('Origin',(0.,-8.1,-9.));
#44828=CARTESIAN_POINT('',(30.,-8.1,-9.));
#44829=CARTESIAN_POINT('',(0.,-8.1,-9.));
#44830=CARTESIAN_POINT('Origin',(0.,-8.1,0.));
#44831=CARTESIAN_POINT('Origin',(0.,-12.5,0.));
#44832=CARTESIAN_POINT('',(-3.05,-12.5,3.73517273739943E-16));
#44833=CARTESIAN_POINT('Origin',(0.,-12.5,0.));
#44834=CARTESIAN_POINT('',(-3.05,-12.5,3.73517273739943E-16));
#44835=CARTESIAN_POINT('Origin',(16.,-12.5,-2.));
#44836=CARTESIAN_POINT('',(12.95,-12.5,-2.));
#44837=CARTESIAN_POINT('Origin',(16.,-12.5,-2.));
#44838=CARTESIAN_POINT('',(12.95,-12.5,-2.));
#44839=CARTESIAN_POINT('Origin',(50.,0.,0.));
#44840=CARTESIAN_POINT('',(150.,-9.79717439317883E-16,8.));
#44841=CARTESIAN_POINT('Origin',(150.,0.,0.));
#44842=CARTESIAN_POINT('',(50.,-9.79717439317883E-16,8.));
#44843=CARTESIAN_POINT('Origin',(50.,0.,0.));
#44844=CARTESIAN_POINT('Origin',(150.,0.,79.9999999999995));
#44845=CARTESIAN_POINT('',(180.42851484533,-9.79717439317883E-16,14.7458393333612));
#44846=CARTESIAN_POINT('Origin',(183.809460939256,0.,7.49537703706801));
#44847=CARTESIAN_POINT('Origin',(150.,9.79717439317883E-16,79.9999999999995));
#44848=CARTESIAN_POINT('Origin',(183.809460939256,0.,7.49537703706801));
#44849=CARTESIAN_POINT('Origin',(50.,0.,0.));
#44850=CARTESIAN_POINT('Origin',(45.,-12.,6.5));
#44851=CARTESIAN_POINT('Origin',(30.,-8.1,-9.));
#44852=CARTESIAN_POINT('',(0.,0.,0.));
#44853=CARTESIAN_POINT('Origin',(76.0732233047034,-3.25953419062578E-16,
0.));
#44854=CARTESIAN_POINT('',(75.6464466094067,-2.60762735250063E-15,10.6464466094067));
#44855=CARTESIAN_POINT('Origin',(75.6464466094067,-6.51906838125157E-16,
0.));
#44856=CARTESIAN_POINT('',(76.5,1.34711147906209E-15,11.));
#44857=CARTESIAN_POINT('',(76.0732233047034,6.73555739531044E-16,10.8232233047034));
#44858=CARTESIAN_POINT('Origin',(76.5,0.,0.));
#44859=CARTESIAN_POINT('Origin',(75.5,0.,0.));
#44860=CARTESIAN_POINT('',(75.3535533905933,0.,10.3535533905933));
#44861=CARTESIAN_POINT('',(75.5,-1.28587913910472E-15,10.5));
#44862=CARTESIAN_POINT('Origin',(75.3535533905933,-6.33972300979564E-16,
0.));
#44863=CARTESIAN_POINT('Origin',(75.,0.,0.));
#44864=CARTESIAN_POINT('',(150.,-1.34711147906209E-15,11.));
#44865=CARTESIAN_POINT('Origin',(150.,0.,0.));
#44866=CARTESIAN_POINT('',(75.,-1.34711147906209E-15,11.));
#44867=CARTESIAN_POINT('Origin',(75.1767766952966,-3.16986150489782E-16,
0.));
#44868=CARTESIAN_POINT('',(75.,-1.16341445918999E-15,9.5));
#44869=CARTESIAN_POINT('',(75.1767766952966,-1.84965183155412E-15,9.92677669529664));
#44870=CARTESIAN_POINT('Origin',(75.,0.,0.));
#44871=CARTESIAN_POINT('Origin',(75.,0.,0.));
#44872=CARTESIAN_POINT('',(75.,-9.79717439317883E-16,8.));
#44873=CARTESIAN_POINT('Origin',(75.,0.,0.));
#44874=CARTESIAN_POINT('Origin',(184.715768726293,8.84447404295016E-31,
7.91799529880872));
#44875=CARTESIAN_POINT('',(185.382672042254,-8.57252759403147E-16,15.9526228550281));
#44876=CARTESIAN_POINT('Origin',(188.340999874439,8.5979550100686E-31,9.60846834577153));
#44877=CARTESIAN_POINT('',(180.066967847145,-1.34711147906209E-15,17.8873809562119));
#44878=CARTESIAN_POINT('Origin',(181.757440894108,-8.57252759403146E-16,
14.2621498080653));
#44879=CARTESIAN_POINT('',(184.715768726293,-11.,7.91799529880872));
#44880=CARTESIAN_POINT('Origin',(184.715768726293,8.84447404295016E-31,
7.91799529880872));
#44881=CARTESIAN_POINT('Origin',(184.715768726293,8.84447404295016E-31,
7.91799529880872));
#44882=CARTESIAN_POINT('Origin',(183.809460939256,8.84447404295016E-31,
7.49537703706802));
#44883=CARTESIAN_POINT('',(183.809460939256,-11.,7.49537703706799));
#44884=CARTESIAN_POINT('',(183.809460939256,-11.,7.49537703706802));
#44885=CARTESIAN_POINT('',(179.160660060108,1.34711147906209E-15,17.4647626944711));
#44886=CARTESIAN_POINT('Origin',(183.809460939256,0.,7.49537703706801));
#44887=CARTESIAN_POINT('Origin',(183.809460939256,0.,7.49537703706801));
#44888=CARTESIAN_POINT('Origin',(188.340999874439,-1.08770485875751E-30,
9.60846834577153));
#44889=CARTESIAN_POINT('Origin',(183.809460939256,-1.08770485875751E-30,
7.49537703706802));
#44890=CARTESIAN_POINT('',(180.42851484533,-9.79717439317883E-16,14.7458393333612));
#44891=CARTESIAN_POINT('Origin',(183.809460939256,0.,7.49537703706803));
#44892=CARTESIAN_POINT('Origin',(150.,0.,79.9999999999995));
#44893=CARTESIAN_POINT('',(150.,-9.79717439317883E-16,8.));
#44894=CARTESIAN_POINT('Origin',(150.,0.,0.));
#44895=CARTESIAN_POINT('Origin',(150.,9.79717439317883E-16,79.9999999999995));
#44896=CARTESIAN_POINT('Origin',(75.,0.,0.));
#44897=CARTESIAN_POINT('',(75.,-9.79717439317883E-16,8.));
#44898=CARTESIAN_POINT('Origin',(150.,0.,79.9999999999995));
#44899=CARTESIAN_POINT('Origin',(150.,1.34711147906209E-15,79.9999999999995));
#44900=CARTESIAN_POINT('',(0.,0.,0.));
#44901=CARTESIAN_POINT('Origin',(0.,5.1,0.));
#44902=CARTESIAN_POINT('',(-5.8,5.,-7.10295143505465E-16));
#44903=CARTESIAN_POINT('',(-6.,5.2,-7.34788079488412E-16));
#44904=CARTESIAN_POINT('',(-5.8,5.,-7.10295143505465E-16));
#44905=CARTESIAN_POINT('',(6.,5.2,0.));
#44906=CARTESIAN_POINT('Origin',(0.,5.2,0.));
#44907=CARTESIAN_POINT('',(5.8,5.,0.));
#44908=CARTESIAN_POINT('',(6.,5.2,0.));
#44909=CARTESIAN_POINT('Origin',(0.,5.,0.));
#44910=CARTESIAN_POINT('Origin',(-5.9,5.1,4.5));
#44911=CARTESIAN_POINT('',(-5.8,5.,18.));
#44912=CARTESIAN_POINT('',(-6.,5.2,18.));
#44913=CARTESIAN_POINT('',(-5.8,5.,18.));
#44914=CARTESIAN_POINT('',(-6.,5.2,4.5));
#44915=CARTESIAN_POINT('',(-5.8,5.,4.5));
#44916=CARTESIAN_POINT('Origin',(0.,5.1,18.));
#44917=CARTESIAN_POINT('',(5.8,5.,18.));
#44918=CARTESIAN_POINT('',(6.,5.2,18.));
#44919=CARTESIAN_POINT('',(5.8,5.,18.));
#44920=CARTESIAN_POINT('Origin',(0.,5.2,18.));
#44921=CARTESIAN_POINT('Origin',(0.,5.,18.));
#44922=CARTESIAN_POINT('Origin',(5.9,5.1,13.5));
#44923=CARTESIAN_POINT('',(6.,5.2,13.5));
#44924=CARTESIAN_POINT('',(5.8,5.,13.5));
#44925=CARTESIAN_POINT('Origin',(6.,5.,18.));
#44926=CARTESIAN_POINT('',(6.,7.4,0.));
#44927=CARTESIAN_POINT('',(6.,5.,0.));
#44928=CARTESIAN_POINT('',(6.,7.4,18.));
#44929=CARTESIAN_POINT('',(6.,7.4,15.75));
#44930=CARTESIAN_POINT('',(6.,5.,18.));
#44931=CARTESIAN_POINT('Origin',(0.,5.,0.));
#44932=CARTESIAN_POINT('',(-6.,7.4,-7.34788079488412E-16));
#44933=CARTESIAN_POINT('',(-6.,5.,-7.34788079488412E-16));
#44934=CARTESIAN_POINT('Origin',(0.,7.4,0.));
#44935=CARTESIAN_POINT('Origin',(0.,5.,9.));
#44936=CARTESIAN_POINT('',(-3.05,5.,18.));
#44937=CARTESIAN_POINT('Origin',(0.,5.,18.));
#44938=CARTESIAN_POINT('',(-3.05,5.,3.73517273739943E-16));
#44939=CARTESIAN_POINT('Origin',(0.,5.,0.));
#44940=CARTESIAN_POINT('Origin',(5.92928932188135,7.57071067811865,15.75));
#44941=CARTESIAN_POINT('',(5.85857864376269,7.74142135623731,0.));
#44942=CARTESIAN_POINT('',(6.,7.4,0.));
#44943=CARTESIAN_POINT('',(5.85857864376269,7.74142135623731,18.));
#44944=CARTESIAN_POINT('',(5.85857864376269,7.74142135623731,15.75));
#44945=CARTESIAN_POINT('',(5.85857864376269,7.74142135623731,18.));
#44946=CARTESIAN_POINT('Origin',(0.,7.57071067811865,1.79367239590926E-16));
#44947=CARTESIAN_POINT('',(-5.85857864376269,7.74142135623731,-7.17468958363702E-16));
#44948=CARTESIAN_POINT('',(-6.,7.4,-7.34788079488412E-16));
#44949=CARTESIAN_POINT('Origin',(0.,7.74142135623731,3.58734479181851E-16));
#44950=CARTESIAN_POINT('Origin',(-5.92928932188135,7.57071067811865,2.25));
#44951=CARTESIAN_POINT('',(-6.,7.4,18.));
#44952=CARTESIAN_POINT('',(-5.85857864376269,7.74142135623731,18.));
#44953=CARTESIAN_POINT('',(-6.,7.4,18.));
#44954=CARTESIAN_POINT('',(-5.85857864376269,7.74142135623731,2.25));
#44955=CARTESIAN_POINT('',(-6.,7.4,2.25));
#44956=CARTESIAN_POINT('Origin',(0.,7.57071067811865,18.));
#44957=CARTESIAN_POINT('Origin',(0.,7.74142135623731,18.));
#44958=CARTESIAN_POINT('Origin',(0.,7.4,18.));
#44959=CARTESIAN_POINT('Origin',(0.,7.8,18.));
#44960=CARTESIAN_POINT('',(5.74142135623731,7.85857864376269,18.));
#44961=CARTESIAN_POINT('',(5.6,8.,18.));
#44962=CARTESIAN_POINT('',(-5.74142135623731,7.85857864376269,18.));
#44963=CARTESIAN_POINT('Origin',(0.,7.85857864376269,18.));
#44964=CARTESIAN_POINT('',(-6.,7.6,18.));
#44965=CARTESIAN_POINT('Origin',(5.8,7.8,13.5));
#44966=CARTESIAN_POINT('',(5.74142135623731,7.85857864376269,0.));
#44967=CARTESIAN_POINT('',(6.,7.6,0.));
#44968=CARTESIAN_POINT('',(5.74142135623731,7.85857864376269,11.25));
#44969=CARTESIAN_POINT('Origin',(5.57071067811865,7.92928932188135,11.25));
#44970=CARTESIAN_POINT('',(5.4,8.,18.));
#44971=CARTESIAN_POINT('',(5.4,8.,18.));
#44972=CARTESIAN_POINT('',(5.4,8.,0.));
#44973=CARTESIAN_POINT('',(5.74142135623731,7.85857864376269,0.));
#44974=CARTESIAN_POINT('',(5.4,8.,11.25));
#44975=CARTESIAN_POINT('Origin',(0.,7.92928932188135,18.));
#44976=CARTESIAN_POINT('',(-5.4,8.,18.));
#44977=CARTESIAN_POINT('',(-5.4,8.,18.));
#44978=CARTESIAN_POINT('Origin',(0.,8.,18.));
#44979=CARTESIAN_POINT('Origin',(-5.57071067811865,7.92928932188135,6.75));
#44980=CARTESIAN_POINT('',(-5.4,8.,-1.11022302462516E-15));
#44981=CARTESIAN_POINT('',(-5.74142135623731,7.85857864376269,-7.03121328647228E-16));
#44982=CARTESIAN_POINT('',(-5.4,8.,-1.11022302462516E-15));
#44983=CARTESIAN_POINT('',(-5.74142135623731,7.85857864376269,6.75));
#44984=CARTESIAN_POINT('',(-5.4,8.,6.75));
#44985=CARTESIAN_POINT('Origin',(0.,7.92928932188135,1.75780332161807E-16));
#44986=CARTESIAN_POINT('Origin',(0.,7.85857864376269,3.51560664323614E-16));
#44987=CARTESIAN_POINT('Origin',(0.,8.,0.));
#44988=CARTESIAN_POINT('Origin',(0.,7.8,0.));
#44989=CARTESIAN_POINT('',(-6.,7.6,-7.34788079488412E-16));
#44990=CARTESIAN_POINT('Origin',(0.,8.,9.));
#44991=CARTESIAN_POINT('',(-3.05,8.,-3.73517273739943E-16));
#44992=CARTESIAN_POINT('Origin',(0.,8.,0.));
#44993=CARTESIAN_POINT('',(-3.05,8.,18.));
#44994=CARTESIAN_POINT('Origin',(0.,8.,18.));
#44995=CARTESIAN_POINT('Origin',(-5.8,7.8,4.5));
#44996=CARTESIAN_POINT('Origin',(0.,4.9,0.));
#44997=CARTESIAN_POINT('',(-3.05,4.9,3.73517273739943E-16));
#44998=CARTESIAN_POINT('Origin',(0.,4.9,18.));
#44999=CARTESIAN_POINT('',(-3.05,4.9,18.));
#45000=CARTESIAN_POINT('Origin',(0.,5.,18.));
#45001=CARTESIAN_POINT('',(-6.,5.,18.));
#45002=CARTESIAN_POINT('Origin',(-6.,5.,0.));
#45003=CARTESIAN_POINT('',(0.,0.,0.));
#45004=CARTESIAN_POINT('Origin',(-15.,2.6,0.));
#45005=CARTESIAN_POINT('',(-15.,-2.6,-3.18408167778312E-16));
#45006=CARTESIAN_POINT('Origin',(-15.,0.,0.));
#45007=CARTESIAN_POINT('Origin',(-14.8,0.,0.));
#45008=CARTESIAN_POINT('',(-14.6,-3.,-3.67394039744206E-16));
#45009=CARTESIAN_POINT('Origin',(-14.6,0.,0.));
#45010=CARTESIAN_POINT('',(-14.8,-2.8,-3.42901103761259E-16));
#45011=CARTESIAN_POINT('Origin',(-13.695,0.,0.));
#45012=CARTESIAN_POINT('',(-12.79,-3.,-3.67394039744206E-16));
#45013=CARTESIAN_POINT('Origin',(-12.79,0.,0.));
#45014=CARTESIAN_POINT('',(-13.695,-3.,-3.67394039744206E-16));
#45015=CARTESIAN_POINT('Origin',(-12.79,2.5,0.));
#45016=CARTESIAN_POINT('',(-12.79,-2.5,-3.06161699786838E-16));
#45017=CARTESIAN_POINT('Origin',(-12.79,0.,0.));
#45018=CARTESIAN_POINT('Origin',(-12.42,0.,0.));
#45019=CARTESIAN_POINT('',(-12.05,-2.5,-3.06161699786838E-16));
#45020=CARTESIAN_POINT('Origin',(-12.05,0.,0.));
#45021=CARTESIAN_POINT('',(-12.42,-2.5,-3.06161699786838E-16));
#45022=CARTESIAN_POINT('Origin',(-12.05,3.,0.));
#45023=CARTESIAN_POINT('',(-12.05,-3.,-3.67394039744206E-16));
#45024=CARTESIAN_POINT('Origin',(-12.05,0.,0.));
#45025=CARTESIAN_POINT('Origin',(0.,0.,0.));
#45026=CARTESIAN_POINT('',(12.05,-3.,-3.67394039744206E-16));
#45027=CARTESIAN_POINT('Origin',(12.05,0.,0.));
#45028=CARTESIAN_POINT('',(0.,-3.,-3.67394039744206E-16));
#45029=CARTESIAN_POINT('Origin',(12.05,2.5,0.));
#45030=CARTESIAN_POINT('',(12.05,-2.5,-3.06161699786838E-16));
#45031=CARTESIAN_POINT('Origin',(12.05,0.,0.));
#45032=CARTESIAN_POINT('Origin',(12.42,0.,0.));
#45033=CARTESIAN_POINT('',(12.79,-2.5,-3.06161699786838E-16));
#45034=CARTESIAN_POINT('Origin',(12.79,0.,0.));
#45035=CARTESIAN_POINT('',(12.42,-2.5,-3.06161699786838E-16));
#45036=CARTESIAN_POINT('Origin',(12.79,3.,0.));
#45037=CARTESIAN_POINT('',(12.79,-3.,-3.67394039744206E-16));
#45038=CARTESIAN_POINT('Origin',(12.79,0.,0.));
#45039=CARTESIAN_POINT('Origin',(13.695,0.,0.));
#45040=CARTESIAN_POINT('',(14.6,-3.,-3.67394039744206E-16));
#45041=CARTESIAN_POINT('Origin',(14.6,0.,0.));
#45042=CARTESIAN_POINT('',(13.695,-3.,-3.67394039744206E-16));
#45043=CARTESIAN_POINT('Origin',(14.8,0.,0.));
#45044=CARTESIAN_POINT('',(15.,-2.6,-3.18408167778312E-16));
#45045=CARTESIAN_POINT('Origin',(15.,0.,0.));
#45046=CARTESIAN_POINT('',(14.8,-2.8,-3.42901103761259E-16));
#45047=CARTESIAN_POINT('Origin',(15.,0.,0.));
#45048=CARTESIAN_POINT('',(0.,0.,0.));
#45049=CARTESIAN_POINT('Origin',(0.,4.705,0.));
#45050=CARTESIAN_POINT('',(-3.61662826400503,4.9,-3.61));
#45051=CARTESIAN_POINT('',(-3.61662826400503,4.9,3.61));
#45052=CARTESIAN_POINT('Origin',(0.,4.9,0.));
#45053=CARTESIAN_POINT('',(-3.77491721763537,4.51,4.));
#45054=CARTESIAN_POINT('Ctrl Pts',(-3.61662826400502,4.9,3.61));
#45055=CARTESIAN_POINT('Ctrl Pts',(-3.67042997577938,4.77027947236335,3.73972052763665));
#45056=CARTESIAN_POINT('Ctrl Pts',(-3.72320339124168,4.64014360909558,3.86985639090442));
#45057=CARTESIAN_POINT('Ctrl Pts',(-3.77491721763537,4.51,4.));
#45058=CARTESIAN_POINT('',(-3.77491721763537,4.51,-4.));
#45059=CARTESIAN_POINT('Origin',(0.,4.51,0.));
#45060=CARTESIAN_POINT('Ctrl Pts',(-3.61662826400502,4.9,-3.61));
#45061=CARTESIAN_POINT('Ctrl Pts',(-3.67042997577939,4.77027947236332,-3.73972052763668));
#45062=CARTESIAN_POINT('Ctrl Pts',(-3.7232033912417,4.64014360909552,-3.86985639090449));
#45063=CARTESIAN_POINT('Ctrl Pts',(-3.77491721763537,4.51,-4.));
#45064=CARTESIAN_POINT('Origin',(-3.5,4.705,3.805));
#45065=CARTESIAN_POINT('',(-6.11,4.9,3.61));
#45066=CARTESIAN_POINT('',(-3.5,4.9,3.61));
#45067=CARTESIAN_POINT('',(-6.5,4.51,4.));
#45068=CARTESIAN_POINT('',(-6.11,4.9,3.61));
#45069=CARTESIAN_POINT('',(-3.5,4.51,4.));
#45070=CARTESIAN_POINT('Origin',(-6.305,4.705,-2.));
#45071=CARTESIAN_POINT('',(-6.11,4.9,-3.61));
#45072=CARTESIAN_POINT('',(-6.11,4.9,-2.));
#45073=CARTESIAN_POINT('',(-6.5,4.51,-4.));
#45074=CARTESIAN_POINT('',(-6.11,4.9,-3.61));
#45075=CARTESIAN_POINT('',(-6.5,4.51,-2.));
#45076=CARTESIAN_POINT('Origin',(-2.13745860881769,4.705,-3.805));
#45077=CARTESIAN_POINT('',(-2.13745860881769,4.51,-4.));
#45078=CARTESIAN_POINT('',(-2.13745860881769,4.9,-3.61));
#45079=CARTESIAN_POINT('Origin',(-3.77491721763537,-4.9,-4.));
#45080=CARTESIAN_POINT('',(-3.77491721763537,-4.51,-4.));
#45081=CARTESIAN_POINT('',(-3.77491721763537,-4.9,-4.));
#45082=CARTESIAN_POINT('',(-6.5,-4.51,-4.));
#45083=CARTESIAN_POINT('',(-2.13745860881769,-4.51,-4.));
#45084=CARTESIAN_POINT('',(-6.5,-4.9,-4.));
#45085=CARTESIAN_POINT('Origin',(0.,-4.9,0.));
#45086=CARTESIAN_POINT('',(-3.77491721763537,-4.51,4.));
#45087=CARTESIAN_POINT('',(-3.77491721763537,-4.9,4.));
#45088=CARTESIAN_POINT('Origin',(0.,-4.51,0.));
#45089=CARTESIAN_POINT('Origin',(-0.499999999999999,4.9,0.));
#45090=CARTESIAN_POINT('',(-3.05,4.9,-3.73517273739943E-16));
#45091=CARTESIAN_POINT('Origin',(0.,4.9,0.));
#45092=CARTESIAN_POINT('Origin',(0.,-4.705,0.));
#45093=CARTESIAN_POINT('',(-3.61662826400503,-4.9,3.61));
#45094=CARTESIAN_POINT('Ctrl Pts',(-3.77491721763537,-4.51,4.));
#45095=CARTESIAN_POINT('Ctrl Pts',(-3.72320339124172,-4.64014360909549,
3.86985639090451));
#45096=CARTESIAN_POINT('Ctrl Pts',(-3.6704299757794,-4.77027947236331,3.73972052763669));
#45097=CARTESIAN_POINT('Ctrl Pts',(-3.61662826400502,-4.9,3.61));
#45098=CARTESIAN_POINT('',(-3.61662826400503,-4.9,-3.61));
#45099=CARTESIAN_POINT('Origin',(0.,-4.9,0.));
#45100=CARTESIAN_POINT('Ctrl Pts',(-3.61662826400502,-4.9,-3.61));
#45101=CARTESIAN_POINT('Ctrl Pts',(-3.6704299757794,-4.77027947236331,-3.73972052763669));
#45102=CARTESIAN_POINT('Ctrl Pts',(-3.72320339124172,-4.64014360909548,
-3.86985639090452));
#45103=CARTESIAN_POINT('Ctrl Pts',(-3.77491721763537,-4.51,-4.));
#45104=CARTESIAN_POINT('Origin',(-2.13745860881769,-4.705,-3.805));
#45105=CARTESIAN_POINT('',(-6.11,-4.9,-3.61));
#45106=CARTESIAN_POINT('',(-2.13745860881769,-4.9,-3.61));
#45107=CARTESIAN_POINT('',(-6.11,-4.9,-3.61));
#45108=CARTESIAN_POINT('Origin',(-6.305,-4.705,-2.));
#45109=CARTESIAN_POINT('',(-6.11,-4.9,3.61));
#45110=CARTESIAN_POINT('',(-6.11,-4.9,-2.));
#45111=CARTESIAN_POINT('',(-6.5,-4.51,4.));
#45112=CARTESIAN_POINT('',(-6.11,-4.9,3.61));
#45113=CARTESIAN_POINT('',(-6.5,-4.51,-2.));
#45114=CARTESIAN_POINT('Origin',(-3.5,-4.705,3.805));
#45115=CARTESIAN_POINT('',(-3.5,-4.51,4.));
#45116=CARTESIAN_POINT('',(-3.5,-4.9,3.61));
#45117=CARTESIAN_POINT('Origin',(-6.5,-4.9,4.));
#45118=CARTESIAN_POINT('',(-6.5,-4.9,4.));
#45119=CARTESIAN_POINT('Origin',(-0.499999999999999,-4.9,0.));
#45120=CARTESIAN_POINT('',(-3.05,-4.9,3.73517273739943E-16));
#45121=CARTESIAN_POINT('Origin',(0.,-4.9,0.));
#45122=CARTESIAN_POINT('Origin',(0.,-5.,0.));
#45123=CARTESIAN_POINT('',(-3.05,-5.,3.73517273739943E-16));
#45124=CARTESIAN_POINT('Origin',(-6.5,-4.9,-4.));
#45125=CARTESIAN_POINT('',(-6.5,-3.99,4.88634072859794E-16));
#45126=CARTESIAN_POINT('Origin',(-6.5,0.,0.));
#45127=CARTESIAN_POINT('Origin',(-34.3,3.49,0.));
#45128=CARTESIAN_POINT('',(-34.3,-3.49,-4.27401732902426E-16));
#45129=CARTESIAN_POINT('Origin',(-34.3,0.,0.));
#45130=CARTESIAN_POINT('Origin',(-34.05,0.,0.));
#45131=CARTESIAN_POINT('',(-33.8,-3.99,-4.88634072859794E-16));
#45132=CARTESIAN_POINT('Origin',(-33.8,0.,0.));
#45133=CARTESIAN_POINT('',(-34.05,-3.74,-4.5801790288111E-16));
#45134=CARTESIAN_POINT('Origin',(-19.4,0.,0.));
#45135=CARTESIAN_POINT('',(-19.4,-3.99,-4.88634072859794E-16));
#45136=CARTESIAN_POINT('',(0.,0.,0.));
#45137=CARTESIAN_POINT('Origin',(0.,-2.63677968348475E-15,-2.77555756156289E-16));
#45138=CARTESIAN_POINT('',(0.,-2.3,4.99599839871872));
#45139=CARTESIAN_POINT('',(0.,2.3,4.99599839871872));
#45140=CARTESIAN_POINT('Origin',(0.,-2.63677968348475E-15,-2.77555756156289E-16));
#45141=CARTESIAN_POINT('',(0.7,2.3,4.99599839871872));
#45142=CARTESIAN_POINT('',(0.,2.3,4.99599839871872));
#45143=CARTESIAN_POINT('',(0.7,-2.3,4.99599839871872));
#45144=CARTESIAN_POINT('Origin',(0.7,-2.63677968348475E-15,-2.77555756156289E-16));
#45145=CARTESIAN_POINT('',(0.,-2.3,4.99599839871872));
#45146=CARTESIAN_POINT('Origin',(0.,-2.3,0.979795897113271));
#45147=CARTESIAN_POINT('',(0.,-2.3,0.979795897113271));
#45148=CARTESIAN_POINT('',(0.,-2.3,4.99599839871872));
#45149=CARTESIAN_POINT('',(0.7,-2.3,0.979795897113271));
#45150=CARTESIAN_POINT('',(0.7,-2.3,4.99599839871872));
#45151=CARTESIAN_POINT('',(0.,-2.3,0.979795897113271));
#45152=CARTESIAN_POINT('Origin',(0.,0.,-1.38777878078145E-16));
#45153=CARTESIAN_POINT('',(0.,2.3,0.979795897113271));
#45154=CARTESIAN_POINT('Origin',(0.,0.,-1.38777878078145E-16));
#45155=CARTESIAN_POINT('',(0.7,2.3,0.979795897113271));
#45156=CARTESIAN_POINT('Origin',(0.7,0.,-1.38777878078145E-16));
#45157=CARTESIAN_POINT('',(0.,2.3,0.979795897113271));
#45158=CARTESIAN_POINT('Origin',(0.,2.3,4.99599839871872));
#45159=CARTESIAN_POINT('',(0.,2.3,4.99599839871872));
#45160=CARTESIAN_POINT('',(0.7,2.3,4.99599839871872));
#45161=CARTESIAN_POINT('Origin',(0.7,-2.22044604925031E-15,-0.25200080064064));
#45162=CARTESIAN_POINT('Origin',(0.,-2.22044604925031E-15,-0.25200080064064));
#45163=CARTESIAN_POINT('',(0.,0.,0.));
#45164=CARTESIAN_POINT('',(0.,0.,0.));
#45165=CARTESIAN_POINT('',(0.,0.,0.));
#45166=CARTESIAN_POINT('',(0.,0.,0.));
#45167=CARTESIAN_POINT('',(95.6,0.,0.));
#45168=CARTESIAN_POINT('',(103.6,0.,0.));
#45169=CARTESIAN_POINT('',(97.1,0.,0.));
#45170=CARTESIAN_POINT('',(10.,0.,0.));
#45171=CARTESIAN_POINT('',(57.,0.,0.));
#45172=CARTESIAN_POINT('',(0.,0.,0.));
#45173=CARTESIAN_POINT('',(72.,0.,0.));
#45174=CARTESIAN_POINT('',(108.,0.,34.));
#45175=CARTESIAN_POINT('',(108.,8.05,34.));
#45176=CARTESIAN_POINT('',(108.,-8.05,34.));
#45177=CARTESIAN_POINT('',(0.,0.,0.));
#45178=CARTESIAN_POINT('',(0.,0.,0.));
#45179=CARTESIAN_POINT('',(0.,0.,0.));
#45180=CARTESIAN_POINT('',(0.,0.,0.));
#45181=CARTESIAN_POINT('',(136.,-14.5,0.));
#45182=CARTESIAN_POINT('',(107.933815006624,0.,51.999878320329));
#45183=CARTESIAN_POINT('',(107.933815006624,0.,51.999878320329));
#45184=CARTESIAN_POINT('',(108.,0.,34.));
#45185=CARTESIAN_POINT('',(108.,0.,34.));
#45186=CARTESIAN_POINT('',(107.933815006624,0.,51.999878320329));
#45187=CARTESIAN_POINT('',(124.,0.,53.3701701719456));
#45188=CARTESIAN_POINT('',(124.,0.,53.3701701719456));
#45189=CARTESIAN_POINT('',(107.933815006624,12.05,51.999878320329));
#45190=CARTESIAN_POINT('',(107.933815006624,-12.05,51.999878320329));
#45191=CARTESIAN_POINT('',(124.,12.05,53.3701701719456));
#45192=CARTESIAN_POINT('',(124.,-12.05,53.3701701719456));
#45193=UNCERTAINTY_MEASURE_WITH_UNIT(LENGTH_MEASURE(0.01),#45237,
'DISTANCE_ACCURACY_VALUE',
'Maximum model space distance between geometric entities at asserted c
onnectivities');
#45194=UNCERTAINTY_MEASURE_WITH_UNIT(LENGTH_MEASURE(0.01),#45237,
'DISTANCE_ACCURACY_VALUE',
'Maximum model space distance between geometric entities at asserted c
onnectivities');
#45195=UNCERTAINTY_MEASURE_WITH_UNIT(LENGTH_MEASURE(0.01),#45237,
'DISTANCE_ACCURACY_VALUE',
'Maximum model space distance between geometric entities at asserted c
onnectivities');
#45196=UNCERTAINTY_MEASURE_WITH_UNIT(LENGTH_MEASURE(0.01),#45237,
'DISTANCE_ACCURACY_VALUE',
'Maximum model space distance between geometric entities at asserted c
onnectivities');
#45197=UNCERTAINTY_MEASURE_WITH_UNIT(LENGTH_MEASURE(0.01),#45237,
'DISTANCE_ACCURACY_VALUE',
'Maximum model space distance between geometric entities at asserted c
onnectivities');
#45198=UNCERTAINTY_MEASURE_WITH_UNIT(LENGTH_MEASURE(0.01),#45237,
'DISTANCE_ACCURACY_VALUE',
'Maximum model space distance between geometric entities at asserted c
onnectivities');
#45199=UNCERTAINTY_MEASURE_WITH_UNIT(LENGTH_MEASURE(0.01),#45237,
'DISTANCE_ACCURACY_VALUE',
'Maximum model space distance between geometric entities at asserted c
onnectivities');
#45200=UNCERTAINTY_MEASURE_WITH_UNIT(LENGTH_MEASURE(0.01),#45237,
'DISTANCE_ACCURACY_VALUE',
'Maximum model space distance between geometric entities at asserted c
onnectivities');
#45201=UNCERTAINTY_MEASURE_WITH_UNIT(LENGTH_MEASURE(0.01),#45237,
'DISTANCE_ACCURACY_VALUE',
'Maximum model space distance between geometric entities at asserted c
onnectivities');
#45202=UNCERTAINTY_MEASURE_WITH_UNIT(LENGTH_MEASURE(0.01),#45237,
'DISTANCE_ACCURACY_VALUE',
'Maximum model space distance between geometric entities at asserted c
onnectivities');
#45203=UNCERTAINTY_MEASURE_WITH_UNIT(LENGTH_MEASURE(0.01),#45237,
'DISTANCE_ACCURACY_VALUE',
'Maximum model space distance between geometric entities at asserted c
onnectivities');
#45204=UNCERTAINTY_MEASURE_WITH_UNIT(LENGTH_MEASURE(0.01),#45237,
'DISTANCE_ACCURACY_VALUE',
'Maximum model space distance between geometric entities at asserted c
onnectivities');
#45205=UNCERTAINTY_MEASURE_WITH_UNIT(LENGTH_MEASURE(0.01),#45237,
'DISTANCE_ACCURACY_VALUE',
'Maximum model space distance between geometric entities at asserted c
onnectivities');
#45206=UNCERTAINTY_MEASURE_WITH_UNIT(LENGTH_MEASURE(0.01),#45237,
'DISTANCE_ACCURACY_VALUE',
'Maximum model space distance between geometric entities at asserted c
onnectivities');
#45207=UNCERTAINTY_MEASURE_WITH_UNIT(LENGTH_MEASURE(0.01),#45237,
'DISTANCE_ACCURACY_VALUE',
'Maximum model space distance between geometric entities at asserted c
onnectivities');
#45208=UNCERTAINTY_MEASURE_WITH_UNIT(LENGTH_MEASURE(0.01),#45237,
'DISTANCE_ACCURACY_VALUE',
'Maximum model space distance between geometric entities at asserted c
onnectivities');
#45209=UNCERTAINTY_MEASURE_WITH_UNIT(LENGTH_MEASURE(0.01),#45237,
'DISTANCE_ACCURACY_VALUE',
'Maximum model space distance between geometric entities at asserted c
onnectivities');
#45210=UNCERTAINTY_MEASURE_WITH_UNIT(LENGTH_MEASURE(0.01),#45237,
'DISTANCE_ACCURACY_VALUE',
'Maximum model space distance between geometric entities at asserted c
onnectivities');
#45211=UNCERTAINTY_MEASURE_WITH_UNIT(LENGTH_MEASURE(0.01),#45237,
'DISTANCE_ACCURACY_VALUE',
'Maximum model space distance between geometric entities at asserted c
onnectivities');
#45212=UNCERTAINTY_MEASURE_WITH_UNIT(LENGTH_MEASURE(0.01),#45237,
'DISTANCE_ACCURACY_VALUE',
'Maximum model space distance between geometric entities at asserted c
onnectivities');
#45213=UNCERTAINTY_MEASURE_WITH_UNIT(LENGTH_MEASURE(0.01),#45237,
'DISTANCE_ACCURACY_VALUE',
'Maximum model space distance between geometric entities at asserted c
onnectivities');
#45214=UNCERTAINTY_MEASURE_WITH_UNIT(LENGTH_MEASURE(0.01),#45237,
'DISTANCE_ACCURACY_VALUE',
'Maximum model space distance between geometric entities at asserted c
onnectivities');
#45215=(
GEOMETRIC_REPRESENTATION_CONTEXT(3)
GLOBAL_UNCERTAINTY_ASSIGNED_CONTEXT((#45193))
GLOBAL_UNIT_ASSIGNED_CONTEXT((#45237,#45239,#45240))
REPRESENTATION_CONTEXT('','3D')
);
#45216=(
GEOMETRIC_REPRESENTATION_CONTEXT(3)
GLOBAL_UNCERTAINTY_ASSIGNED_CONTEXT((#45194))
GLOBAL_UNIT_ASSIGNED_CONTEXT((#45237,#45239,#45240))
REPRESENTATION_CONTEXT('','3D')
);
#45217=(
GEOMETRIC_REPRESENTATION_CONTEXT(3)
GLOBAL_UNCERTAINTY_ASSIGNED_CONTEXT((#45195))
GLOBAL_UNIT_ASSIGNED_CONTEXT((#45237,#45239,#45240))
REPRESENTATION_CONTEXT('','3D')
);
#45218=(
GEOMETRIC_REPRESENTATION_CONTEXT(3)
GLOBAL_UNCERTAINTY_ASSIGNED_CONTEXT((#45196))
GLOBAL_UNIT_ASSIGNED_CONTEXT((#45237,#45239,#45240))
REPRESENTATION_CONTEXT('','3D')
);
#45219=(
GEOMETRIC_REPRESENTATION_CONTEXT(3)
GLOBAL_UNCERTAINTY_ASSIGNED_CONTEXT((#45197))
GLOBAL_UNIT_ASSIGNED_CONTEXT((#45237,#45239,#45240))
REPRESENTATION_CONTEXT('','3D')
);
#45220=(
GEOMETRIC_REPRESENTATION_CONTEXT(3)
GLOBAL_UNCERTAINTY_ASSIGNED_CONTEXT((#45198))
GLOBAL_UNIT_ASSIGNED_CONTEXT((#45237,#45239,#45240))
REPRESENTATION_CONTEXT('','3D')
);
#45221=(
GEOMETRIC_REPRESENTATION_CONTEXT(3)
GLOBAL_UNCERTAINTY_ASSIGNED_CONTEXT((#45199))
GLOBAL_UNIT_ASSIGNED_CONTEXT((#45237,#45239,#45240))
REPRESENTATION_CONTEXT('','3D')
);
#45222=(
GEOMETRIC_REPRESENTATION_CONTEXT(3)
GLOBAL_UNCERTAINTY_ASSIGNED_CONTEXT((#45200))
GLOBAL_UNIT_ASSIGNED_CONTEXT((#45237,#45239,#45240))
REPRESENTATION_CONTEXT('','3D')
);
#45223=(
GEOMETRIC_REPRESENTATION_CONTEXT(3)
GLOBAL_UNCERTAINTY_ASSIGNED_CONTEXT((#45201))
GLOBAL_UNIT_ASSIGNED_CONTEXT((#45237,#45239,#45240))
REPRESENTATION_CONTEXT('','3D')
);
#45224=(
GEOMETRIC_REPRESENTATION_CONTEXT(3)
GLOBAL_UNCERTAINTY_ASSIGNED_CONTEXT((#45202))
GLOBAL_UNIT_ASSIGNED_CONTEXT((#45237,#45239,#45240))
REPRESENTATION_CONTEXT('','3D')
);
#45225=(
GEOMETRIC_REPRESENTATION_CONTEXT(3)
GLOBAL_UNCERTAINTY_ASSIGNED_CONTEXT((#45203))
GLOBAL_UNIT_ASSIGNED_CONTEXT((#45237,#45239,#45240))
REPRESENTATION_CONTEXT('','3D')
);
#45226=(
GEOMETRIC_REPRESENTATION_CONTEXT(3)
GLOBAL_UNCERTAINTY_ASSIGNED_CONTEXT((#45204))
GLOBAL_UNIT_ASSIGNED_CONTEXT((#45237,#45239,#45240))
REPRESENTATION_CONTEXT('','3D')
);
#45227=(
GEOMETRIC_REPRESENTATION_CONTEXT(3)
GLOBAL_UNCERTAINTY_ASSIGNED_CONTEXT((#45205))
GLOBAL_UNIT_ASSIGNED_CONTEXT((#45237,#45239,#45240))
REPRESENTATION_CONTEXT('','3D')
);
#45228=(
GEOMETRIC_REPRESENTATION_CONTEXT(3)
GLOBAL_UNCERTAINTY_ASSIGNED_CONTEXT((#45206))
GLOBAL_UNIT_ASSIGNED_CONTEXT((#45237,#45239,#45240))
REPRESENTATION_CONTEXT('','3D')
);
#45229=(
GEOMETRIC_REPRESENTATION_CONTEXT(3)
GLOBAL_UNCERTAINTY_ASSIGNED_CONTEXT((#45207))
GLOBAL_UNIT_ASSIGNED_CONTEXT((#45237,#45239,#45240))
REPRESENTATION_CONTEXT('','3D')
);
#45230=(
GEOMETRIC_REPRESENTATION_CONTEXT(3)
GLOBAL_UNCERTAINTY_ASSIGNED_CONTEXT((#45208))
GLOBAL_UNIT_ASSIGNED_CONTEXT((#45237,#45239,#45240))
REPRESENTATION_CONTEXT('','3D')
);
#45231=(
GEOMETRIC_REPRESENTATION_CONTEXT(3)
GLOBAL_UNCERTAINTY_ASSIGNED_CONTEXT((#45209))
GLOBAL_UNIT_ASSIGNED_CONTEXT((#45237,#45239,#45240))
REPRESENTATION_CONTEXT('','3D')
);
#45232=(
GEOMETRIC_REPRESENTATION_CONTEXT(3)
GLOBAL_UNCERTAINTY_ASSIGNED_CONTEXT((#45210))
GLOBAL_UNIT_ASSIGNED_CONTEXT((#45237,#45239,#45240))
REPRESENTATION_CONTEXT('','3D')
);
#45233=(
GEOMETRIC_REPRESENTATION_CONTEXT(3)
GLOBAL_UNCERTAINTY_ASSIGNED_CONTEXT((#45211))
GLOBAL_UNIT_ASSIGNED_CONTEXT((#45237,#45239,#45240))
REPRESENTATION_CONTEXT('','3D')
);
#45234=(
GEOMETRIC_REPRESENTATION_CONTEXT(3)
GLOBAL_UNCERTAINTY_ASSIGNED_CONTEXT((#45212))
GLOBAL_UNIT_ASSIGNED_CONTEXT((#45237,#45239,#45240))
REPRESENTATION_CONTEXT('','3D')
);
#45235=(
GEOMETRIC_REPRESENTATION_CONTEXT(3)
GLOBAL_UNCERTAINTY_ASSIGNED_CONTEXT((#45213))
GLOBAL_UNIT_ASSIGNED_CONTEXT((#45237,#45239,#45240))
REPRESENTATION_CONTEXT('','3D')
);
#45236=(
GEOMETRIC_REPRESENTATION_CONTEXT(3)
GLOBAL_UNCERTAINTY_ASSIGNED_CONTEXT((#45214))
GLOBAL_UNIT_ASSIGNED_CONTEXT((#45237,#45239,#45240))
REPRESENTATION_CONTEXT('','3D')
);
#45237=(
LENGTH_UNIT()
NAMED_UNIT(*)
SI_UNIT(.MILLI.,.METRE.)
);
#45238=(
LENGTH_UNIT()
NAMED_UNIT(*)
SI_UNIT($,.METRE.)
);
#45239=(
NAMED_UNIT(*)
PLANE_ANGLE_UNIT()
SI_UNIT($,.RADIAN.)
);
#45240=(
NAMED_UNIT(*)
SI_UNIT($,.STERADIAN.)
SOLID_ANGLE_UNIT()
);
#45241=SHAPE_DEFINITION_REPRESENTATION(#45262,#45313);
#45242=SHAPE_DEFINITION_REPRESENTATION(#45263,#45314);
#45243=SHAPE_DEFINITION_REPRESENTATION(#45264,#45315);
#45244=SHAPE_DEFINITION_REPRESENTATION(#45265,#45316);
#45245=SHAPE_DEFINITION_REPRESENTATION(#45266,#45317);
#45246=SHAPE_DEFINITION_REPRESENTATION(#45267,#45318);
#45247=SHAPE_DEFINITION_REPRESENTATION(#45268,#45319);
#45248=SHAPE_DEFINITION_REPRESENTATION(#45269,#45320);
#45249=SHAPE_DEFINITION_REPRESENTATION(#45270,#45321);
#45250=SHAPE_DEFINITION_REPRESENTATION(#45271,#45322);
#45251=SHAPE_DEFINITION_REPRESENTATION(#45272,#45323);
#45252=SHAPE_DEFINITION_REPRESENTATION(#45273,#45324);
#45253=SHAPE_DEFINITION_REPRESENTATION(#45274,#45325);
#45254=SHAPE_DEFINITION_REPRESENTATION(#45275,#45326);
#45255=SHAPE_DEFINITION_REPRESENTATION(#45276,#45327);
#45256=SHAPE_DEFINITION_REPRESENTATION(#45277,#45328);
#45257=SHAPE_DEFINITION_REPRESENTATION(#45278,#45329);
#45258=SHAPE_DEFINITION_REPRESENTATION(#45279,#45330);
#45259=SHAPE_DEFINITION_REPRESENTATION(#45280,#45331);
#45260=SHAPE_DEFINITION_REPRESENTATION(#45281,#45332);
#45261=SHAPE_DEFINITION_REPRESENTATION(#45282,#45333);
#45262=PRODUCT_DEFINITION_SHAPE('',$,#45335);
#45263=PRODUCT_DEFINITION_SHAPE('',$,#45336);
#45264=PRODUCT_DEFINITION_SHAPE('',$,#45337);
#45265=PRODUCT_DEFINITION_SHAPE('',$,#45338);
#45266=PRODUCT_DEFINITION_SHAPE('',$,#45339);
#45267=PRODUCT_DEFINITION_SHAPE('',$,#45340);
#45268=PRODUCT_DEFINITION_SHAPE('',$,#45341);
#45269=PRODUCT_DEFINITION_SHAPE('',$,#45342);
#45270=PRODUCT_DEFINITION_SHAPE('',$,#45343);
#45271=PRODUCT_DEFINITION_SHAPE('',$,#45344);
#45272=PRODUCT_DEFINITION_SHAPE('',$,#45345);
#45273=PRODUCT_DEFINITION_SHAPE('',$,#45346);
#45274=PRODUCT_DEFINITION_SHAPE('',$,#45347);
#45275=PRODUCT_DEFINITION_SHAPE('',$,#45348);
#45276=PRODUCT_DEFINITION_SHAPE('',$,#45349);
#45277=PRODUCT_DEFINITION_SHAPE('',$,#45350);
#45278=PRODUCT_DEFINITION_SHAPE('',$,#45351);
#45279=PRODUCT_DEFINITION_SHAPE('',$,#45352);
#45280=PRODUCT_DEFINITION_SHAPE('',$,#45353);
#45281=PRODUCT_DEFINITION_SHAPE('',$,#45354);
#45282=PRODUCT_DEFINITION_SHAPE('',$,#45355);
#45283=PRODUCT_DEFINITION_SHAPE($,$,#101);
#45284=PRODUCT_DEFINITION_SHAPE($,$,#102);
#45285=PRODUCT_DEFINITION_SHAPE($,$,#103);
#45286=PRODUCT_DEFINITION_SHAPE($,$,#104);
#45287=PRODUCT_DEFINITION_SHAPE($,$,#105);
#45288=PRODUCT_DEFINITION_SHAPE($,$,#106);
#45289=PRODUCT_DEFINITION_SHAPE($,$,#107);
#45290=PRODUCT_DEFINITION_SHAPE($,$,#108);
#45291=PRODUCT_DEFINITION_SHAPE($,$,#109);
#45292=PRODUCT_DEFINITION_SHAPE($,$,#110);
#45293=PRODUCT_DEFINITION_SHAPE($,$,#111);
#45294=PRODUCT_DEFINITION_SHAPE($,$,#112);
#45295=PRODUCT_DEFINITION_SHAPE($,$,#113);
#45296=PRODUCT_DEFINITION_SHAPE($,$,#114);
#45297=PRODUCT_DEFINITION_SHAPE($,$,#115);
#45298=PRODUCT_DEFINITION_SHAPE($,$,#116);
#45299=PRODUCT_DEFINITION_SHAPE($,$,#117);
#45300=PRODUCT_DEFINITION_SHAPE($,$,#118);
#45301=PRODUCT_DEFINITION_SHAPE($,$,#119);
#45302=PRODUCT_DEFINITION_SHAPE($,$,#120);
#45303=PRODUCT_DEFINITION_SHAPE($,$,#121);
#45304=PRODUCT_DEFINITION_SHAPE($,$,#122);
#45305=PRODUCT_DEFINITION_SHAPE($,$,#123);
#45306=PRODUCT_DEFINITION_SHAPE($,$,#124);
#45307=PRODUCT_DEFINITION_SHAPE($,$,#125);
#45308=PRODUCT_DEFINITION_SHAPE($,$,#126);
#45309=PRODUCT_DEFINITION_SHAPE($,$,#127);
#45310=PRODUCT_DEFINITION_SHAPE($,$,#128);
#45311=PRODUCT_DEFINITION_SHAPE($,$,#129);
#45312=PRODUCT_DEFINITION_SHAPE($,$,#130);
#45313=SHAPE_REPRESENTATION('',(#16758,#18093,#18094,#18095,#18096,#18097,
#18098,#18099,#18100,#18101,#18102,#18103,#18104,#18105,#18106,#18107,#18108,
#18109,#18110,#18111,#18112,#18113,#18114,#18115,#18116,#18117,#18118,#18119,
#18120,#18121,#18122),#45215);
#45314=SHAPE_REPRESENTATION('',(#16759),#45216);
#45315=SHAPE_REPRESENTATION('',(#16969),#45217);
#45316=SHAPE_REPRESENTATION('',(#17111),#45218);
#45317=SHAPE_REPRESENTATION('',(#17147),#45219);
#45318=SHAPE_REPRESENTATION('',(#17152),#45220);
#45319=SHAPE_REPRESENTATION('',(#17156),#45221);
#45320=SHAPE_REPRESENTATION('',(#17165),#45222);
#45321=SHAPE_REPRESENTATION('',(#17175),#45223);
#45322=SHAPE_REPRESENTATION('',(#17253),#45224);
#45323=SHAPE_REPRESENTATION('',(#17279),#45225);
#45324=SHAPE_REPRESENTATION('',(#17342),#45226);
#45325=SHAPE_REPRESENTATION('',(#17551),#45227);
#45326=SHAPE_REPRESENTATION('',(#17572),#45228);
#45327=SHAPE_REPRESENTATION('',(#17601),#45229);
#45328=SHAPE_REPRESENTATION('',(#17879),#45230);
#45329=SHAPE_REPRESENTATION('',(#17958),#45231);
#45330=SHAPE_REPRESENTATION('',(#17987),#45232);
#45331=SHAPE_REPRESENTATION('',(#18028),#45233);
#45332=SHAPE_REPRESENTATION('',(#18054),#45234);
#45333=SHAPE_REPRESENTATION('',(#18082),#45235);
#45334=PRODUCT_DEFINITION_CONTEXT('part definition',#45399,'design');
#45335=PRODUCT_DEFINITION('2026-10-25-23-38-09-980','MAS-329',#45356,#45334);
#45336=PRODUCT_DEFINITION('2026-10-25-23-38-11-368',
'01_Pincer_Head_C-Frame',#45357,#45334);
#45337=PRODUCT_DEFINITION('2026-10-25-23-38-13-511',
'02_Hydraulic_Cylinder_Body',#45358,#45334);
#45338=PRODUCT_DEFINITION('2026-10-25-23-38-15-275','03_Ram_Piston_D36',
#45359,#45334);
#45339=PRODUCT_DEFINITION('2026-10-25-23-38-15-879',
'04_Piston_Return_Spring_D33x1.6',#45360,#45334);
#45340=PRODUCT_DEFINITION('2026-10-25-23-38-16-850',
'05_O-Ring_30x3.1_NBR',#45361,#45334);
#45341=PRODUCT_DEFINITION('2026-10-25-23-38-17-064',
'06_Backup_Ring_30x2_PTFE',#45362,#45334);
#45342=PRODUCT_DEFINITION('2026-10-25-23-38-17-379',
'07_Die_Magnet_D6x5_NdFeB',#45363,#45334);
#45343=PRODUCT_DEFINITION('2026-10-25-23-38-17-681',
'08_Crimping_Die_10_AWG',#45364,#45334);
#45344=PRODUCT_DEFINITION('2026-10-25-23-38-20-461',
'11_Handle_Pin_D6x22',#45365,#45334);
#45345=PRODUCT_DEFINITION('2026-10-25-23-38-26-010',
'16_Fount_Oil_Reservoir',#45366,#45334);
#45346=PRODUCT_DEFINITION('2026-10-25-23-38-26-935',
'17_Faucet_Oil_Filler_Screw_M10x1',#45367,#45334);
#45347=PRODUCT_DEFINITION('2026-10-25-23-38-28-911',
'18_Fixed_Handle_Tube',#45368,#45334);
#45348=PRODUCT_DEFINITION('2026-10-25-23-38-29-621',
'19_Fixed_Handle_Grip',#45369,#45334);
#45349=PRODUCT_DEFINITION('2026-10-25-23-38-30-333',
'20_Oil_Return_Valve_Knob_M10x1',#45370,#45334);
#45350=PRODUCT_DEFINITION('2026-10-25-23-38-22-272','14_Pump_Handle',#45371,
#45334);
#45351=PRODUCT_DEFINITION('2026-10-25-23-38-24-602',
'15_Pump_Handle_Grip',#45372,#45334);
#45352=PRODUCT_DEFINITION('2026-10-25-23-38-19-262',
'09_Plank_Link_Plate',#45373,#45334);
#45353=PRODUCT_DEFINITION('2026-10-25-23-38-19-947',
'10_Handle_Pin_D6x30',#45374,#45334);
#45354=PRODUCT_DEFINITION('2026-10-25-23-38-21-279',
'13_Injection_Piston_D8',#45375,#45334);
#45355=PRODUCT_DEFINITION('2026-10-25-23-38-20-982',
'12_E-Clip_DIN_6799_-_5',#45376,#45334);
#45356=PRODUCT_DEFINITION_FORMATION('',$,#45401);
#45357=PRODUCT_DEFINITION_FORMATION('',$,#45402);
#45358=PRODUCT_DEFINITION_FORMATION('',$,#45403);
#45359=PRODUCT_DEFINITION_FORMATION('',$,#45404);
#45360=PRODUCT_DEFINITION_FORMATION('',$,#45405);
#45361=PRODUCT_DEFINITION_FORMATION('',$,#45406);
#45362=PRODUCT_DEFINITION_FORMATION('',$,#45407);
#45363=PRODUCT_DEFINITION_FORMATION('',$,#45408);
#45364=PRODUCT_DEFINITION_FORMATION('',$,#45409);
#45365=PRODUCT_DEFINITION_FORMATION('',$,#45410);
#45366=PRODUCT_DEFINITION_FORMATION('',$,#45411);
#45367=PRODUCT_DEFINITION_FORMATION('',$,#45412);
#45368=PRODUCT_DEFINITION_FORMATION('',$,#45413);
#45369=PRODUCT_DEFINITION_FORMATION('',$,#45414);
#45370=PRODUCT_DEFINITION_FORMATION('',$,#45415);
#45371=PRODUCT_DEFINITION_FORMATION('',$,#45416);
#45372=PRODUCT_DEFINITION_FORMATION('',$,#45417);
#45373=PRODUCT_DEFINITION_FORMATION('',$,#45418);
#45374=PRODUCT_DEFINITION_FORMATION('',$,#45419);
#45375=PRODUCT_DEFINITION_FORMATION('',$,#45420);
#45376=PRODUCT_DEFINITION_FORMATION('',$,#45421);
#45377=PRODUCT_RELATED_PRODUCT_CATEGORY('MAS-329','MAS-329',(#45401));
#45378=PRODUCT_RELATED_PRODUCT_CATEGORY('01_Pincer_Head_C-Frame',
'01_Pincer_Head_C-Frame',(#45402));
#45379=PRODUCT_RELATED_PRODUCT_CATEGORY('02_Hydraulic_Cylinder_Body',
'02_Hydraulic_Cylinder_Body',(#45403));
#45380=PRODUCT_RELATED_PRODUCT_CATEGORY('03_Ram_Piston_D36',
'03_Ram_Piston_D36',(#45404));
#45381=PRODUCT_RELATED_PRODUCT_CATEGORY(
'04_Piston_Return_Spring_D33x1.6','04_Piston_Return_Spring_D33x1.6',(#45405));
#45382=PRODUCT_RELATED_PRODUCT_CATEGORY('05_O-Ring_30x3.1_NBR',
'05_O-Ring_30x3.1_NBR',(#45406));
#45383=PRODUCT_RELATED_PRODUCT_CATEGORY('06_Backup_Ring_30x2_PTFE',
'06_Backup_Ring_30x2_PTFE',(#45407));
#45384=PRODUCT_RELATED_PRODUCT_CATEGORY('07_Die_Magnet_D6x5_NdFeB',
'07_Die_Magnet_D6x5_NdFeB',(#45408));
#45385=PRODUCT_RELATED_PRODUCT_CATEGORY('08_Crimping_Die_10_AWG',
'08_Crimping_Die_10_AWG',(#45409));
#45386=PRODUCT_RELATED_PRODUCT_CATEGORY('11_Handle_Pin_D6x22',
'11_Handle_Pin_D6x22',(#45410));
#45387=PRODUCT_RELATED_PRODUCT_CATEGORY('16_Fount_Oil_Reservoir',
'16_Fount_Oil_Reservoir',(#45411));
#45388=PRODUCT_RELATED_PRODUCT_CATEGORY(
'17_Faucet_Oil_Filler_Screw_M10x1','17_Faucet_Oil_Filler_Screw_M10x1',(#45412));
#45389=PRODUCT_RELATED_PRODUCT_CATEGORY('18_Fixed_Handle_Tube',
'18_Fixed_Handle_Tube',(#45413));
#45390=PRODUCT_RELATED_PRODUCT_CATEGORY('19_Fixed_Handle_Grip',
'19_Fixed_Handle_Grip',(#45414));
#45391=PRODUCT_RELATED_PRODUCT_CATEGORY(
'20_Oil_Return_Valve_Knob_M10x1','20_Oil_Return_Valve_Knob_M10x1',(#45415));
#45392=PRODUCT_RELATED_PRODUCT_CATEGORY('14_Pump_Handle',
'14_Pump_Handle',(#45416));
#45393=PRODUCT_RELATED_PRODUCT_CATEGORY('15_Pump_Handle_Grip',
'15_Pump_Handle_Grip',(#45417));
#45394=PRODUCT_RELATED_PRODUCT_CATEGORY('09_Plank_Link_Plate',
'09_Plank_Link_Plate',(#45418));
#45395=PRODUCT_RELATED_PRODUCT_CATEGORY('10_Handle_Pin_D6x30',
'10_Handle_Pin_D6x30',(#45419));
#45396=PRODUCT_RELATED_PRODUCT_CATEGORY('13_Injection_Piston_D8',
'13_Injection_Piston_D8',(#45420));
#45397=PRODUCT_RELATED_PRODUCT_CATEGORY('12_E-Clip_DIN_6799_-_5',
'12_E-Clip_DIN_6799_-_5',(#45421));
#45398=APPLICATION_PROTOCOL_DEFINITION('international standard',
'automotive_design',2009,#45399);
#45399=APPLICATION_CONTEXT(
'Core Data for Automotive Mechanical Design Process');
#45400=PRODUCT_CONTEXT('part definition',#45399,'mechanical');
#45401=PRODUCT('2026-10-25-23-38-09-980','MAS-329',$,(#45400));
#45402=PRODUCT('2026-10-25-23-38-11-368','01_Pincer_Head_C-Frame',$,(#45400));
#45403=PRODUCT('2026-10-25-23-38-13-511','02_Hydraulic_Cylinder_Body',$,
(#45400));
#45404=PRODUCT('2026-10-25-23-38-15-275','03_Ram_Piston_D36',$,(#45400));
#45405=PRODUCT('2026-10-25-23-38-15-879',
'04_Piston_Return_Spring_D33x1.6',$,(#45400));
#45406=PRODUCT('2026-10-25-23-38-16-850','05_O-Ring_30x3.1_NBR',$,(#45400));
#45407=PRODUCT('2026-10-25-23-38-17-064','06_Backup_Ring_30x2_PTFE',$,(#45400));
#45408=PRODUCT('2026-10-25-23-38-17-379','07_Die_Magnet_D6x5_NdFeB',$,(#45400));
#45409=PRODUCT('2026-10-25-23-38-17-681','08_Crimping_Die_10_AWG',$,(#45400));
#45410=PRODUCT('2026-10-25-23-38-20-461','11_Handle_Pin_D6x22',$,(#45400));
#45411=PRODUCT('2026-10-25-23-38-26-010','16_Fount_Oil_Reservoir',$,(#45400));
#45412=PRODUCT('2026-10-25-23-38-26-935',
'17_Faucet_Oil_Filler_Screw_M10x1',$,(#45400));
#45413=PRODUCT('2026-10-25-23-38-28-911','18_Fixed_Handle_Tube',$,(#45400));
#45414=PRODUCT('2026-10-25-23-38-29-621','19_Fixed_Handle_Grip',$,(#45400));
#45415=PRODUCT('2026-10-25-23-38-30-333',
'20_Oil_Return_Valve_Knob_M10x1',$,(#45400));
#45416=PRODUCT('2026-10-25-23-38-22-272','14_Pump_Handle',$,(#45400));
#45417=PRODUCT('2026-10-25-23-38-24-602','15_Pump_Handle_Grip',$,(#45400));
#45418=PRODUCT('2026-10-25-23-38-19-262','09_Plank_Link_Plate',$,(#45400));
#45419=PRODUCT('2026-10-25-23-38-19-947','10_Handle_Pin_D6x30',$,(#45400));
#45420=PRODUCT('2026-10-25-23-38-21-279','13_Injection_Piston_D8',$,(#45400));
#45421=PRODUCT('2026-10-25-23-38-20-982','12_E-Clip_DIN_6799_-_5',$,(#45400));
#45422=PRESENTATION_STYLE_ASSIGNMENT((#45427));
#45423=PRESENTATION_STYLE_ASSIGNMENT((#45428));
#45424=PRESENTATION_STYLE_ASSIGNMENT((#45429));
#45425=PRESENTATION_STYLE_ASSIGNMENT((#45430));
#45426=PRESENTATION_STYLE_ASSIGNMENT((#45431));
#45427=SURFACE_STYLE_USAGE(.BOTH.,#45432);
#45428=SURFACE_STYLE_USAGE(.BOTH.,#45433);
#45429=SURFACE_STYLE_USAGE(.BOTH.,#45434);
#45430=SURFACE_STYLE_USAGE(.BOTH.,#45435);
#45431=SURFACE_STYLE_USAGE(.BOTH.,#45436);
#45432=SURFACE_SIDE_STYLE('',(#45437));
#45433=SURFACE_SIDE_STYLE('',(#45438));
#45434=SURFACE_SIDE_STYLE('',(#45439));
#45435=SURFACE_SIDE_STYLE('',(#45440));
#45436=SURFACE_SIDE_STYLE('',(#45441));
#45437=SURFACE_STYLE_FILL_AREA(#45442);
#45438=SURFACE_STYLE_FILL_AREA(#45443);
#45439=SURFACE_STYLE_FILL_AREA(#45444);
#45440=SURFACE_STYLE_FILL_AREA(#45445);
#45441=SURFACE_STYLE_FILL_AREA(#45446);
#45442=FILL_AREA_STYLE('Steel - Satin',(#45447));
#45443=FILL_AREA_STYLE('MAS496_gun',(#45448));
#45444=FILL_AREA_STYLE('MAS496_ss',(#45449));
#45445=FILL_AREA_STYLE('MAS496_ti',(#45450));
#45446=FILL_AREA_STYLE('MAS496_al',(#45451));
#45447=FILL_AREA_STYLE_COLOUR('Steel - Satin',#45452);
#45448=FILL_AREA_STYLE_COLOUR('MAS496_gun',#45453);
#45449=FILL_AREA_STYLE_COLOUR('MAS496_ss',#45454);
#45450=FILL_AREA_STYLE_COLOUR('MAS496_ti',#45455);
#45451=FILL_AREA_STYLE_COLOUR('MAS496_al',#45456);
#45452=COLOUR_RGB('Steel - Satin',0.627450980392157,0.627450980392157,0.627450980392157);
#45453=COLOUR_RGB('MAS496_gun',0.313725490196078,0.337254901960784,0.364705882352941);
#45454=COLOUR_RGB('MAS496_ss',0.83921568627451,0.850980392156863,0.862745098039216);
#45455=COLOUR_RGB('MAS496_ti',0.549019607843137,0.572549019607843,0.596078431372549);
#45456=COLOUR_RGB('MAS496_al',0.67843137254902,0.705882352941177,0.729411764705882);
#45457=COLOUR_RGB('Dark Blue',0.08,0.2,0.34);
#45458=FILL_AREA_STYLE_COLOUR('',#45457);
#45459=FILL_AREA_STYLE('',(#45458));
#45460=SURFACE_STYLE_FILL_AREA(#45459);
#45461=SURFACE_SIDE_STYLE('',(#45460));
#45462=SURFACE_STYLE_USAGE(.BOTH.,#45461);
#45463=PRESENTATION_STYLE_ASSIGNMENT((#45462));
#45464=COLOUR_RGB('Light Blue',0.38,0.62,0.78);
#45465=FILL_AREA_STYLE_COLOUR('',#45464);
#45466=FILL_AREA_STYLE('',(#45465));
#45467=SURFACE_STYLE_FILL_AREA(#45466);
#45468=SURFACE_SIDE_STYLE('',(#45467));
#45469=SURFACE_STYLE_USAGE(.BOTH.,#45468);
#45470=PRESENTATION_STYLE_ASSIGNMENT((#45469));
#45471=COLOUR_RGB('Sky Blue',0.24,0.69,0.87);
#45472=FILL_AREA_STYLE_COLOUR('',#45471);
#45473=FILL_AREA_STYLE('',(#45472));
#45474=SURFACE_STYLE_FILL_AREA(#45473);
#45475=SURFACE_SIDE_STYLE('',(#45474));
#45476=SURFACE_STYLE_USAGE(.BOTH.,#45475);
#45477=PRESENTATION_STYLE_ASSIGNMENT((#45476));
#45478=COLOUR_RGB('Grey',0.48,0.52,0.57);
#45479=FILL_AREA_STYLE_COLOUR('',#45478);
#45480=FILL_AREA_STYLE('',(#45479));
#45481=SURFACE_STYLE_FILL_AREA(#45480);
#45482=SURFACE_SIDE_STYLE('',(#45481));
#45483=SURFACE_STYLE_USAGE(.BOTH.,#45482);
#45484=PRESENTATION_STYLE_ASSIGNMENT((#45483));
#45485=COLOUR_RGB('Black',0.12,0.14,0.17);
#45486=FILL_AREA_STYLE_COLOUR('',#45485);
#45487=FILL_AREA_STYLE('',(#45486));
#45488=SURFACE_STYLE_FILL_AREA(#45487);
#45489=SURFACE_SIDE_STYLE('',(#45488));
#45490=SURFACE_STYLE_USAGE(.BOTH.,#45489);
#45491=PRESENTATION_STYLE_ASSIGNMENT((#45490));
#45492=COLOUR_RGB('Off White',0.89,0.88,0.83);
#45493=FILL_AREA_STYLE_COLOUR('',#45492);
#45494=FILL_AREA_STYLE('',(#45493));
#45495=SURFACE_STYLE_FILL_AREA(#45494);
#45496=SURFACE_SIDE_STYLE('',(#45495));
#45497=SURFACE_STYLE_USAGE(.BOTH.,#45496);
#45498=PRESENTATION_STYLE_ASSIGNMENT((#45497));
ENDSEC;
END-ISO-10303-21;
